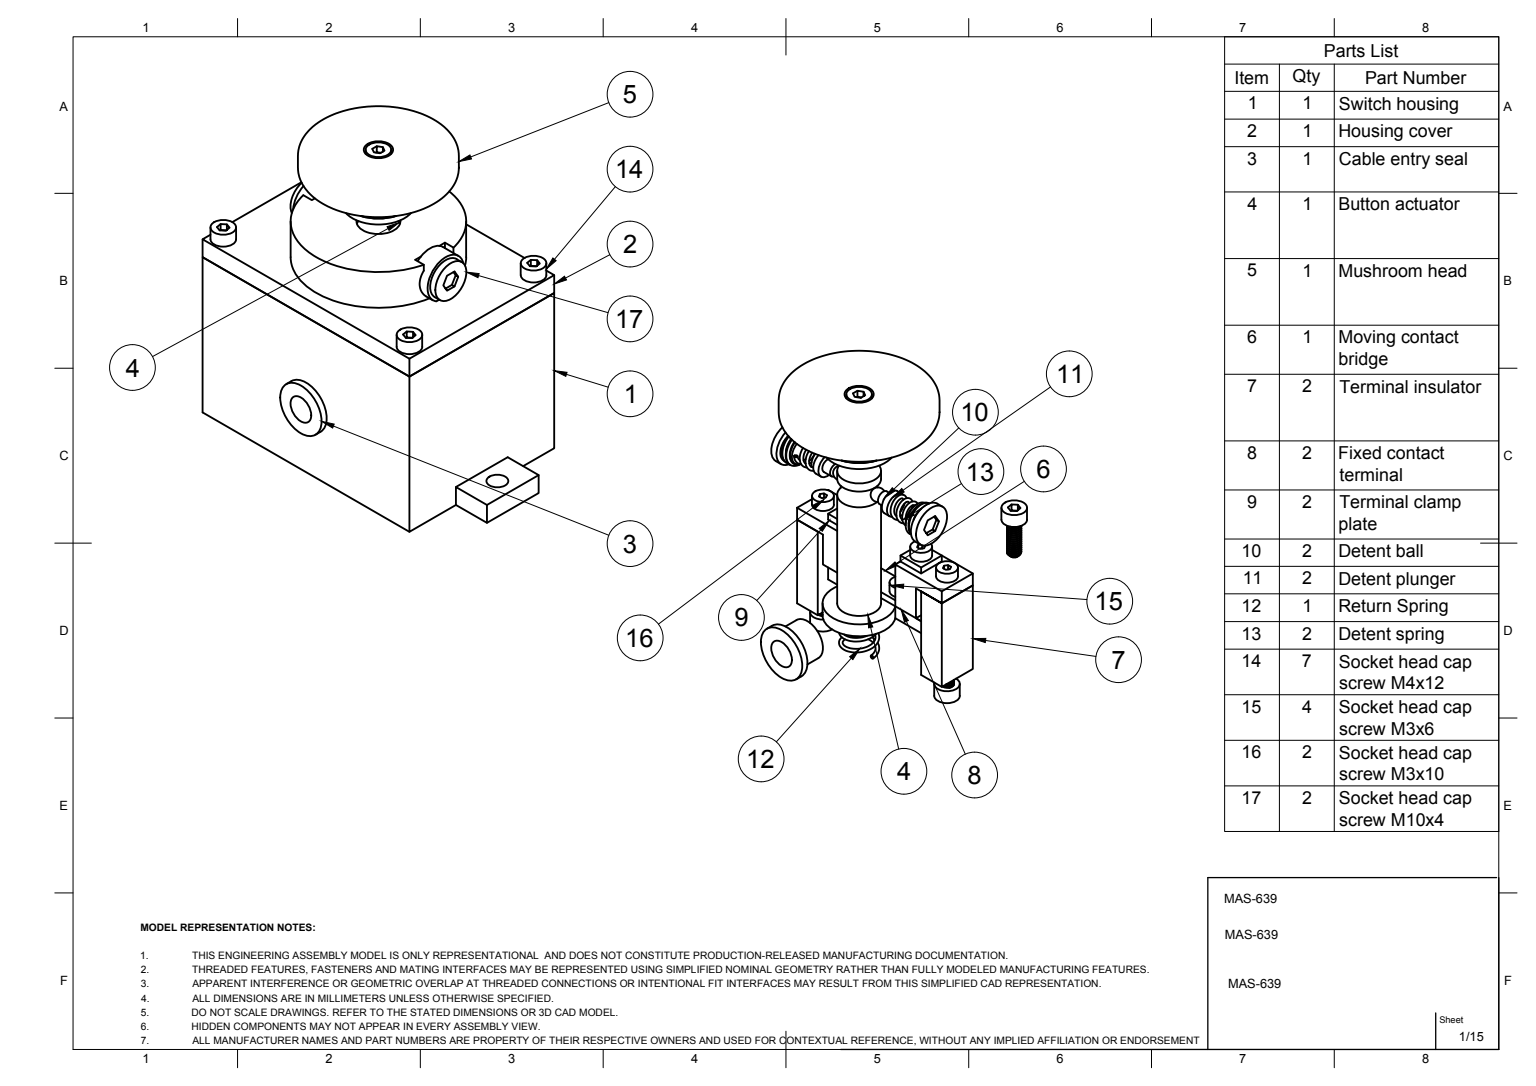
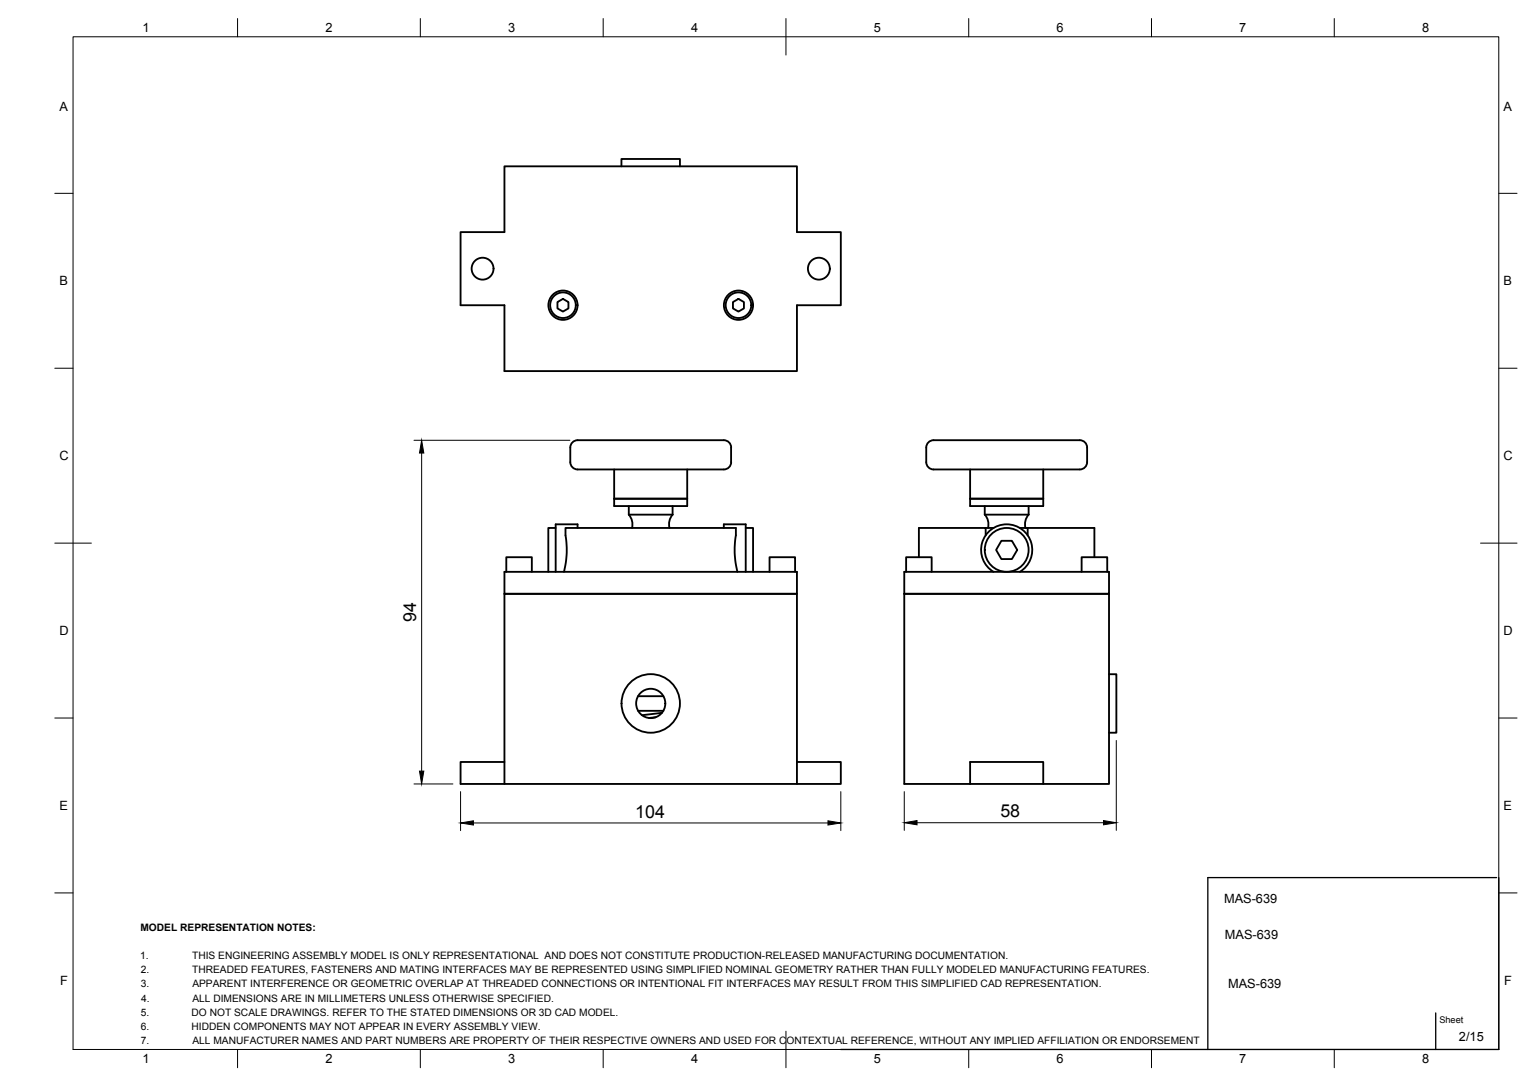
ISO-10303-21;
HEADER;
/* Generated by software containing ST-Developer
 * from STEP Tools, Inc. (www.steptools.com) 
 */

FILE_DESCRIPTION(
/* description */ ('Independent maintained push-to-latch/pull-to-reset mushroom-operator 
CAD. Two opposed spring-loaded ball detents in turned circular seats b
ias both travel stops; direct normally-closed bridge opens6mm when pre
ssed. Rounded palm/pull rim, captured head screw, removable detent clo
sures, native Coil spring families, insulated shared terminals and ord
inary machining features. Manual geometric states and ideal same-mater
ial spring-energy direction only; no electrical/safety certification, 
force/contact dynamics, wear, load or life rating. Requested blue/gray
 visual palette, not safety identification. External wiring/anchors an
d application engineering omitted.'),
/* implementation_level */ '2;1');

FILE_NAME(
/* name */ 'MAS-639.step',
/* time_stamp */ '2026-11-08T17:54:26-08:00',
/* author */ (''),
/* organization */ (''),
/* preprocessor_version */ 'ST-DEVELOPER v20.2',
/* originating_system */ 'Autodesk Translation Framework v15.17.0.0',
/* authorisation */ '');

FILE_SCHEMA (('AUTOMOTIVE_DESIGN { 1 0 10303 214 3 1 1 }'));
ENDSEC;

DATA;
#10=MECHANICAL_DESIGN_GEOMETRIC_PRESENTATION_REPRESENTATION('',(#190,#191,
#192,#193,#194,#195,#196,#197,#198,#199,#200,#201,#202,#203,#204,#205,#206),
#43980);
#11=ITEM_DEFINED_TRANSFORMATION($,$,#11437,#12233);
#12=ITEM_DEFINED_TRANSFORMATION($,$,#11636,#12234);
#13=ITEM_DEFINED_TRANSFORMATION($,$,#11727,#12235);
#14=ITEM_DEFINED_TRANSFORMATION($,$,#11740,#12236);
#15=ITEM_DEFINED_TRANSFORMATION($,$,#11851,#12237);
#16=ITEM_DEFINED_TRANSFORMATION($,$,#11878,#12238);
#17=ITEM_DEFINED_TRANSFORMATION($,$,#11896,#12239);
#18=ITEM_DEFINED_TRANSFORMATION($,$,#11983,#12240);
#19=ITEM_DEFINED_TRANSFORMATION($,$,#12025,#12241);
#20=ITEM_DEFINED_TRANSFORMATION($,$,#12035,#12242);
#21=ITEM_DEFINED_TRANSFORMATION($,$,#12038,#12243);
#22=ITEM_DEFINED_TRANSFORMATION($,$,#11891,#12244);
#23=ITEM_DEFINED_TRANSFORMATION($,$,#11896,#12245);
#24=ITEM_DEFINED_TRANSFORMATION($,$,#11983,#12246);
#25=ITEM_DEFINED_TRANSFORMATION($,$,#12025,#12247);
#26=ITEM_DEFINED_TRANSFORMATION($,$,#12035,#12248);
#27=ITEM_DEFINED_TRANSFORMATION($,$,#12038,#12249);
#28=ITEM_DEFINED_TRANSFORMATION($,$,#12048,#12250);
#29=ITEM_DEFINED_TRANSFORMATION($,$,#12053,#12251);
#30=ITEM_DEFINED_TRANSFORMATION($,$,#12107,#12252);
#31=ITEM_DEFINED_TRANSFORMATION($,$,#12149,#12253);
#32=ITEM_DEFINED_TRANSFORMATION($,$,#12207,#12254);
#33=ITEM_DEFINED_TRANSFORMATION($,$,#12048,#12255);
#34=ITEM_DEFINED_TRANSFORMATION($,$,#12053,#12256);
#35=ITEM_DEFINED_TRANSFORMATION($,$,#12053,#12257);
#36=ITEM_DEFINED_TRANSFORMATION($,$,#12053,#12258);
#37=ITEM_DEFINED_TRANSFORMATION($,$,#12053,#12259);
#38=ITEM_DEFINED_TRANSFORMATION($,$,#12053,#12260);
#39=ITEM_DEFINED_TRANSFORMATION($,$,#12053,#12261);
#40=ITEM_DEFINED_TRANSFORMATION($,$,#12107,#12262);
#41=ITEM_DEFINED_TRANSFORMATION($,$,#12107,#12263);
#42=ITEM_DEFINED_TRANSFORMATION($,$,#12107,#12264);
#43=ITEM_DEFINED_TRANSFORMATION($,$,#12149,#12265);
#44=ITEM_DEFINED_TRANSFORMATION($,$,#12207,#12266);
#45=(
REPRESENTATION_RELATIONSHIP($,$,#44056,#44055)
REPRESENTATION_RELATIONSHIP_WITH_TRANSFORMATION(#11)
SHAPE_REPRESENTATION_RELATIONSHIP()
);
#46=(
REPRESENTATION_RELATIONSHIP($,$,#44057,#44055)
REPRESENTATION_RELATIONSHIP_WITH_TRANSFORMATION(#12)
SHAPE_REPRESENTATION_RELATIONSHIP()
);
#47=(
REPRESENTATION_RELATIONSHIP($,$,#44058,#44055)
REPRESENTATION_RELATIONSHIP_WITH_TRANSFORMATION(#13)
SHAPE_REPRESENTATION_RELATIONSHIP()
);
#48=(
REPRESENTATION_RELATIONSHIP($,$,#44059,#44055)
REPRESENTATION_RELATIONSHIP_WITH_TRANSFORMATION(#14)
SHAPE_REPRESENTATION_RELATIONSHIP()
);
#49=(
REPRESENTATION_RELATIONSHIP($,$,#44060,#44055)
REPRESENTATION_RELATIONSHIP_WITH_TRANSFORMATION(#15)
SHAPE_REPRESENTATION_RELATIONSHIP()
);
#50=(
REPRESENTATION_RELATIONSHIP($,$,#44061,#44055)
REPRESENTATION_RELATIONSHIP_WITH_TRANSFORMATION(#16)
SHAPE_REPRESENTATION_RELATIONSHIP()
);
#51=(
REPRESENTATION_RELATIONSHIP($,$,#44063,#44055)
REPRESENTATION_RELATIONSHIP_WITH_TRANSFORMATION(#17)
SHAPE_REPRESENTATION_RELATIONSHIP()
);
#52=(
REPRESENTATION_RELATIONSHIP($,$,#44064,#44055)
REPRESENTATION_RELATIONSHIP_WITH_TRANSFORMATION(#18)
SHAPE_REPRESENTATION_RELATIONSHIP()
);
#53=(
REPRESENTATION_RELATIONSHIP($,$,#44065,#44055)
REPRESENTATION_RELATIONSHIP_WITH_TRANSFORMATION(#19)
SHAPE_REPRESENTATION_RELATIONSHIP()
);
#54=(
REPRESENTATION_RELATIONSHIP($,$,#44066,#44055)
REPRESENTATION_RELATIONSHIP_WITH_TRANSFORMATION(#20)
SHAPE_REPRESENTATION_RELATIONSHIP()
);
#55=(
REPRESENTATION_RELATIONSHIP($,$,#44067,#44055)
REPRESENTATION_RELATIONSHIP_WITH_TRANSFORMATION(#21)
SHAPE_REPRESENTATION_RELATIONSHIP()
);
#56=(
REPRESENTATION_RELATIONSHIP($,$,#44062,#44055)
REPRESENTATION_RELATIONSHIP_WITH_TRANSFORMATION(#22)
SHAPE_REPRESENTATION_RELATIONSHIP()
);
#57=(
REPRESENTATION_RELATIONSHIP($,$,#44063,#44055)
REPRESENTATION_RELATIONSHIP_WITH_TRANSFORMATION(#23)
SHAPE_REPRESENTATION_RELATIONSHIP()
);
#58=(
REPRESENTATION_RELATIONSHIP($,$,#44064,#44055)
REPRESENTATION_RELATIONSHIP_WITH_TRANSFORMATION(#24)
SHAPE_REPRESENTATION_RELATIONSHIP()
);
#59=(
REPRESENTATION_RELATIONSHIP($,$,#44065,#44055)
REPRESENTATION_RELATIONSHIP_WITH_TRANSFORMATION(#25)
SHAPE_REPRESENTATION_RELATIONSHIP()
);
#60=(
REPRESENTATION_RELATIONSHIP($,$,#44066,#44055)
REPRESENTATION_RELATIONSHIP_WITH_TRANSFORMATION(#26)
SHAPE_REPRESENTATION_RELATIONSHIP()
);
#61=(
REPRESENTATION_RELATIONSHIP($,$,#44067,#44055)
REPRESENTATION_RELATIONSHIP_WITH_TRANSFORMATION(#27)
SHAPE_REPRESENTATION_RELATIONSHIP()
);
#62=(
REPRESENTATION_RELATIONSHIP($,$,#44068,#44055)
REPRESENTATION_RELATIONSHIP_WITH_TRANSFORMATION(#28)
SHAPE_REPRESENTATION_RELATIONSHIP()
);
#63=(
REPRESENTATION_RELATIONSHIP($,$,#44069,#44055)
REPRESENTATION_RELATIONSHIP_WITH_TRANSFORMATION(#29)
SHAPE_REPRESENTATION_RELATIONSHIP()
);
#64=(
REPRESENTATION_RELATIONSHIP($,$,#44070,#44055)
REPRESENTATION_RELATIONSHIP_WITH_TRANSFORMATION(#30)
SHAPE_REPRESENTATION_RELATIONSHIP()
);
#65=(
REPRESENTATION_RELATIONSHIP($,$,#44071,#44055)
REPRESENTATION_RELATIONSHIP_WITH_TRANSFORMATION(#31)
SHAPE_REPRESENTATION_RELATIONSHIP()
);
#66=(
REPRESENTATION_RELATIONSHIP($,$,#44072,#44055)
REPRESENTATION_RELATIONSHIP_WITH_TRANSFORMATION(#32)
SHAPE_REPRESENTATION_RELATIONSHIP()
);
#67=(
REPRESENTATION_RELATIONSHIP($,$,#44068,#44055)
REPRESENTATION_RELATIONSHIP_WITH_TRANSFORMATION(#33)
SHAPE_REPRESENTATION_RELATIONSHIP()
);
#68=(
REPRESENTATION_RELATIONSHIP($,$,#44069,#44055)
REPRESENTATION_RELATIONSHIP_WITH_TRANSFORMATION(#34)
SHAPE_REPRESENTATION_RELATIONSHIP()
);
#69=(
REPRESENTATION_RELATIONSHIP($,$,#44069,#44055)
REPRESENTATION_RELATIONSHIP_WITH_TRANSFORMATION(#35)
SHAPE_REPRESENTATION_RELATIONSHIP()
);
#70=(
REPRESENTATION_RELATIONSHIP($,$,#44069,#44055)
REPRESENTATION_RELATIONSHIP_WITH_TRANSFORMATION(#36)
SHAPE_REPRESENTATION_RELATIONSHIP()
);
#71=(
REPRESENTATION_RELATIONSHIP($,$,#44069,#44055)
REPRESENTATION_RELATIONSHIP_WITH_TRANSFORMATION(#37)
SHAPE_REPRESENTATION_RELATIONSHIP()
);
#72=(
REPRESENTATION_RELATIONSHIP($,$,#44069,#44055)
REPRESENTATION_RELATIONSHIP_WITH_TRANSFORMATION(#38)
SHAPE_REPRESENTATION_RELATIONSHIP()
);
#73=(
REPRESENTATION_RELATIONSHIP($,$,#44069,#44055)
REPRESENTATION_RELATIONSHIP_WITH_TRANSFORMATION(#39)
SHAPE_REPRESENTATION_RELATIONSHIP()
);
#74=(
REPRESENTATION_RELATIONSHIP($,$,#44070,#44055)
REPRESENTATION_RELATIONSHIP_WITH_TRANSFORMATION(#40)
SHAPE_REPRESENTATION_RELATIONSHIP()
);
#75=(
REPRESENTATION_RELATIONSHIP($,$,#44070,#44055)
REPRESENTATION_RELATIONSHIP_WITH_TRANSFORMATION(#41)
SHAPE_REPRESENTATION_RELATIONSHIP()
);
#76=(
REPRESENTATION_RELATIONSHIP($,$,#44070,#44055)
REPRESENTATION_RELATIONSHIP_WITH_TRANSFORMATION(#42)
SHAPE_REPRESENTATION_RELATIONSHIP()
);
#77=(
REPRESENTATION_RELATIONSHIP($,$,#44071,#44055)
REPRESENTATION_RELATIONSHIP_WITH_TRANSFORMATION(#43)
SHAPE_REPRESENTATION_RELATIONSHIP()
);
#78=(
REPRESENTATION_RELATIONSHIP($,$,#44072,#44055)
REPRESENTATION_RELATIONSHIP_WITH_TRANSFORMATION(#44)
SHAPE_REPRESENTATION_RELATIONSHIP()
);
#79=CONTEXT_DEPENDENT_SHAPE_REPRESENTATION(#45,#44021);
#80=CONTEXT_DEPENDENT_SHAPE_REPRESENTATION(#46,#44022);
#81=CONTEXT_DEPENDENT_SHAPE_REPRESENTATION(#47,#44023);
#82=CONTEXT_DEPENDENT_SHAPE_REPRESENTATION(#48,#44024);
#83=CONTEXT_DEPENDENT_SHAPE_REPRESENTATION(#49,#44025);
#84=CONTEXT_DEPENDENT_SHAPE_REPRESENTATION(#50,#44026);
#85=CONTEXT_DEPENDENT_SHAPE_REPRESENTATION(#51,#44027);
#86=CONTEXT_DEPENDENT_SHAPE_REPRESENTATION(#52,#44028);
#87=CONTEXT_DEPENDENT_SHAPE_REPRESENTATION(#53,#44029);
#88=CONTEXT_DEPENDENT_SHAPE_REPRESENTATION(#54,#44030);
#89=CONTEXT_DEPENDENT_SHAPE_REPRESENTATION(#55,#44031);
#90=CONTEXT_DEPENDENT_SHAPE_REPRESENTATION(#56,#44032);
#91=CONTEXT_DEPENDENT_SHAPE_REPRESENTATION(#57,#44033);
#92=CONTEXT_DEPENDENT_SHAPE_REPRESENTATION(#58,#44034);
#93=CONTEXT_DEPENDENT_SHAPE_REPRESENTATION(#59,#44035);
#94=CONTEXT_DEPENDENT_SHAPE_REPRESENTATION(#60,#44036);
#95=CONTEXT_DEPENDENT_SHAPE_REPRESENTATION(#61,#44037);
#96=CONTEXT_DEPENDENT_SHAPE_REPRESENTATION(#62,#44038);
#97=CONTEXT_DEPENDENT_SHAPE_REPRESENTATION(#63,#44039);
#98=CONTEXT_DEPENDENT_SHAPE_REPRESENTATION(#64,#44040);
#99=CONTEXT_DEPENDENT_SHAPE_REPRESENTATION(#65,#44041);
#100=CONTEXT_DEPENDENT_SHAPE_REPRESENTATION(#66,#44042);
#101=CONTEXT_DEPENDENT_SHAPE_REPRESENTATION(#67,#44043);
#102=CONTEXT_DEPENDENT_SHAPE_REPRESENTATION(#68,#44044);
#103=CONTEXT_DEPENDENT_SHAPE_REPRESENTATION(#69,#44045);
#104=CONTEXT_DEPENDENT_SHAPE_REPRESENTATION(#70,#44046);
#105=CONTEXT_DEPENDENT_SHAPE_REPRESENTATION(#71,#44047);
#106=CONTEXT_DEPENDENT_SHAPE_REPRESENTATION(#72,#44048);
#107=CONTEXT_DEPENDENT_SHAPE_REPRESENTATION(#73,#44049);
#108=CONTEXT_DEPENDENT_SHAPE_REPRESENTATION(#74,#44050);
#109=CONTEXT_DEPENDENT_SHAPE_REPRESENTATION(#75,#44051);
#110=CONTEXT_DEPENDENT_SHAPE_REPRESENTATION(#76,#44052);
#111=CONTEXT_DEPENDENT_SHAPE_REPRESENTATION(#77,#44053);
#112=CONTEXT_DEPENDENT_SHAPE_REPRESENTATION(#78,#44054);
#113=NEXT_ASSEMBLY_USAGE_OCCURRENCE('Switch housing:1',
'Switch housing:1','Switch housing:1',#44074,#44075,'Switch housing:1');
#114=NEXT_ASSEMBLY_USAGE_OCCURRENCE('Housing cover:1','Housing cover:1',
'Housing cover:1',#44074,#44076,'Housing cover:1');
#115=NEXT_ASSEMBLY_USAGE_OCCURRENCE('Cable entry seal:1',
'Cable entry seal:1','Cable entry seal:1',#44074,#44077,
'Cable entry seal:1');
#116=NEXT_ASSEMBLY_USAGE_OCCURRENCE('Button actuator:1',
'Button actuator:1','Button actuator:1',#44074,#44078,
'Button actuator:1');
#117=NEXT_ASSEMBLY_USAGE_OCCURRENCE('Mushroom head:1','Mushroom head:1',
'Mushroom head:1',#44074,#44079,'Mushroom head:1');
#118=NEXT_ASSEMBLY_USAGE_OCCURRENCE('Moving contact bridge:1',
'Moving contact bridge:1','Moving contact bridge:1',#44074,#44080,
'Moving contact bridge:1');
#119=NEXT_ASSEMBLY_USAGE_OCCURRENCE('Terminal insulator:1',
'Terminal insulator:1','Terminal insulator:1',#44074,#44082,
'Terminal insulator:1');
#120=NEXT_ASSEMBLY_USAGE_OCCURRENCE('Fixed contact terminal:1',
'Fixed contact terminal:1','Fixed contact terminal:1',#44074,#44083,
'Fixed contact terminal:1');
#121=NEXT_ASSEMBLY_USAGE_OCCURRENCE('Terminal clamp plate:1',
'Terminal clamp plate:1','Terminal clamp plate:1',#44074,#44084,
'Terminal clamp plate:1');
#122=NEXT_ASSEMBLY_USAGE_OCCURRENCE('Detent ball:1','Detent ball:1',
'Detent ball:1',#44074,#44085,'Detent ball:1');
#123=NEXT_ASSEMBLY_USAGE_OCCURRENCE('Detent plunger:1',
'Detent plunger:1','Detent plunger:1',#44074,#44086,'Detent plunger:1');
#124=NEXT_ASSEMBLY_USAGE_OCCURRENCE('Return spring:1','Return spring:1',
'Return spring:1',#44074,#44081,'Return spring:1');
#125=NEXT_ASSEMBLY_USAGE_OCCURRENCE('Terminal insulator:2',
'Terminal insulator:2','Terminal insulator:2',#44074,#44082,
'Terminal insulator:2');
#126=NEXT_ASSEMBLY_USAGE_OCCURRENCE('Fixed contact terminal:2',
'Fixed contact terminal:2','Fixed contact terminal:2',#44074,#44083,
'Fixed contact terminal:2');
#127=NEXT_ASSEMBLY_USAGE_OCCURRENCE('Terminal clamp plate:2',
'Terminal clamp plate:2','Terminal clamp plate:2',#44074,#44084,
'Terminal clamp plate:2');
#128=NEXT_ASSEMBLY_USAGE_OCCURRENCE('Detent ball:2','Detent ball:2',
'Detent ball:2',#44074,#44085,'Detent ball:2');
#129=NEXT_ASSEMBLY_USAGE_OCCURRENCE('Detent plunger:2',
'Detent plunger:2','Detent plunger:2',#44074,#44086,'Detent plunger:2');
#130=NEXT_ASSEMBLY_USAGE_OCCURRENCE('Detent spring:1','Detent spring:1',
'Detent spring:1',#44074,#44087,'Detent spring:1');
#131=NEXT_ASSEMBLY_USAGE_OCCURRENCE('Socket head cap screw M4x12:1',
'Socket head cap screw M4x12:1','Socket head cap screw M4x12:1',#44074,
#44088,'Socket head cap screw M4x12:1');
#132=NEXT_ASSEMBLY_USAGE_OCCURRENCE('Socket head cap screw M3x6:1',
'Socket head cap screw M3x6:1','Socket head cap screw M3x6:1',#44074,#44089,
'Socket head cap screw M3x6:1');
#133=NEXT_ASSEMBLY_USAGE_OCCURRENCE('Socket head cap screw M3x10:1',
'Socket head cap screw M3x10:1','Socket head cap screw M3x10:1',#44074,
#44090,'Socket head cap screw M3x10:1');
#134=NEXT_ASSEMBLY_USAGE_OCCURRENCE('Socket head cap screw M10x4:1',
'Socket head cap screw M10x4:1','Socket head cap screw M10x4:1',#44074,
#44091,'Socket head cap screw M10x4:1');
#135=NEXT_ASSEMBLY_USAGE_OCCURRENCE('Detent spring:2','Detent spring:2',
'Detent spring:2',#44074,#44087,'Detent spring:2');
#136=NEXT_ASSEMBLY_USAGE_OCCURRENCE('Socket head cap screw M4x12:2',
'Socket head cap screw M4x12:2','Socket head cap screw M4x12:2',#44074,
#44088,'Socket head cap screw M4x12:2');
#137=NEXT_ASSEMBLY_USAGE_OCCURRENCE('Socket head cap screw M4x12:3',
'Socket head cap screw M4x12:3','Socket head cap screw M4x12:3',#44074,
#44088,'Socket head cap screw M4x12:3');
#138=NEXT_ASSEMBLY_USAGE_OCCURRENCE('Socket head cap screw M4x12:4',
'Socket head cap screw M4x12:4','Socket head cap screw M4x12:4',#44074,
#44088,'Socket head cap screw M4x12:4');
#139=NEXT_ASSEMBLY_USAGE_OCCURRENCE('Socket head cap screw M4x12:5',
'Socket head cap screw M4x12:5','Socket head cap screw M4x12:5',#44074,
#44088,'Socket head cap screw M4x12:5');
#140=NEXT_ASSEMBLY_USAGE_OCCURRENCE('Socket head cap screw M4x12:6',
'Socket head cap screw M4x12:6','Socket head cap screw M4x12:6',#44074,
#44088,'Socket head cap screw M4x12:6');
#141=NEXT_ASSEMBLY_USAGE_OCCURRENCE('Socket head cap screw M4x12:7',
'Socket head cap screw M4x12:7','Socket head cap screw M4x12:7',#44074,
#44088,'Socket head cap screw M4x12:7');
#142=NEXT_ASSEMBLY_USAGE_OCCURRENCE('Socket head cap screw M3x6:2',
'Socket head cap screw M3x6:2','Socket head cap screw M3x6:2',#44074,#44089,
'Socket head cap screw M3x6:2');
#143=NEXT_ASSEMBLY_USAGE_OCCURRENCE('Socket head cap screw M3x6:3',
'Socket head cap screw M3x6:3','Socket head cap screw M3x6:3',#44074,#44089,
'Socket head cap screw M3x6:3');
#144=NEXT_ASSEMBLY_USAGE_OCCURRENCE('Socket head cap screw M3x6:4',
'Socket head cap screw M3x6:4','Socket head cap screw M3x6:4',#44074,#44089,
'Socket head cap screw M3x6:4');
#145=NEXT_ASSEMBLY_USAGE_OCCURRENCE('Socket head cap screw M3x10:2',
'Socket head cap screw M3x10:2','Socket head cap screw M3x10:2',#44074,
#44090,'Socket head cap screw M3x10:2');
#146=NEXT_ASSEMBLY_USAGE_OCCURRENCE('Socket head cap screw M10x4:2',
'Socket head cap screw M10x4:2','Socket head cap screw M10x4:2',#44074,
#44091,'Socket head cap screw M10x4:2');
#147=CONICAL_SURFACE('',#12088,0.15,0.785398163397449);
#148=CONICAL_SURFACE('',#12130,0.1,0.785398163397448);
#149=CONICAL_SURFACE('',#12188,0.1,0.785398163397448);
#150=CONICAL_SURFACE('',#12214,0.45,0.785398163397448);
#151=SPHERICAL_SURFACE('',#12036,0.2);
#152=TOROIDAL_SURFACE('',#11821,0.899999999999998,0.399999999999998);
#153=TOROIDAL_SURFACE('',#11827,0.900000000000001,0.4);
#154=TOROIDAL_SURFACE('',#11852,2.,0.2);
#155=TOROIDAL_SURFACE('',#11860,2.,0.2);
#156=SHAPE_REPRESENTATION_RELATIONSHIP('SRR','None',#44056,#173);
#157=SHAPE_REPRESENTATION_RELATIONSHIP('SRR','None',#44057,#174);
#158=SHAPE_REPRESENTATION_RELATIONSHIP('SRR','None',#44058,#175);
#159=SHAPE_REPRESENTATION_RELATIONSHIP('SRR','None',#44059,#176);
#160=SHAPE_REPRESENTATION_RELATIONSHIP('SRR','None',#44060,#177);
#161=SHAPE_REPRESENTATION_RELATIONSHIP('SRR','None',#44061,#178);
#162=SHAPE_REPRESENTATION_RELATIONSHIP('SRR','None',#44062,#179);
#163=SHAPE_REPRESENTATION_RELATIONSHIP('SRR','None',#44063,#180);
#164=SHAPE_REPRESENTATION_RELATIONSHIP('SRR','None',#44064,#181);
#165=SHAPE_REPRESENTATION_RELATIONSHIP('SRR','None',#44065,#182);
#166=SHAPE_REPRESENTATION_RELATIONSHIP('SRR','None',#44066,#183);
#167=SHAPE_REPRESENTATION_RELATIONSHIP('SRR','None',#44067,#184);
#168=SHAPE_REPRESENTATION_RELATIONSHIP('SRR','None',#44068,#185);
#169=SHAPE_REPRESENTATION_RELATIONSHIP('SRR','None',#44069,#186);
#170=SHAPE_REPRESENTATION_RELATIONSHIP('SRR','None',#44070,#187);
#171=SHAPE_REPRESENTATION_RELATIONSHIP('SRR','None',#44071,#188);
#172=SHAPE_REPRESENTATION_RELATIONSHIP('SRR','None',#44072,#189);
#173=ADVANCED_BREP_SHAPE_REPRESENTATION('',(#207),#43963);
#174=ADVANCED_BREP_SHAPE_REPRESENTATION('',(#208),#43964);
#175=ADVANCED_BREP_SHAPE_REPRESENTATION('',(#209),#43965);
#176=ADVANCED_BREP_SHAPE_REPRESENTATION('',(#210),#43966);
#177=ADVANCED_BREP_SHAPE_REPRESENTATION('',(#211),#43967);
#178=ADVANCED_BREP_SHAPE_REPRESENTATION('',(#212),#43968);
#179=ADVANCED_BREP_SHAPE_REPRESENTATION('',(#213),#43969);
#180=ADVANCED_BREP_SHAPE_REPRESENTATION('',(#214),#43970);
#181=ADVANCED_BREP_SHAPE_REPRESENTATION('',(#215),#43971);
#182=ADVANCED_BREP_SHAPE_REPRESENTATION('',(#216),#43972);
#183=ADVANCED_BREP_SHAPE_REPRESENTATION('',(#217),#43973);
#184=ADVANCED_BREP_SHAPE_REPRESENTATION('',(#218),#43974);
#185=ADVANCED_BREP_SHAPE_REPRESENTATION('',(#219),#43975);
#186=ADVANCED_BREP_SHAPE_REPRESENTATION('',(#220),#43976);
#187=ADVANCED_BREP_SHAPE_REPRESENTATION('',(#221),#43977);
#188=ADVANCED_BREP_SHAPE_REPRESENTATION('',(#222),#43978);
#189=ADVANCED_BREP_SHAPE_REPRESENTATION('',(#223),#43979);
#190=STYLED_ITEM('',(#44150),#207);
#191=STYLED_ITEM('',(#44151),#208);
#192=STYLED_ITEM('',(#44152),#209);
#193=STYLED_ITEM('',(#44153),#210);
#194=STYLED_ITEM('',(#44150),#211);
#195=STYLED_ITEM('',(#44154),#212);
#196=STYLED_ITEM('',(#44155),#213);
#197=STYLED_ITEM('',(#44156),#214);
#198=STYLED_ITEM('',(#44154),#215);
#199=STYLED_ITEM('',(#44157),#216);
#200=STYLED_ITEM('',(#44158),#217);
#201=STYLED_ITEM('',(#44159),#218);
#202=STYLED_ITEM('',(#44155),#219);
#203=STYLED_ITEM('',(#44160),#220);
#204=STYLED_ITEM('',(#44160),#221);
#205=STYLED_ITEM('',(#44160),#222);
#206=STYLED_ITEM('',(#44160),#223);
#207=MANIFOLD_SOLID_BREP('Body1',#11231);
#208=MANIFOLD_SOLID_BREP('Body1',#11232);
#209=MANIFOLD_SOLID_BREP('Body1',#11233);
#210=MANIFOLD_SOLID_BREP('Body1',#11234);
#211=MANIFOLD_SOLID_BREP('Body1',#11235);
#212=MANIFOLD_SOLID_BREP('Body1',#11236);
#213=MANIFOLD_SOLID_BREP('Body1',#11237);
#214=MANIFOLD_SOLID_BREP('Body1',#11238);
#215=MANIFOLD_SOLID_BREP('Body1',#11239);
#216=MANIFOLD_SOLID_BREP('Body1',#11240);
#217=MANIFOLD_SOLID_BREP('Body1',#11241);
#218=MANIFOLD_SOLID_BREP('Body1',#11242);
#219=MANIFOLD_SOLID_BREP('Body1',#11243);
#220=MANIFOLD_SOLID_BREP('Body1',#11244);
#221=MANIFOLD_SOLID_BREP('Body1',#11245);
#222=MANIFOLD_SOLID_BREP('Body1',#11246);
#223=MANIFOLD_SOLID_BREP('Body1',#11247);
#224=B_SPLINE_SURFACE_WITH_KNOTS('',3,3,((#18348,#18349,#18350,#18351,#18352,
#18353,#18354,#18355,#18356,#18357,#18358,#18359,#18360,#18361,#18362,#18363,
#18364,#18365,#18366,#18367,#18368,#18369,#18370,#18371,#18372,#18373,#18374,
#18375,#18376,#18377,#18378,#18379,#18380,#18381,#18382,#18383,#18384,#18385,
#18386,#18387,#18388,#18389,#18390,#18391,#18392,#18393,#18394,#18395,#18396,
#18397,#18398,#18399,#18400,#18401,#18402,#18403,#18404,#18405,#18406,#18407,
#18408,#18409,#18410,#18411,#18412,#18413,#18414,#18415,#18416,#18417,#18418,
#18419,#18420,#18421,#18422,#18423,#18424,#18425,#18426,#18427,#18428,#18429,
#18430,#18431,#18432,#18433),(#18434,#18435,#18436,#18437,#18438,#18439,
#18440,#18441,#18442,#18443,#18444,#18445,#18446,#18447,#18448,#18449,#18450,
#18451,#18452,#18453,#18454,#18455,#18456,#18457,#18458,#18459,#18460,#18461,
#18462,#18463,#18464,#18465,#18466,#18467,#18468,#18469,#18470,#18471,#18472,
#18473,#18474,#18475,#18476,#18477,#18478,#18479,#18480,#18481,#18482,#18483,
#18484,#18485,#18486,#18487,#18488,#18489,#18490,#18491,#18492,#18493,#18494,
#18495,#18496,#18497,#18498,#18499,#18500,#18501,#18502,#18503,#18504,#18505,
#18506,#18507,#18508,#18509,#18510,#18511,#18512,#18513,#18514,#18515,#18516,
#18517,#18518,#18519),(#18520,#18521,#18522,#18523,#18524,#18525,#18526,
#18527,#18528,#18529,#18530,#18531,#18532,#18533,#18534,#18535,#18536,#18537,
#18538,#18539,#18540,#18541,#18542,#18543,#18544,#18545,#18546,#18547,#18548,
#18549,#18550,#18551,#18552,#18553,#18554,#18555,#18556,#18557,#18558,#18559,
#18560,#18561,#18562,#18563,#18564,#18565,#18566,#18567,#18568,#18569,#18570,
#18571,#18572,#18573,#18574,#18575,#18576,#18577,#18578,#18579,#18580,#18581,
#18582,#18583,#18584,#18585,#18586,#18587,#18588,#18589,#18590,#18591,#18592,
#18593,#18594,#18595,#18596,#18597,#18598,#18599,#18600,#18601,#18602,#18603,
#18604,#18605),(#18606,#18607,#18608,#18609,#18610,#18611,#18612,#18613,
#18614,#18615,#18616,#18617,#18618,#18619,#18620,#18621,#18622,#18623,#18624,
#18625,#18626,#18627,#18628,#18629,#18630,#18631,#18632,#18633,#18634,#18635,
#18636,#18637,#18638,#18639,#18640,#18641,#18642,#18643,#18644,#18645,#18646,
#18647,#18648,#18649,#18650,#18651,#18652,#18653,#18654,#18655,#18656,#18657,
#18658,#18659,#18660,#18661,#18662,#18663,#18664,#18665,#18666,#18667,#18668,
#18669,#18670,#18671,#18672,#18673,#18674,#18675,#18676,#18677,#18678,#18679,
#18680,#18681,#18682,#18683,#18684,#18685,#18686,#18687,#18688,#18689,#18690,
#18691)),.UNSPECIFIED.,.F.,.F.,.F.,(4,4),(4,1,1,1,1,1,1,1,1,1,1,1,1,1,1,
1,1,1,1,1,1,1,1,1,1,1,1,1,1,1,1,1,1,1,1,1,1,1,1,1,1,1,1,1,1,1,1,1,1,1,1,
1,1,1,1,1,1,1,1,1,1,1,1,1,1,1,1,1,1,1,1,1,1,1,1,1,1,1,1,1,1,1,1,4),(0.,
0.0448889834294937),(11.8615800042567,12.8591513772396,13.8567227502226,
14.8542941232055,15.8518654961884,16.8494368691714,17.8470082421543,18.8445796151372,
19.8421509881202,20.8397223611031,21.837293734086,22.834865107069,23.8324364800519,
24.8300078530348,25.8275792260178,26.8251505990007,27.8227219719836,28.8202933449666,
29.8178647179495,30.8154360909324,31.8130074639154,32.8105788368983,33.8081502098812,
34.8057215828642,35.8032929558471,36.80086432883,37.798435701813,38.7960070747959,
39.7935784477789,40.7911498207618,41.7887211937447,42.7862925667277,43.7838639397106,
44.7814353126935,45.7790066856765,46.7765780586594,47.7741494316423,48.7717208046253,
49.7692921776082,50.7668635505911,51.7644349235741,52.762006296557,53.7595776695399,
54.7571490425229,55.7547204155058,56.7522917884887,57.7498631614717,58.7474345344546,
59.7450059074375,60.7425772804205,61.7401486534034,62.7377200263864,63.7352913993693,
64.7328627723522,65.7304341453352,66.7280055183181,67.725576891301,68.723148264284,
69.7207196372669,70.7182910102498,71.7158623832328,72.7134337562157,73.7110051291986,
74.7085765021816,75.7061478751645,76.7037192481474,77.7012906211304,78.6988619941133,
79.6964333670962,80.6940047400792,81.6915761130621,82.689147486045,83.686718859028,
84.6842902320109,85.6818616049939,86.6794329779768,87.6770043509597,88.6745757239427,
89.6721470969256,90.6697184699085,91.6672898428915,92.6648612158744,93.6624325888573,
94.6600039618403),.UNSPECIFIED.);
#225=B_SPLINE_SURFACE_WITH_KNOTS('',3,3,((#18769,#18770,#18771,#18772,#18773,
#18774,#18775,#18776,#18777,#18778,#18779,#18780,#18781,#18782,#18783,#18784,
#18785,#18786,#18787,#18788,#18789,#18790,#18791,#18792,#18793,#18794,#18795,
#18796,#18797,#18798,#18799,#18800,#18801,#18802,#18803,#18804,#18805,#18806,
#18807,#18808,#18809,#18810,#18811,#18812,#18813,#18814,#18815,#18816,#18817,
#18818,#18819,#18820,#18821,#18822,#18823,#18824,#18825,#18826,#18827,#18828,
#18829,#18830,#18831,#18832,#18833,#18834,#18835,#18836,#18837,#18838,#18839,
#18840,#18841,#18842,#18843,#18844,#18845,#18846,#18847,#18848,#18849,#18850,
#18851,#18852,#18853,#18854),(#18855,#18856,#18857,#18858,#18859,#18860,
#18861,#18862,#18863,#18864,#18865,#18866,#18867,#18868,#18869,#18870,#18871,
#18872,#18873,#18874,#18875,#18876,#18877,#18878,#18879,#18880,#18881,#18882,
#18883,#18884,#18885,#18886,#18887,#18888,#18889,#18890,#18891,#18892,#18893,
#18894,#18895,#18896,#18897,#18898,#18899,#18900,#18901,#18902,#18903,#18904,
#18905,#18906,#18907,#18908,#18909,#18910,#18911,#18912,#18913,#18914,#18915,
#18916,#18917,#18918,#18919,#18920,#18921,#18922,#18923,#18924,#18925,#18926,
#18927,#18928,#18929,#18930,#18931,#18932,#18933,#18934,#18935,#18936,#18937,
#18938,#18939,#18940),(#18941,#18942,#18943,#18944,#18945,#18946,#18947,
#18948,#18949,#18950,#18951,#18952,#18953,#18954,#18955,#18956,#18957,#18958,
#18959,#18960,#18961,#18962,#18963,#18964,#18965,#18966,#18967,#18968,#18969,
#18970,#18971,#18972,#18973,#18974,#18975,#18976,#18977,#18978,#18979,#18980,
#18981,#18982,#18983,#18984,#18985,#18986,#18987,#18988,#18989,#18990,#18991,
#18992,#18993,#18994,#18995,#18996,#18997,#18998,#18999,#19000,#19001,#19002,
#19003,#19004,#19005,#19006,#19007,#19008,#19009,#19010,#19011,#19012,#19013,
#19014,#19015,#19016,#19017,#19018,#19019,#19020,#19021,#19022,#19023,#19024,
#19025,#19026),(#19027,#19028,#19029,#19030,#19031,#19032,#19033,#19034,
#19035,#19036,#19037,#19038,#19039,#19040,#19041,#19042,#19043,#19044,#19045,
#19046,#19047,#19048,#19049,#19050,#19051,#19052,#19053,#19054,#19055,#19056,
#19057,#19058,#19059,#19060,#19061,#19062,#19063,#19064,#19065,#19066,#19067,
#19068,#19069,#19070,#19071,#19072,#19073,#19074,#19075,#19076,#19077,#19078,
#19079,#19080,#19081,#19082,#19083,#19084,#19085,#19086,#19087,#19088,#19089,
#19090,#19091,#19092,#19093,#19094,#19095,#19096,#19097,#19098,#19099,#19100,
#19101,#19102,#19103,#19104,#19105,#19106,#19107,#19108,#19109,#19110,#19111,
#19112)),.UNSPECIFIED.,.F.,.F.,.F.,(4,4),(4,1,1,1,1,1,1,1,1,1,1,1,1,1,1,
1,1,1,1,1,1,1,1,1,1,1,1,1,1,1,1,1,1,1,1,1,1,1,1,1,1,1,1,1,1,1,1,1,1,1,1,
1,1,1,1,1,1,1,1,1,1,1,1,1,1,1,1,1,1,1,1,1,1,1,1,1,1,1,1,1,1,1,1,4),(0.,
0.0448889834294937),(14.3981410127769,15.3957123857599,16.3932837587428,
17.3908551317257,18.3884265047087,19.3859978776916,20.3835692506745,21.3811406236575,
22.3787119966404,23.3762833696233,24.3738547426063,25.3714261155892,26.3689974885721,
27.3665688615551,28.364140234538,29.3617116075209,30.3592829805039,31.3568543534868,
32.3544257264697,33.3519970994527,34.3495684724356,35.3471398454185,36.3447112184015,
37.3422825913844,38.3398539643674,39.3374253373503,40.3349967103332,41.3325680833162,
42.3301394562991,43.327710829282,44.325282202265,45.3228535752479,46.3204249482308,
47.3179963212138,48.3155676941967,49.3131390671796,50.3107104401626,51.3082818131455,
52.3058531861284,53.3034245591114,54.3009959320943,55.2985673050772,56.2961386780602,
57.2937100510431,58.291281424026,59.288852797009,60.2864241699919,61.2839955429748,
62.2815669159578,63.2791382889407,64.2767096619236,65.2742810349066,66.2718524078895,
67.2694237808725,68.2669951538554,69.2645665268383,70.2621378998213,71.2597092728042,
72.2572806457871,73.2548520187701,74.252423391753,75.2499947647359,76.2475661377189,
77.2451375107018,78.2427088836847,79.2402802566677,80.2378516296506,81.2354230026336,
82.2329943756165,83.2305657485994,84.2281371215823,85.2257084945653,86.2232798675482,
87.2208512405312,88.2184226135141,89.215993986497,90.21356535948,91.2111367324629,
92.2087081054458,93.2062794784288,94.2038508514117,95.2014222243946,96.1989935973776,
97.1965649703605),.UNSPECIFIED.);
#226=B_SPLINE_SURFACE_WITH_KNOTS('',3,3,((#19321,#19322,#19323,#19324,#19325,
#19326,#19327,#19328,#19329,#19330,#19331,#19332,#19333,#19334,#19335,#19336,
#19337,#19338,#19339,#19340,#19341,#19342,#19343,#19344,#19345,#19346,#19347,
#19348,#19349,#19350,#19351,#19352,#19353,#19354,#19355,#19356,#19357,#19358,
#19359,#19360,#19361,#19362,#19363,#19364,#19365,#19366,#19367,#19368,#19369,
#19370,#19371,#19372,#19373,#19374,#19375,#19376,#19377,#19378,#19379,#19380,
#19381,#19382,#19383,#19384,#19385,#19386,#19387,#19388,#19389,#19390,#19391,
#19392,#19393,#19394,#19395,#19396,#19397,#19398,#19399,#19400,#19401,#19402,
#19403,#19404,#19405,#19406),(#19407,#19408,#19409,#19410,#19411,#19412,
#19413,#19414,#19415,#19416,#19417,#19418,#19419,#19420,#19421,#19422,#19423,
#19424,#19425,#19426,#19427,#19428,#19429,#19430,#19431,#19432,#19433,#19434,
#19435,#19436,#19437,#19438,#19439,#19440,#19441,#19442,#19443,#19444,#19445,
#19446,#19447,#19448,#19449,#19450,#19451,#19452,#19453,#19454,#19455,#19456,
#19457,#19458,#19459,#19460,#19461,#19462,#19463,#19464,#19465,#19466,#19467,
#19468,#19469,#19470,#19471,#19472,#19473,#19474,#19475,#19476,#19477,#19478,
#19479,#19480,#19481,#19482,#19483,#19484,#19485,#19486,#19487,#19488,#19489,
#19490,#19491,#19492),(#19493,#19494,#19495,#19496,#19497,#19498,#19499,
#19500,#19501,#19502,#19503,#19504,#19505,#19506,#19507,#19508,#19509,#19510,
#19511,#19512,#19513,#19514,#19515,#19516,#19517,#19518,#19519,#19520,#19521,
#19522,#19523,#19524,#19525,#19526,#19527,#19528,#19529,#19530,#19531,#19532,
#19533,#19534,#19535,#19536,#19537,#19538,#19539,#19540,#19541,#19542,#19543,
#19544,#19545,#19546,#19547,#19548,#19549,#19550,#19551,#19552,#19553,#19554,
#19555,#19556,#19557,#19558,#19559,#19560,#19561,#19562,#19563,#19564,#19565,
#19566,#19567,#19568,#19569,#19570,#19571,#19572,#19573,#19574,#19575,#19576,
#19577,#19578),(#19579,#19580,#19581,#19582,#19583,#19584,#19585,#19586,
#19587,#19588,#19589,#19590,#19591,#19592,#19593,#19594,#19595,#19596,#19597,
#19598,#19599,#19600,#19601,#19602,#19603,#19604,#19605,#19606,#19607,#19608,
#19609,#19610,#19611,#19612,#19613,#19614,#19615,#19616,#19617,#19618,#19619,
#19620,#19621,#19622,#19623,#19624,#19625,#19626,#19627,#19628,#19629,#19630,
#19631,#19632,#19633,#19634,#19635,#19636,#19637,#19638,#19639,#19640,#19641,
#19642,#19643,#19644,#19645,#19646,#19647,#19648,#19649,#19650,#19651,#19652,
#19653,#19654,#19655,#19656,#19657,#19658,#19659,#19660,#19661,#19662,#19663,
#19664)),.UNSPECIFIED.,.F.,.F.,.F.,(4,4),(4,1,1,1,1,1,1,1,1,1,1,1,1,1,1,
1,1,1,1,1,1,1,1,1,1,1,1,1,1,1,1,1,1,1,1,1,1,1,1,1,1,1,1,1,1,1,1,1,1,1,1,
1,1,1,1,1,1,1,1,1,1,1,1,1,1,1,1,1,1,1,1,1,1,1,1,1,1,1,1,1,1,1,1,4),(0.,
0.0448889834294937),(11.8615800042567,12.8591513772396,13.8567227502225,
14.8542941232055,15.8518654961884,16.8494368691713,17.8470082421543,18.8445796151372,
19.8421509881202,20.8397223611031,21.837293734086,22.834865107069,23.8324364800519,
24.8300078530348,25.8275792260178,26.8251505990007,27.8227219719836,28.8202933449666,
29.8178647179495,30.8154360909324,31.8130074639154,32.8105788368983,33.8081502098812,
34.8057215828642,35.8032929558471,36.80086432883,37.798435701813,38.7960070747959,
39.7935784477788,40.7911498207618,41.7887211937447,42.7862925667276,43.7838639397106,
44.7814353126935,45.7790066856764,46.7765780586594,47.7741494316423,48.7717208046252,
49.7692921776082,50.7668635505911,51.764434923574,52.762006296557,53.7595776695399,
54.7571490425228,55.7547204155058,56.7522917884887,57.7498631614716,58.7474345344546,
59.7450059074375,60.7425772804204,61.7401486534034,62.7377200263863,63.7352913993692,
64.7328627723522,65.7304341453351,66.728005518318,67.725576891301,68.7231482642839,
69.7207196372669,70.7182910102498,71.7158623832327,72.7134337562156,73.7110051291986,
74.7085765021815,75.7061478751644,76.7037192481474,77.7012906211303,78.6988619941132,
79.6964333670962,80.6940047400791,81.6915761130621,82.689147486045,83.6867188590279,
84.6842902320109,85.6818616049938,86.6794329779767,87.6770043509596,88.6745757239426,
89.6721470969255,90.6697184699085,91.6672898428914,92.6648612158743,93.6624325888573,
94.6600039618402),.UNSPECIFIED.);
#227=B_SPLINE_SURFACE_WITH_KNOTS('',3,3,((#19742,#19743,#19744,#19745,#19746,
#19747,#19748,#19749,#19750,#19751,#19752,#19753,#19754,#19755,#19756,#19757,
#19758,#19759,#19760,#19761,#19762,#19763,#19764,#19765,#19766,#19767,#19768,
#19769,#19770,#19771,#19772,#19773,#19774,#19775,#19776,#19777,#19778,#19779,
#19780,#19781,#19782,#19783,#19784,#19785,#19786,#19787,#19788,#19789,#19790,
#19791,#19792,#19793,#19794,#19795,#19796,#19797,#19798,#19799,#19800,#19801,
#19802,#19803,#19804,#19805,#19806,#19807,#19808,#19809,#19810,#19811,#19812,
#19813,#19814,#19815,#19816,#19817,#19818,#19819,#19820,#19821,#19822,#19823,
#19824,#19825,#19826,#19827),(#19828,#19829,#19830,#19831,#19832,#19833,
#19834,#19835,#19836,#19837,#19838,#19839,#19840,#19841,#19842,#19843,#19844,
#19845,#19846,#19847,#19848,#19849,#19850,#19851,#19852,#19853,#19854,#19855,
#19856,#19857,#19858,#19859,#19860,#19861,#19862,#19863,#19864,#19865,#19866,
#19867,#19868,#19869,#19870,#19871,#19872,#19873,#19874,#19875,#19876,#19877,
#19878,#19879,#19880,#19881,#19882,#19883,#19884,#19885,#19886,#19887,#19888,
#19889,#19890,#19891,#19892,#19893,#19894,#19895,#19896,#19897,#19898,#19899,
#19900,#19901,#19902,#19903,#19904,#19905,#19906,#19907,#19908,#19909,#19910,
#19911,#19912,#19913),(#19914,#19915,#19916,#19917,#19918,#19919,#19920,
#19921,#19922,#19923,#19924,#19925,#19926,#19927,#19928,#19929,#19930,#19931,
#19932,#19933,#19934,#19935,#19936,#19937,#19938,#19939,#19940,#19941,#19942,
#19943,#19944,#19945,#19946,#19947,#19948,#19949,#19950,#19951,#19952,#19953,
#19954,#19955,#19956,#19957,#19958,#19959,#19960,#19961,#19962,#19963,#19964,
#19965,#19966,#19967,#19968,#19969,#19970,#19971,#19972,#19973,#19974,#19975,
#19976,#19977,#19978,#19979,#19980,#19981,#19982,#19983,#19984,#19985,#19986,
#19987,#19988,#19989,#19990,#19991,#19992,#19993,#19994,#19995,#19996,#19997,
#19998,#19999),(#20000,#20001,#20002,#20003,#20004,#20005,#20006,#20007,
#20008,#20009,#20010,#20011,#20012,#20013,#20014,#20015,#20016,#20017,#20018,
#20019,#20020,#20021,#20022,#20023,#20024,#20025,#20026,#20027,#20028,#20029,
#20030,#20031,#20032,#20033,#20034,#20035,#20036,#20037,#20038,#20039,#20040,
#20041,#20042,#20043,#20044,#20045,#20046,#20047,#20048,#20049,#20050,#20051,
#20052,#20053,#20054,#20055,#20056,#20057,#20058,#20059,#20060,#20061,#20062,
#20063,#20064,#20065,#20066,#20067,#20068,#20069,#20070,#20071,#20072,#20073,
#20074,#20075,#20076,#20077,#20078,#20079,#20080,#20081,#20082,#20083,#20084,
#20085)),.UNSPECIFIED.,.F.,.F.,.F.,(4,4),(4,1,1,1,1,1,1,1,1,1,1,1,1,1,1,
1,1,1,1,1,1,1,1,1,1,1,1,1,1,1,1,1,1,1,1,1,1,1,1,1,1,1,1,1,1,1,1,1,1,1,1,
1,1,1,1,1,1,1,1,1,1,1,1,1,1,1,1,1,1,1,1,1,1,1,1,1,1,1,1,1,1,1,1,4),(0.,
0.0448889834294937),(14.3981410127769,15.3957123857599,16.3932837587428,
17.3908551317257,18.3884265047087,19.3859978776916,20.3835692506745,21.3811406236575,
22.3787119966404,23.3762833696233,24.3738547426063,25.3714261155892,26.3689974885721,
27.3665688615551,28.364140234538,29.3617116075209,30.3592829805039,31.3568543534868,
32.3544257264697,33.3519970994527,34.3495684724356,35.3471398454185,36.3447112184015,
37.3422825913844,38.3398539643673,39.3374253373503,40.3349967103332,41.3325680833161,
42.3301394562991,43.327710829282,44.3252822022649,45.3228535752479,46.3204249482308,
47.3179963212137,48.3155676941967,49.3131390671796,50.3107104401625,51.3082818131455,
52.3058531861284,53.3034245591113,54.3009959320943,55.2985673050772,56.2961386780601,
57.2937100510431,58.291281424026,59.2888527970089,60.2864241699919,61.2839955429748,
62.2815669159577,63.2791382889407,64.2767096619236,65.2742810349065,66.2718524078895,
67.2694237808724,68.2669951538553,69.2645665268383,70.2621378998212,71.2597092728041,
72.2572806457871,73.25485201877,74.2524233917529,75.2499947647359,76.2475661377188,
77.2451375107017,78.2427088836847,79.2402802566676,80.2378516296505,81.2354230026335,
82.2329943756164,83.2305657485993,84.2281371215823,85.2257084945652,86.2232798675481,
87.2208512405311,88.218422613514,89.2159939864969,90.2135653594799,91.2111367324628,
92.2087081054457,93.2062794784287,94.2038508514116,95.2014222243945,96.1989935973775,
97.1965649703604),.UNSPECIFIED.);
#228=B_SPLINE_SURFACE_WITH_KNOTS('',3,3,((#20294,#20295,#20296,#20297,#20298,
#20299,#20300,#20301,#20302,#20303,#20304,#20305,#20306,#20307,#20308,#20309,
#20310,#20311,#20312,#20313,#20314,#20315,#20316,#20317,#20318,#20319,#20320,
#20321,#20322,#20323,#20324,#20325,#20326,#20327,#20328,#20329,#20330,#20331,
#20332,#20333,#20334,#20335,#20336,#20337,#20338,#20339,#20340,#20341,#20342,
#20343,#20344,#20345,#20346,#20347,#20348,#20349,#20350,#20351,#20352,#20353,
#20354,#20355,#20356,#20357,#20358,#20359,#20360,#20361,#20362,#20363,#20364,
#20365,#20366,#20367,#20368,#20369,#20370,#20371,#20372,#20373,#20374,#20375,
#20376,#20377,#20378,#20379),(#20380,#20381,#20382,#20383,#20384,#20385,
#20386,#20387,#20388,#20389,#20390,#20391,#20392,#20393,#20394,#20395,#20396,
#20397,#20398,#20399,#20400,#20401,#20402,#20403,#20404,#20405,#20406,#20407,
#20408,#20409,#20410,#20411,#20412,#20413,#20414,#20415,#20416,#20417,#20418,
#20419,#20420,#20421,#20422,#20423,#20424,#20425,#20426,#20427,#20428,#20429,
#20430,#20431,#20432,#20433,#20434,#20435,#20436,#20437,#20438,#20439,#20440,
#20441,#20442,#20443,#20444,#20445,#20446,#20447,#20448,#20449,#20450,#20451,
#20452,#20453,#20454,#20455,#20456,#20457,#20458,#20459,#20460,#20461,#20462,
#20463,#20464,#20465),(#20466,#20467,#20468,#20469,#20470,#20471,#20472,
#20473,#20474,#20475,#20476,#20477,#20478,#20479,#20480,#20481,#20482,#20483,
#20484,#20485,#20486,#20487,#20488,#20489,#20490,#20491,#20492,#20493,#20494,
#20495,#20496,#20497,#20498,#20499,#20500,#20501,#20502,#20503,#20504,#20505,
#20506,#20507,#20508,#20509,#20510,#20511,#20512,#20513,#20514,#20515,#20516,
#20517,#20518,#20519,#20520,#20521,#20522,#20523,#20524,#20525,#20526,#20527,
#20528,#20529,#20530,#20531,#20532,#20533,#20534,#20535,#20536,#20537,#20538,
#20539,#20540,#20541,#20542,#20543,#20544,#20545,#20546,#20547,#20548,#20549,
#20550,#20551),(#20552,#20553,#20554,#20555,#20556,#20557,#20558,#20559,
#20560,#20561,#20562,#20563,#20564,#20565,#20566,#20567,#20568,#20569,#20570,
#20571,#20572,#20573,#20574,#20575,#20576,#20577,#20578,#20579,#20580,#20581,
#20582,#20583,#20584,#20585,#20586,#20587,#20588,#20589,#20590,#20591,#20592,
#20593,#20594,#20595,#20596,#20597,#20598,#20599,#20600,#20601,#20602,#20603,
#20604,#20605,#20606,#20607,#20608,#20609,#20610,#20611,#20612,#20613,#20614,
#20615,#20616,#20617,#20618,#20619,#20620,#20621,#20622,#20623,#20624,#20625,
#20626,#20627,#20628,#20629,#20630,#20631,#20632,#20633,#20634,#20635,#20636,
#20637)),.UNSPECIFIED.,.F.,.F.,.F.,(4,4),(4,1,1,1,1,1,1,1,1,1,1,1,1,1,1,
1,1,1,1,1,1,1,1,1,1,1,1,1,1,1,1,1,1,1,1,1,1,1,1,1,1,1,1,1,1,1,1,1,1,1,1,
1,1,1,1,1,1,1,1,1,1,1,1,1,1,1,1,1,1,1,1,1,1,1,1,1,1,1,1,1,1,1,1,4),(0.,
0.0448889834294937),(11.8615800042567,12.8591513772396,13.8567227502225,
14.8542941232055,15.8518654961884,16.8494368691713,17.8470082421543,18.8445796151372,
19.8421509881201,20.8397223611031,21.837293734086,22.8348651070689,23.8324364800519,
24.8300078530348,25.8275792260178,26.8251505990007,27.8227219719836,28.8202933449666,
29.8178647179495,30.8154360909324,31.8130074639154,32.8105788368983,33.8081502098812,
34.8057215828642,35.8032929558471,36.80086432883,37.798435701813,38.7960070747959,
39.7935784477788,40.7911498207618,41.7887211937447,42.7862925667276,43.7838639397106,
44.7814353126935,45.7790066856764,46.7765780586594,47.7741494316423,48.7717208046252,
49.7692921776082,50.7668635505911,51.764434923574,52.762006296557,53.7595776695399,
54.7571490425228,55.7547204155058,56.7522917884887,57.7498631614716,58.7474345344546,
59.7450059074375,60.7425772804204,61.7401486534034,62.7377200263863,63.7352913993692,
64.7328627723522,65.7304341453351,66.728005518318,67.725576891301,68.7231482642839,
69.7207196372668,70.7182910102498,71.7158623832327,72.7134337562156,73.7110051291986,
74.7085765021815,75.7061478751644,76.7037192481474,77.7012906211303,78.6988619941132,
79.6964333670962,80.6940047400791,81.6915761130621,82.689147486045,83.6867188590279,
84.6842902320109,85.6818616049938,86.6794329779767,87.6770043509596,88.6745757239426,
89.6721470969255,90.6697184699085,91.6672898428914,92.6648612158743,93.6624325888573,
94.6600039618402),.UNSPECIFIED.);
#229=B_SPLINE_SURFACE_WITH_KNOTS('',3,3,((#20715,#20716,#20717,#20718,#20719,
#20720,#20721,#20722,#20723,#20724,#20725,#20726,#20727,#20728,#20729,#20730,
#20731,#20732,#20733,#20734,#20735,#20736,#20737,#20738,#20739,#20740,#20741,
#20742,#20743,#20744,#20745,#20746,#20747,#20748,#20749,#20750,#20751,#20752,
#20753,#20754,#20755,#20756,#20757,#20758,#20759,#20760,#20761,#20762,#20763,
#20764,#20765,#20766,#20767,#20768,#20769,#20770,#20771,#20772,#20773,#20774,
#20775,#20776,#20777,#20778,#20779,#20780,#20781,#20782,#20783,#20784,#20785,
#20786,#20787,#20788,#20789,#20790,#20791,#20792,#20793,#20794,#20795,#20796,
#20797,#20798,#20799,#20800),(#20801,#20802,#20803,#20804,#20805,#20806,
#20807,#20808,#20809,#20810,#20811,#20812,#20813,#20814,#20815,#20816,#20817,
#20818,#20819,#20820,#20821,#20822,#20823,#20824,#20825,#20826,#20827,#20828,
#20829,#20830,#20831,#20832,#20833,#20834,#20835,#20836,#20837,#20838,#20839,
#20840,#20841,#20842,#20843,#20844,#20845,#20846,#20847,#20848,#20849,#20850,
#20851,#20852,#20853,#20854,#20855,#20856,#20857,#20858,#20859,#20860,#20861,
#20862,#20863,#20864,#20865,#20866,#20867,#20868,#20869,#20870,#20871,#20872,
#20873,#20874,#20875,#20876,#20877,#20878,#20879,#20880,#20881,#20882,#20883,
#20884,#20885,#20886),(#20887,#20888,#20889,#20890,#20891,#20892,#20893,
#20894,#20895,#20896,#20897,#20898,#20899,#20900,#20901,#20902,#20903,#20904,
#20905,#20906,#20907,#20908,#20909,#20910,#20911,#20912,#20913,#20914,#20915,
#20916,#20917,#20918,#20919,#20920,#20921,#20922,#20923,#20924,#20925,#20926,
#20927,#20928,#20929,#20930,#20931,#20932,#20933,#20934,#20935,#20936,#20937,
#20938,#20939,#20940,#20941,#20942,#20943,#20944,#20945,#20946,#20947,#20948,
#20949,#20950,#20951,#20952,#20953,#20954,#20955,#20956,#20957,#20958,#20959,
#20960,#20961,#20962,#20963,#20964,#20965,#20966,#20967,#20968,#20969,#20970,
#20971,#20972),(#20973,#20974,#20975,#20976,#20977,#20978,#20979,#20980,
#20981,#20982,#20983,#20984,#20985,#20986,#20987,#20988,#20989,#20990,#20991,
#20992,#20993,#20994,#20995,#20996,#20997,#20998,#20999,#21000,#21001,#21002,
#21003,#21004,#21005,#21006,#21007,#21008,#21009,#21010,#21011,#21012,#21013,
#21014,#21015,#21016,#21017,#21018,#21019,#21020,#21021,#21022,#21023,#21024,
#21025,#21026,#21027,#21028,#21029,#21030,#21031,#21032,#21033,#21034,#21035,
#21036,#21037,#21038,#21039,#21040,#21041,#21042,#21043,#21044,#21045,#21046,
#21047,#21048,#21049,#21050,#21051,#21052,#21053,#21054,#21055,#21056,#21057,
#21058)),.UNSPECIFIED.,.F.,.F.,.F.,(4,4),(4,1,1,1,1,1,1,1,1,1,1,1,1,1,1,
1,1,1,1,1,1,1,1,1,1,1,1,1,1,1,1,1,1,1,1,1,1,1,1,1,1,1,1,1,1,1,1,1,1,1,1,
1,1,1,1,1,1,1,1,1,1,1,1,1,1,1,1,1,1,1,1,1,1,1,1,1,1,1,1,1,1,1,1,4),(0.,
0.0448889834294937),(14.3981410127769,15.3957123857599,16.3932837587428,
17.3908551317257,18.3884265047087,19.3859978776916,20.3835692506745,21.3811406236575,
22.3787119966404,23.3762833696233,24.3738547426063,25.3714261155892,26.3689974885721,
27.3665688615551,28.364140234538,29.3617116075209,30.3592829805039,31.3568543534868,
32.3544257264697,33.3519970994527,34.3495684724356,35.3471398454185,36.3447112184015,
37.3422825913844,38.3398539643673,39.3374253373503,40.3349967103332,41.3325680833161,
42.3301394562991,43.327710829282,44.3252822022649,45.3228535752479,46.3204249482308,
47.3179963212137,48.3155676941967,49.3131390671796,50.3107104401625,51.3082818131455,
52.3058531861284,53.3034245591113,54.3009959320943,55.2985673050772,56.2961386780601,
57.2937100510431,58.291281424026,59.2888527970089,60.2864241699919,61.2839955429748,
62.2815669159577,63.2791382889407,64.2767096619236,65.2742810349065,66.2718524078895,
67.2694237808724,68.2669951538553,69.2645665268383,70.2621378998212,71.2597092728041,
72.2572806457871,73.25485201877,74.2524233917529,75.2499947647359,76.2475661377188,
77.2451375107017,78.2427088836847,79.2402802566676,80.2378516296505,81.2354230026335,
82.2329943756164,83.2305657485993,84.2281371215823,85.2257084945652,86.2232798675481,
87.2208512405311,88.218422613514,89.2159939864969,90.2135653594799,91.2111367324628,
92.2087081054457,93.2062794784287,94.2038508514116,95.2014222243945,96.1989935973775,
97.1965649703604),.UNSPECIFIED.);
#230=B_SPLINE_SURFACE_WITH_KNOTS('',3,3,((#21267,#21268,#21269,#21270,#21271,
#21272,#21273,#21274,#21275,#21276,#21277,#21278,#21279,#21280,#21281,#21282,
#21283,#21284,#21285,#21286,#21287,#21288,#21289,#21290,#21291,#21292,#21293,
#21294,#21295,#21296,#21297,#21298,#21299,#21300,#21301,#21302,#21303,#21304,
#21305,#21306,#21307,#21308,#21309,#21310,#21311,#21312,#21313,#21314,#21315,
#21316,#21317,#21318,#21319,#21320,#21321,#21322,#21323,#21324,#21325,#21326,
#21327,#21328,#21329,#21330,#21331,#21332,#21333,#21334,#21335,#21336,#21337,
#21338,#21339,#21340,#21341,#21342,#21343,#21344,#21345,#21346,#21347,#21348,
#21349,#21350,#21351,#21352),(#21353,#21354,#21355,#21356,#21357,#21358,
#21359,#21360,#21361,#21362,#21363,#21364,#21365,#21366,#21367,#21368,#21369,
#21370,#21371,#21372,#21373,#21374,#21375,#21376,#21377,#21378,#21379,#21380,
#21381,#21382,#21383,#21384,#21385,#21386,#21387,#21388,#21389,#21390,#21391,
#21392,#21393,#21394,#21395,#21396,#21397,#21398,#21399,#21400,#21401,#21402,
#21403,#21404,#21405,#21406,#21407,#21408,#21409,#21410,#21411,#21412,#21413,
#21414,#21415,#21416,#21417,#21418,#21419,#21420,#21421,#21422,#21423,#21424,
#21425,#21426,#21427,#21428,#21429,#21430,#21431,#21432,#21433,#21434,#21435,
#21436,#21437,#21438),(#21439,#21440,#21441,#21442,#21443,#21444,#21445,
#21446,#21447,#21448,#21449,#21450,#21451,#21452,#21453,#21454,#21455,#21456,
#21457,#21458,#21459,#21460,#21461,#21462,#21463,#21464,#21465,#21466,#21467,
#21468,#21469,#21470,#21471,#21472,#21473,#21474,#21475,#21476,#21477,#21478,
#21479,#21480,#21481,#21482,#21483,#21484,#21485,#21486,#21487,#21488,#21489,
#21490,#21491,#21492,#21493,#21494,#21495,#21496,#21497,#21498,#21499,#21500,
#21501,#21502,#21503,#21504,#21505,#21506,#21507,#21508,#21509,#21510,#21511,
#21512,#21513,#21514,#21515,#21516,#21517,#21518,#21519,#21520,#21521,#21522,
#21523,#21524),(#21525,#21526,#21527,#21528,#21529,#21530,#21531,#21532,
#21533,#21534,#21535,#21536,#21537,#21538,#21539,#21540,#21541,#21542,#21543,
#21544,#21545,#21546,#21547,#21548,#21549,#21550,#21551,#21552,#21553,#21554,
#21555,#21556,#21557,#21558,#21559,#21560,#21561,#21562,#21563,#21564,#21565,
#21566,#21567,#21568,#21569,#21570,#21571,#21572,#21573,#21574,#21575,#21576,
#21577,#21578,#21579,#21580,#21581,#21582,#21583,#21584,#21585,#21586,#21587,
#21588,#21589,#21590,#21591,#21592,#21593,#21594,#21595,#21596,#21597,#21598,
#21599,#21600,#21601,#21602,#21603,#21604,#21605,#21606,#21607,#21608,#21609,
#21610)),.UNSPECIFIED.,.F.,.F.,.F.,(4,4),(4,1,1,1,1,1,1,1,1,1,1,1,1,1,1,
1,1,1,1,1,1,1,1,1,1,1,1,1,1,1,1,1,1,1,1,1,1,1,1,1,1,1,1,1,1,1,1,1,1,1,1,
1,1,1,1,1,1,1,1,1,1,1,1,1,1,1,1,1,1,1,1,1,1,1,1,1,1,1,1,1,1,1,1,4),(0.,
0.0448889834294937),(11.8615800042567,12.8591513772396,13.8567227502226,
14.8542941232055,15.8518654961884,16.8494368691714,17.8470082421543,18.8445796151372,
19.8421509881202,20.8397223611031,21.837293734086,22.834865107069,23.8324364800519,
24.8300078530348,25.8275792260178,26.8251505990007,27.8227219719836,28.8202933449666,
29.8178647179495,30.8154360909324,31.8130074639154,32.8105788368983,33.8081502098812,
34.8057215828642,35.8032929558471,36.80086432883,37.798435701813,38.7960070747959,
39.7935784477789,40.7911498207618,41.7887211937447,42.7862925667277,43.7838639397106,
44.7814353126935,45.7790066856765,46.7765780586594,47.7741494316423,48.7717208046253,
49.7692921776082,50.7668635505911,51.7644349235741,52.762006296557,53.7595776695399,
54.7571490425229,55.7547204155058,56.7522917884887,57.7498631614717,58.7474345344546,
59.7450059074375,60.7425772804205,61.7401486534034,62.7377200263864,63.7352913993693,
64.7328627723522,65.7304341453352,66.7280055183181,67.725576891301,68.723148264284,
69.7207196372669,70.7182910102498,71.7158623832328,72.7134337562157,73.7110051291986,
74.7085765021816,75.7061478751645,76.7037192481474,77.7012906211304,78.6988619941133,
79.6964333670962,80.6940047400792,81.6915761130621,82.689147486045,83.686718859028,
84.6842902320109,85.6818616049939,86.6794329779768,87.6770043509597,88.6745757239427,
89.6721470969256,90.6697184699085,91.6672898428915,92.6648612158744,93.6624325888573,
94.6600039618403),.UNSPECIFIED.);
#231=B_SPLINE_SURFACE_WITH_KNOTS('',3,3,((#21688,#21689,#21690,#21691,#21692,
#21693,#21694,#21695,#21696,#21697,#21698,#21699,#21700,#21701,#21702,#21703,
#21704,#21705,#21706,#21707,#21708,#21709,#21710,#21711,#21712,#21713,#21714,
#21715,#21716,#21717,#21718,#21719,#21720,#21721,#21722,#21723,#21724,#21725,
#21726,#21727,#21728,#21729,#21730,#21731,#21732,#21733,#21734,#21735,#21736,
#21737,#21738,#21739,#21740,#21741,#21742,#21743,#21744,#21745,#21746,#21747,
#21748,#21749,#21750,#21751,#21752,#21753,#21754,#21755,#21756,#21757,#21758,
#21759,#21760,#21761,#21762,#21763,#21764,#21765,#21766,#21767,#21768,#21769,
#21770,#21771,#21772,#21773),(#21774,#21775,#21776,#21777,#21778,#21779,
#21780,#21781,#21782,#21783,#21784,#21785,#21786,#21787,#21788,#21789,#21790,
#21791,#21792,#21793,#21794,#21795,#21796,#21797,#21798,#21799,#21800,#21801,
#21802,#21803,#21804,#21805,#21806,#21807,#21808,#21809,#21810,#21811,#21812,
#21813,#21814,#21815,#21816,#21817,#21818,#21819,#21820,#21821,#21822,#21823,
#21824,#21825,#21826,#21827,#21828,#21829,#21830,#21831,#21832,#21833,#21834,
#21835,#21836,#21837,#21838,#21839,#21840,#21841,#21842,#21843,#21844,#21845,
#21846,#21847,#21848,#21849,#21850,#21851,#21852,#21853,#21854,#21855,#21856,
#21857,#21858,#21859),(#21860,#21861,#21862,#21863,#21864,#21865,#21866,
#21867,#21868,#21869,#21870,#21871,#21872,#21873,#21874,#21875,#21876,#21877,
#21878,#21879,#21880,#21881,#21882,#21883,#21884,#21885,#21886,#21887,#21888,
#21889,#21890,#21891,#21892,#21893,#21894,#21895,#21896,#21897,#21898,#21899,
#21900,#21901,#21902,#21903,#21904,#21905,#21906,#21907,#21908,#21909,#21910,
#21911,#21912,#21913,#21914,#21915,#21916,#21917,#21918,#21919,#21920,#21921,
#21922,#21923,#21924,#21925,#21926,#21927,#21928,#21929,#21930,#21931,#21932,
#21933,#21934,#21935,#21936,#21937,#21938,#21939,#21940,#21941,#21942,#21943,
#21944,#21945),(#21946,#21947,#21948,#21949,#21950,#21951,#21952,#21953,
#21954,#21955,#21956,#21957,#21958,#21959,#21960,#21961,#21962,#21963,#21964,
#21965,#21966,#21967,#21968,#21969,#21970,#21971,#21972,#21973,#21974,#21975,
#21976,#21977,#21978,#21979,#21980,#21981,#21982,#21983,#21984,#21985,#21986,
#21987,#21988,#21989,#21990,#21991,#21992,#21993,#21994,#21995,#21996,#21997,
#21998,#21999,#22000,#22001,#22002,#22003,#22004,#22005,#22006,#22007,#22008,
#22009,#22010,#22011,#22012,#22013,#22014,#22015,#22016,#22017,#22018,#22019,
#22020,#22021,#22022,#22023,#22024,#22025,#22026,#22027,#22028,#22029,#22030,
#22031)),.UNSPECIFIED.,.F.,.F.,.F.,(4,4),(4,1,1,1,1,1,1,1,1,1,1,1,1,1,1,
1,1,1,1,1,1,1,1,1,1,1,1,1,1,1,1,1,1,1,1,1,1,1,1,1,1,1,1,1,1,1,1,1,1,1,1,
1,1,1,1,1,1,1,1,1,1,1,1,1,1,1,1,1,1,1,1,1,1,1,1,1,1,1,1,1,1,1,1,4),(0.,
0.0448889834294937),(14.3981410127769,15.3957123857599,16.3932837587428,
17.3908551317257,18.3884265047087,19.3859978776916,20.3835692506745,21.3811406236575,
22.3787119966404,23.3762833696233,24.3738547426063,25.3714261155892,26.3689974885721,
27.3665688615551,28.364140234538,29.3617116075209,30.3592829805039,31.3568543534868,
32.3544257264697,33.3519970994527,34.3495684724356,35.3471398454185,36.3447112184015,
37.3422825913844,38.3398539643674,39.3374253373503,40.3349967103332,41.3325680833162,
42.3301394562991,43.327710829282,44.325282202265,45.3228535752479,46.3204249482308,
47.3179963212138,48.3155676941967,49.3131390671796,50.3107104401626,51.3082818131455,
52.3058531861284,53.3034245591114,54.3009959320943,55.2985673050772,56.2961386780602,
57.2937100510431,58.291281424026,59.288852797009,60.2864241699919,61.2839955429748,
62.2815669159578,63.2791382889407,64.2767096619237,65.2742810349066,66.2718524078895,
67.2694237808725,68.2669951538554,69.2645665268383,70.2621378998213,71.2597092728042,
72.2572806457871,73.2548520187701,74.252423391753,75.2499947647359,76.2475661377189,
77.2451375107018,78.2427088836847,79.2402802566677,80.2378516296506,81.2354230026336,
82.2329943756165,83.2305657485994,84.2281371215823,85.2257084945653,86.2232798675482,
87.2208512405312,88.2184226135141,89.215993986497,90.21356535948,91.2111367324629,
92.2087081054458,93.2062794784288,94.2038508514117,95.2014222243946,96.1989935973776,
97.1965649703605),.UNSPECIFIED.);
#232=B_SPLINE_SURFACE_WITH_KNOTS('',3,3,((#23003,#23004,#23005,#23006,#23007,
#23008,#23009,#23010,#23011,#23012,#23013,#23014,#23015,#23016,#23017,#23018,
#23019,#23020,#23021,#23022,#23023,#23024,#23025,#23026,#23027,#23028,#23029,
#23030,#23031,#23032,#23033,#23034,#23035,#23036,#23037,#23038,#23039,#23040,
#23041,#23042,#23043,#23044,#23045,#23046,#23047,#23048,#23049,#23050,#23051),
(#23052,#23053,#23054,#23055,#23056,#23057,#23058,#23059,#23060,#23061,
#23062,#23063,#23064,#23065,#23066,#23067,#23068,#23069,#23070,#23071,#23072,
#23073,#23074,#23075,#23076,#23077,#23078,#23079,#23080,#23081,#23082,#23083,
#23084,#23085,#23086,#23087,#23088,#23089,#23090,#23091,#23092,#23093,#23094,
#23095,#23096,#23097,#23098,#23099,#23100),(#23101,#23102,#23103,#23104,
#23105,#23106,#23107,#23108,#23109,#23110,#23111,#23112,#23113,#23114,#23115,
#23116,#23117,#23118,#23119,#23120,#23121,#23122,#23123,#23124,#23125,#23126,
#23127,#23128,#23129,#23130,#23131,#23132,#23133,#23134,#23135,#23136,#23137,
#23138,#23139,#23140,#23141,#23142,#23143,#23144,#23145,#23146,#23147,#23148,
#23149),(#23150,#23151,#23152,#23153,#23154,#23155,#23156,#23157,#23158,
#23159,#23160,#23161,#23162,#23163,#23164,#23165,#23166,#23167,#23168,#23169,
#23170,#23171,#23172,#23173,#23174,#23175,#23176,#23177,#23178,#23179,#23180,
#23181,#23182,#23183,#23184,#23185,#23186,#23187,#23188,#23189,#23190,#23191,
#23192,#23193,#23194,#23195,#23196,#23197,#23198)),.UNSPECIFIED.,.F.,.F.,
 .F.,(4,4),(4,1,1,1,1,1,1,1,1,1,1,1,1,1,1,1,1,1,1,1,1,1,1,1,1,1,1,1,1,1,
1,1,1,1,1,1,1,1,1,1,1,1,1,1,1,1,4),(0.,0.0965329650085055),(11.852942864427,
12.3521979234545,12.851452982482,13.3507080415095,13.849963100537,14.3492181595645,
14.848473218592,15.3477282776195,15.846983336647,16.3462383956745,16.845493454702,
17.3447485137295,17.844003572757,18.3432586317845,18.842513690812,19.3417687498395,
19.841023808867,20.3402788678945,20.839533926922,21.3387889859495,21.838044044977,
22.3372991040045,22.836554163032,23.3358092220595,23.835064281087,24.3343193401145,
24.833574399142,25.3328294581695,25.832084517197,26.3313395762245,26.830594635252,
27.3298496942795,27.829104753307,28.3283598123345,28.827614871362,29.3268699303895,
29.826124989417,30.3253800484445,30.824635107472,31.3238901664995,31.823145225527,
32.3224002845545,32.821655343582,33.3209104026095,33.820165461637,34.3194205206645,
34.818675579692),.UNSPECIFIED.);
#233=B_SPLINE_SURFACE_WITH_KNOTS('',3,3,((#23385,#23386,#23387,#23388,#23389,
#23390,#23391,#23392,#23393,#23394,#23395,#23396,#23397,#23398,#23399,#23400,
#23401,#23402,#23403,#23404,#23405,#23406,#23407,#23408,#23409,#23410,#23411,
#23412,#23413,#23414,#23415,#23416,#23417,#23418,#23419,#23420,#23421,#23422,
#23423,#23424,#23425,#23426,#23427,#23428,#23429,#23430,#23431,#23432,#23433),
(#23434,#23435,#23436,#23437,#23438,#23439,#23440,#23441,#23442,#23443,
#23444,#23445,#23446,#23447,#23448,#23449,#23450,#23451,#23452,#23453,#23454,
#23455,#23456,#23457,#23458,#23459,#23460,#23461,#23462,#23463,#23464,#23465,
#23466,#23467,#23468,#23469,#23470,#23471,#23472,#23473,#23474,#23475,#23476,
#23477,#23478,#23479,#23480,#23481,#23482),(#23483,#23484,#23485,#23486,
#23487,#23488,#23489,#23490,#23491,#23492,#23493,#23494,#23495,#23496,#23497,
#23498,#23499,#23500,#23501,#23502,#23503,#23504,#23505,#23506,#23507,#23508,
#23509,#23510,#23511,#23512,#23513,#23514,#23515,#23516,#23517,#23518,#23519,
#23520,#23521,#23522,#23523,#23524,#23525,#23526,#23527,#23528,#23529,#23530,
#23531),(#23532,#23533,#23534,#23535,#23536,#23537,#23538,#23539,#23540,
#23541,#23542,#23543,#23544,#23545,#23546,#23547,#23548,#23549,#23550,#23551,
#23552,#23553,#23554,#23555,#23556,#23557,#23558,#23559,#23560,#23561,#23562,
#23563,#23564,#23565,#23566,#23567,#23568,#23569,#23570,#23571,#23572,#23573,
#23574,#23575,#23576,#23577,#23578,#23579,#23580)),.UNSPECIFIED.,.F.,.F.,
 .F.,(4,4),(4,1,1,1,1,1,1,1,1,1,1,1,1,1,1,1,1,1,1,1,1,1,1,1,1,1,1,1,1,1,
1,1,1,1,1,1,1,1,1,1,1,1,1,1,1,1,4),(0.,0.0965329650085055),(14.399609326548,
14.8988643855755,15.398119444603,15.8973745036305,16.396629562658,16.8958846216855,
17.395139680713,17.8943947397405,18.393649798768,18.8929048577955,19.392159916823,
19.8914149758505,20.390670034878,20.8899250939055,21.389180152933,21.8884352119605,
22.387690270988,22.8869453300155,23.386200389043,23.8854554480705,24.384710507098,
24.8839655661255,25.383220625153,25.8824756841805,26.381730743208,26.8809858022355,
27.380240861263,27.8794959202905,28.378750979318,28.8780060383455,29.377261097373,
29.8765161564005,30.375771215428,30.8750262744555,31.374281333483,31.8735363925105,
32.372791451538,32.8720465105655,33.371301569593,33.8705566286205,34.369811687648,
34.8690667466755,35.368321805703,35.8675768647305,36.366831923758,36.8660869827855,
37.365342041813),.UNSPECIFIED.);
#234=B_SPLINE_SURFACE_WITH_KNOTS('',3,3,((#23796,#23797,#23798,#23799,#23800,
#23801,#23802,#23803,#23804,#23805,#23806,#23807,#23808,#23809,#23810,#23811,
#23812,#23813,#23814,#23815,#23816,#23817,#23818,#23819,#23820,#23821,#23822,
#23823,#23824,#23825,#23826,#23827,#23828,#23829,#23830,#23831,#23832,#23833,
#23834,#23835,#23836,#23837,#23838,#23839,#23840,#23841,#23842,#23843,#23844),
(#23845,#23846,#23847,#23848,#23849,#23850,#23851,#23852,#23853,#23854,
#23855,#23856,#23857,#23858,#23859,#23860,#23861,#23862,#23863,#23864,#23865,
#23866,#23867,#23868,#23869,#23870,#23871,#23872,#23873,#23874,#23875,#23876,
#23877,#23878,#23879,#23880,#23881,#23882,#23883,#23884,#23885,#23886,#23887,
#23888,#23889,#23890,#23891,#23892,#23893),(#23894,#23895,#23896,#23897,
#23898,#23899,#23900,#23901,#23902,#23903,#23904,#23905,#23906,#23907,#23908,
#23909,#23910,#23911,#23912,#23913,#23914,#23915,#23916,#23917,#23918,#23919,
#23920,#23921,#23922,#23923,#23924,#23925,#23926,#23927,#23928,#23929,#23930,
#23931,#23932,#23933,#23934,#23935,#23936,#23937,#23938,#23939,#23940,#23941,
#23942),(#23943,#23944,#23945,#23946,#23947,#23948,#23949,#23950,#23951,
#23952,#23953,#23954,#23955,#23956,#23957,#23958,#23959,#23960,#23961,#23962,
#23963,#23964,#23965,#23966,#23967,#23968,#23969,#23970,#23971,#23972,#23973,
#23974,#23975,#23976,#23977,#23978,#23979,#23980,#23981,#23982,#23983,#23984,
#23985,#23986,#23987,#23988,#23989,#23990,#23991)),.UNSPECIFIED.,.F.,.F.,
 .F.,(4,4),(4,1,1,1,1,1,1,1,1,1,1,1,1,1,1,1,1,1,1,1,1,1,1,1,1,1,1,1,1,1,
1,1,1,1,1,1,1,1,1,1,1,1,1,1,1,1,4),(0.,0.0965329650085055),(11.852942864427,
12.3521979234545,12.851452982482,13.3507080415095,13.849963100537,14.3492181595645,
14.848473218592,15.3477282776195,15.846983336647,16.3462383956745,16.845493454702,
17.3447485137295,17.844003572757,18.3432586317845,18.842513690812,19.3417687498395,
19.841023808867,20.3402788678945,20.839533926922,21.3387889859495,21.838044044977,
22.3372991040045,22.836554163032,23.3358092220595,23.835064281087,24.3343193401145,
24.833574399142,25.3328294581695,25.832084517197,26.3313395762245,26.830594635252,
27.3298496942795,27.829104753307,28.3283598123345,28.827614871362,29.3268699303895,
29.826124989417,30.3253800484445,30.824635107472,31.3238901664995,31.823145225527,
32.3224002845545,32.821655343582,33.3209104026095,33.820165461637,34.3194205206645,
34.818675579692),.UNSPECIFIED.);
#235=B_SPLINE_SURFACE_WITH_KNOTS('',3,3,((#24178,#24179,#24180,#24181,#24182,
#24183,#24184,#24185,#24186,#24187,#24188,#24189,#24190,#24191,#24192,#24193,
#24194,#24195,#24196,#24197,#24198,#24199,#24200,#24201,#24202,#24203,#24204,
#24205,#24206,#24207,#24208,#24209,#24210,#24211,#24212,#24213,#24214,#24215,
#24216,#24217,#24218,#24219,#24220,#24221,#24222,#24223,#24224,#24225,#24226),
(#24227,#24228,#24229,#24230,#24231,#24232,#24233,#24234,#24235,#24236,
#24237,#24238,#24239,#24240,#24241,#24242,#24243,#24244,#24245,#24246,#24247,
#24248,#24249,#24250,#24251,#24252,#24253,#24254,#24255,#24256,#24257,#24258,
#24259,#24260,#24261,#24262,#24263,#24264,#24265,#24266,#24267,#24268,#24269,
#24270,#24271,#24272,#24273,#24274,#24275),(#24276,#24277,#24278,#24279,
#24280,#24281,#24282,#24283,#24284,#24285,#24286,#24287,#24288,#24289,#24290,
#24291,#24292,#24293,#24294,#24295,#24296,#24297,#24298,#24299,#24300,#24301,
#24302,#24303,#24304,#24305,#24306,#24307,#24308,#24309,#24310,#24311,#24312,
#24313,#24314,#24315,#24316,#24317,#24318,#24319,#24320,#24321,#24322,#24323,
#24324),(#24325,#24326,#24327,#24328,#24329,#24330,#24331,#24332,#24333,
#24334,#24335,#24336,#24337,#24338,#24339,#24340,#24341,#24342,#24343,#24344,
#24345,#24346,#24347,#24348,#24349,#24350,#24351,#24352,#24353,#24354,#24355,
#24356,#24357,#24358,#24359,#24360,#24361,#24362,#24363,#24364,#24365,#24366,
#24367,#24368,#24369,#24370,#24371,#24372,#24373)),.UNSPECIFIED.,.F.,.F.,
 .F.,(4,4),(4,1,1,1,1,1,1,1,1,1,1,1,1,1,1,1,1,1,1,1,1,1,1,1,1,1,1,1,1,1,
1,1,1,1,1,1,1,1,1,1,1,1,1,1,1,1,4),(0.,0.0965329650085055),(14.399609326548,
14.8988643855755,15.398119444603,15.8973745036305,16.396629562658,16.8958846216855,
17.395139680713,17.8943947397405,18.393649798768,18.8929048577955,19.392159916823,
19.8914149758505,20.390670034878,20.8899250939055,21.389180152933,21.8884352119605,
22.387690270988,22.8869453300155,23.386200389043,23.8854554480705,24.384710507098,
24.8839655661255,25.383220625153,25.8824756841805,26.381730743208,26.8809858022355,
27.380240861263,27.8794959202905,28.378750979318,28.8780060383455,29.377261097373,
29.8765161564005,30.375771215428,30.8750262744555,31.374281333483,31.8735363925105,
32.372791451538,32.8720465105655,33.371301569593,33.8705566286205,34.369811687648,
34.8690667466755,35.368321805703,35.8675768647305,36.366831923758,36.8660869827855,
37.365342041813),.UNSPECIFIED.);
#236=B_SPLINE_SURFACE_WITH_KNOTS('',3,3,((#26841,#26842,#26843,#26844,#26845,
#26846,#26847,#26848,#26849,#26850,#26851,#26852,#26853,#26854,#26855,#26856,
#26857,#26858,#26859,#26860,#26861,#26862,#26863,#26864,#26865,#26866,#26867,
#26868,#26869,#26870,#26871,#26872,#26873,#26874,#26875,#26876,#26877,#26878,
#26879,#26880,#26881,#26882,#26883,#26884,#26885,#26886,#26887,#26888,#26889,
#26890,#26891,#26892,#26893,#26894,#26895,#26896),(#26897,#26898,#26899,
#26900,#26901,#26902,#26903,#26904,#26905,#26906,#26907,#26908,#26909,#26910,
#26911,#26912,#26913,#26914,#26915,#26916,#26917,#26918,#26919,#26920,#26921,
#26922,#26923,#26924,#26925,#26926,#26927,#26928,#26929,#26930,#26931,#26932,
#26933,#26934,#26935,#26936,#26937,#26938,#26939,#26940,#26941,#26942,#26943,
#26944,#26945,#26946,#26947,#26948,#26949,#26950,#26951,#26952),(#26953,
#26954,#26955,#26956,#26957,#26958,#26959,#26960,#26961,#26962,#26963,#26964,
#26965,#26966,#26967,#26968,#26969,#26970,#26971,#26972,#26973,#26974,#26975,
#26976,#26977,#26978,#26979,#26980,#26981,#26982,#26983,#26984,#26985,#26986,
#26987,#26988,#26989,#26990,#26991,#26992,#26993,#26994,#26995,#26996,#26997,
#26998,#26999,#27000,#27001,#27002,#27003,#27004,#27005,#27006,#27007,#27008),
(#27009,#27010,#27011,#27012,#27013,#27014,#27015,#27016,#27017,#27018,
#27019,#27020,#27021,#27022,#27023,#27024,#27025,#27026,#27027,#27028,#27029,
#27030,#27031,#27032,#27033,#27034,#27035,#27036,#27037,#27038,#27039,#27040,
#27041,#27042,#27043,#27044,#27045,#27046,#27047,#27048,#27049,#27050,#27051,
#27052,#27053,#27054,#27055,#27056,#27057,#27058,#27059,#27060,#27061,#27062,
#27063,#27064)),.UNSPECIFIED.,.F.,.F.,.F.,(4,4),(4,1,1,1,1,1,1,1,1,1,1,
1,1,1,1,1,1,1,1,1,1,1,1,1,1,1,1,1,1,1,1,1,1,1,1,1,1,1,1,1,1,1,1,1,1,1,1,
1,1,1,1,1,1,4),(0.,0.0321584099938621),(11.8553612635793,12.8418906022433,
13.8284199409074,14.8149492795714,15.8014786182354,16.7880079568995,17.7745372955635,
18.7610666342275,19.7475959728915,20.7341253115556,21.7206546502196,22.7071839888836,
23.6937133275477,24.6802426662117,25.6667720048757,26.6533013435398,27.6398306822038,
28.6263600208678,29.6128893595319,30.5994186981959,31.5859480368599,32.5724773755239,
33.559006714188,34.545536052852,35.532065391516,36.5185947301801,37.5051240688441,
38.4916534075081,39.4781827461722,40.4647120848362,41.4512414235002,42.4377707621643,
43.4243001008283,44.4108294394923,45.3973587781563,46.3838881168204,47.3704174554844,
48.3569467941484,49.3434761328125,50.3300054714765,51.3165348101405,52.3030641488046,
53.2895934874686,54.2761228261326,55.2626521647967,56.2491815034607,57.2357108421247,
58.2222401807888,59.2087695194528,60.1952988581168,61.1818281967808,62.1683575354449,
63.1548868741089,64.1414162127729),.UNSPECIFIED.);
#237=B_SPLINE_SURFACE_WITH_KNOTS('',3,3,((#27191,#27192,#27193,#27194,#27195,
#27196,#27197,#27198,#27199,#27200,#27201,#27202,#27203,#27204,#27205,#27206,
#27207,#27208,#27209,#27210,#27211,#27212,#27213,#27214,#27215,#27216,#27217,
#27218,#27219,#27220,#27221,#27222,#27223,#27224,#27225,#27226,#27227,#27228,
#27229,#27230,#27231,#27232,#27233,#27234,#27235,#27236,#27237,#27238,#27239,
#27240,#27241,#27242,#27243,#27244,#27245,#27246),(#27247,#27248,#27249,
#27250,#27251,#27252,#27253,#27254,#27255,#27256,#27257,#27258,#27259,#27260,
#27261,#27262,#27263,#27264,#27265,#27266,#27267,#27268,#27269,#27270,#27271,
#27272,#27273,#27274,#27275,#27276,#27277,#27278,#27279,#27280,#27281,#27282,
#27283,#27284,#27285,#27286,#27287,#27288,#27289,#27290,#27291,#27292,#27293,
#27294,#27295,#27296,#27297,#27298,#27299,#27300,#27301,#27302),(#27303,
#27304,#27305,#27306,#27307,#27308,#27309,#27310,#27311,#27312,#27313,#27314,
#27315,#27316,#27317,#27318,#27319,#27320,#27321,#27322,#27323,#27324,#27325,
#27326,#27327,#27328,#27329,#27330,#27331,#27332,#27333,#27334,#27335,#27336,
#27337,#27338,#27339,#27340,#27341,#27342,#27343,#27344,#27345,#27346,#27347,
#27348,#27349,#27350,#27351,#27352,#27353,#27354,#27355,#27356,#27357,#27358),
(#27359,#27360,#27361,#27362,#27363,#27364,#27365,#27366,#27367,#27368,
#27369,#27370,#27371,#27372,#27373,#27374,#27375,#27376,#27377,#27378,#27379,
#27380,#27381,#27382,#27383,#27384,#27385,#27386,#27387,#27388,#27389,#27390,
#27391,#27392,#27393,#27394,#27395,#27396,#27397,#27398,#27399,#27400,#27401,
#27402,#27403,#27404,#27405,#27406,#27407,#27408,#27409,#27410,#27411,#27412,
#27413,#27414)),.UNSPECIFIED.,.F.,.F.,.F.,(4,4),(4,1,1,1,1,1,1,1,1,1,1,
1,1,1,1,1,1,1,1,1,1,1,1,1,1,1,1,1,1,1,1,1,1,1,1,1,1,1,1,1,1,1,1,1,1,1,1,
1,1,1,1,1,1,4),(0.,0.0321584099938621),(14.3984001269718,15.3849294656359,
16.3714588042999,17.3579881429639,18.344517481628,19.331046820292,20.317576158956,
21.30410549762,22.2906348362841,23.2771641749481,24.2636935136121,25.2502228522762,
26.2367521909402,27.2232815296042,28.2098108682683,29.1963402069323,30.1828695455963,
31.1693988842604,32.1559282229244,33.1424575615884,34.1289869002524,35.1155162389165,
36.1020455775805,37.0885749162445,38.0751042549086,39.0616335935726,40.0481629322366,
41.0346922709007,42.0212216095647,43.0077509482287,43.9942802868928,44.9808096255568,
45.9673389642208,46.9538683028848,47.9403976415489,48.9269269802129,49.9134563188769,
50.899985657541,51.886514996205,52.873044334869,53.8595736735331,54.8461030121971,
55.8326323508611,56.8191616895251,57.8056910281892,58.7922203668532,59.7787497055172,
60.7652790441813,61.7518083828453,62.7383377215093,63.7248670601734,64.7113963988374,
65.6979257375014,66.6844550761655),.UNSPECIFIED.);
#238=B_SPLINE_SURFACE_WITH_KNOTS('',3,3,((#27677,#27678,#27679,#27680,#27681,
#27682,#27683,#27684,#27685,#27686,#27687,#27688,#27689,#27690,#27691,#27692,
#27693,#27694,#27695,#27696,#27697,#27698,#27699,#27700,#27701,#27702,#27703,
#27704,#27705,#27706,#27707,#27708,#27709,#27710,#27711,#27712,#27713,#27714,
#27715,#27716,#27717,#27718,#27719,#27720,#27721,#27722,#27723,#27724,#27725,
#27726,#27727,#27728,#27729,#27730,#27731,#27732),(#27733,#27734,#27735,
#27736,#27737,#27738,#27739,#27740,#27741,#27742,#27743,#27744,#27745,#27746,
#27747,#27748,#27749,#27750,#27751,#27752,#27753,#27754,#27755,#27756,#27757,
#27758,#27759,#27760,#27761,#27762,#27763,#27764,#27765,#27766,#27767,#27768,
#27769,#27770,#27771,#27772,#27773,#27774,#27775,#27776,#27777,#27778,#27779,
#27780,#27781,#27782,#27783,#27784,#27785,#27786,#27787,#27788),(#27789,
#27790,#27791,#27792,#27793,#27794,#27795,#27796,#27797,#27798,#27799,#27800,
#27801,#27802,#27803,#27804,#27805,#27806,#27807,#27808,#27809,#27810,#27811,
#27812,#27813,#27814,#27815,#27816,#27817,#27818,#27819,#27820,#27821,#27822,
#27823,#27824,#27825,#27826,#27827,#27828,#27829,#27830,#27831,#27832,#27833,
#27834,#27835,#27836,#27837,#27838,#27839,#27840,#27841,#27842,#27843,#27844),
(#27845,#27846,#27847,#27848,#27849,#27850,#27851,#27852,#27853,#27854,
#27855,#27856,#27857,#27858,#27859,#27860,#27861,#27862,#27863,#27864,#27865,
#27866,#27867,#27868,#27869,#27870,#27871,#27872,#27873,#27874,#27875,#27876,
#27877,#27878,#27879,#27880,#27881,#27882,#27883,#27884,#27885,#27886,#27887,
#27888,#27889,#27890,#27891,#27892,#27893,#27894,#27895,#27896,#27897,#27898,
#27899,#27900)),.UNSPECIFIED.,.F.,.F.,.F.,(4,4),(4,1,1,1,1,1,1,1,1,1,1,
1,1,1,1,1,1,1,1,1,1,1,1,1,1,1,1,1,1,1,1,1,1,1,1,1,1,1,1,1,1,1,1,1,1,1,1,
1,1,1,1,1,1,4),(0.,0.0321584099938621),(11.8553612635793,12.8418906022433,
13.8284199409074,14.8149492795714,15.8014786182354,16.7880079568995,17.7745372955635,
18.7610666342275,19.7475959728915,20.7341253115556,21.7206546502196,22.7071839888836,
23.6937133275477,24.6802426662117,25.6667720048757,26.6533013435398,27.6398306822038,
28.6263600208678,29.6128893595319,30.5994186981959,31.5859480368599,32.5724773755239,
33.559006714188,34.545536052852,35.532065391516,36.5185947301801,37.5051240688441,
38.4916534075081,39.4781827461722,40.4647120848362,41.4512414235002,42.4377707621643,
43.4243001008283,44.4108294394923,45.3973587781563,46.3838881168204,47.3704174554844,
48.3569467941484,49.3434761328125,50.3300054714765,51.3165348101405,52.3030641488046,
53.2895934874686,54.2761228261326,55.2626521647967,56.2491815034607,57.2357108421247,
58.2222401807888,59.2087695194528,60.1952988581168,61.1818281967808,62.1683575354449,
63.1548868741089,64.1414162127729),.UNSPECIFIED.);
#239=B_SPLINE_SURFACE_WITH_KNOTS('',3,3,((#27975,#27976,#27977,#27978,#27979,
#27980,#27981,#27982,#27983,#27984,#27985,#27986,#27987,#27988,#27989,#27990,
#27991,#27992,#27993,#27994,#27995,#27996,#27997,#27998,#27999,#28000,#28001,
#28002,#28003,#28004,#28005,#28006,#28007,#28008,#28009,#28010,#28011,#28012,
#28013,#28014,#28015,#28016,#28017,#28018,#28019,#28020,#28021,#28022,#28023,
#28024,#28025,#28026,#28027,#28028,#28029,#28030),(#28031,#28032,#28033,
#28034,#28035,#28036,#28037,#28038,#28039,#28040,#28041,#28042,#28043,#28044,
#28045,#28046,#28047,#28048,#28049,#28050,#28051,#28052,#28053,#28054,#28055,
#28056,#28057,#28058,#28059,#28060,#28061,#28062,#28063,#28064,#28065,#28066,
#28067,#28068,#28069,#28070,#28071,#28072,#28073,#28074,#28075,#28076,#28077,
#28078,#28079,#28080,#28081,#28082,#28083,#28084,#28085,#28086),(#28087,
#28088,#28089,#28090,#28091,#28092,#28093,#28094,#28095,#28096,#28097,#28098,
#28099,#28100,#28101,#28102,#28103,#28104,#28105,#28106,#28107,#28108,#28109,
#28110,#28111,#28112,#28113,#28114,#28115,#28116,#28117,#28118,#28119,#28120,
#28121,#28122,#28123,#28124,#28125,#28126,#28127,#28128,#28129,#28130,#28131,
#28132,#28133,#28134,#28135,#28136,#28137,#28138,#28139,#28140,#28141,#28142),
(#28143,#28144,#28145,#28146,#28147,#28148,#28149,#28150,#28151,#28152,
#28153,#28154,#28155,#28156,#28157,#28158,#28159,#28160,#28161,#28162,#28163,
#28164,#28165,#28166,#28167,#28168,#28169,#28170,#28171,#28172,#28173,#28174,
#28175,#28176,#28177,#28178,#28179,#28180,#28181,#28182,#28183,#28184,#28185,
#28186,#28187,#28188,#28189,#28190,#28191,#28192,#28193,#28194,#28195,#28196,
#28197,#28198)),.UNSPECIFIED.,.F.,.F.,.F.,(4,4),(4,1,1,1,1,1,1,1,1,1,1,
1,1,1,1,1,1,1,1,1,1,1,1,1,1,1,1,1,1,1,1,1,1,1,1,1,1,1,1,1,1,1,1,1,1,1,1,
1,1,1,1,1,1,4),(0.,0.0321584099938621),(14.3984001269718,15.3849294656359,
16.3714588042999,17.3579881429639,18.344517481628,19.331046820292,20.317576158956,
21.30410549762,22.2906348362841,23.2771641749481,24.2636935136121,25.2502228522762,
26.2367521909402,27.2232815296042,28.2098108682683,29.1963402069323,30.1828695455963,
31.1693988842604,32.1559282229244,33.1424575615884,34.1289869002524,35.1155162389165,
36.1020455775805,37.0885749162445,38.0751042549086,39.0616335935726,40.0481629322366,
41.0346922709007,42.0212216095647,43.0077509482287,43.9942802868928,44.9808096255568,
45.9673389642208,46.9538683028848,47.9403976415489,48.9269269802129,49.9134563188769,
50.899985657541,51.886514996205,52.873044334869,53.8595736735331,54.8461030121971,
55.8326323508611,56.8191616895251,57.8056910281892,58.7922203668532,59.7787497055172,
60.7652790441813,61.7518083828453,62.7383377215093,63.7248670601734,64.7113963988374,
65.6979257375014,66.6844550761655),.UNSPECIFIED.);
#240=B_SPLINE_SURFACE_WITH_KNOTS('',3,3,((#28411,#28412,#28413,#28414,#28415,
#28416,#28417,#28418,#28419,#28420,#28421,#28422,#28423,#28424,#28425,#28426,
#28427,#28428,#28429,#28430,#28431,#28432,#28433,#28434,#28435,#28436,#28437,
#28438,#28439,#28440,#28441,#28442,#28443,#28444,#28445,#28446,#28447,#28448,
#28449,#28450,#28451,#28452,#28453,#28454,#28455,#28456,#28457,#28458,#28459,
#28460,#28461,#28462,#28463,#28464,#28465,#28466,#28467,#28468,#28469,#28470,
#28471,#28472,#28473,#28474,#28475,#28476,#28477,#28478,#28479,#28480,#28481,
#28482,#28483,#28484,#28485,#28486,#28487,#28488,#28489,#28490,#28491,#28492,
#28493,#28494,#28495,#28496),(#28497,#28498,#28499,#28500,#28501,#28502,
#28503,#28504,#28505,#28506,#28507,#28508,#28509,#28510,#28511,#28512,#28513,
#28514,#28515,#28516,#28517,#28518,#28519,#28520,#28521,#28522,#28523,#28524,
#28525,#28526,#28527,#28528,#28529,#28530,#28531,#28532,#28533,#28534,#28535,
#28536,#28537,#28538,#28539,#28540,#28541,#28542,#28543,#28544,#28545,#28546,
#28547,#28548,#28549,#28550,#28551,#28552,#28553,#28554,#28555,#28556,#28557,
#28558,#28559,#28560,#28561,#28562,#28563,#28564,#28565,#28566,#28567,#28568,
#28569,#28570,#28571,#28572,#28573,#28574,#28575,#28576,#28577,#28578,#28579,
#28580,#28581,#28582),(#28583,#28584,#28585,#28586,#28587,#28588,#28589,
#28590,#28591,#28592,#28593,#28594,#28595,#28596,#28597,#28598,#28599,#28600,
#28601,#28602,#28603,#28604,#28605,#28606,#28607,#28608,#28609,#28610,#28611,
#28612,#28613,#28614,#28615,#28616,#28617,#28618,#28619,#28620,#28621,#28622,
#28623,#28624,#28625,#28626,#28627,#28628,#28629,#28630,#28631,#28632,#28633,
#28634,#28635,#28636,#28637,#28638,#28639,#28640,#28641,#28642,#28643,#28644,
#28645,#28646,#28647,#28648,#28649,#28650,#28651,#28652,#28653,#28654,#28655,
#28656,#28657,#28658,#28659,#28660,#28661,#28662,#28663,#28664,#28665,#28666,
#28667,#28668),(#28669,#28670,#28671,#28672,#28673,#28674,#28675,#28676,
#28677,#28678,#28679,#28680,#28681,#28682,#28683,#28684,#28685,#28686,#28687,
#28688,#28689,#28690,#28691,#28692,#28693,#28694,#28695,#28696,#28697,#28698,
#28699,#28700,#28701,#28702,#28703,#28704,#28705,#28706,#28707,#28708,#28709,
#28710,#28711,#28712,#28713,#28714,#28715,#28716,#28717,#28718,#28719,#28720,
#28721,#28722,#28723,#28724,#28725,#28726,#28727,#28728,#28729,#28730,#28731,
#28732,#28733,#28734,#28735,#28736,#28737,#28738,#28739,#28740,#28741,#28742,
#28743,#28744,#28745,#28746,#28747,#28748,#28749,#28750,#28751,#28752,#28753,
#28754)),.UNSPECIFIED.,.F.,.F.,.F.,(4,4),(4,1,1,1,1,1,1,1,1,1,1,1,1,1,1,
1,1,1,1,1,1,1,1,1,1,1,1,1,1,1,1,1,1,1,1,1,1,1,1,1,1,1,1,1,1,1,1,1,1,1,1,
1,1,1,1,1,1,1,1,1,1,1,1,1,1,1,1,1,1,1,1,1,1,1,1,1,1,1,1,1,1,1,1,4),(0.,
0.0448889834294937),(11.8615800042566,12.8591513772395,13.8567227502225,
14.8542941232054,15.8518654961883,16.8494368691713,17.8470082421542,18.8445796151371,
19.8421509881201,20.839722361103,21.837293734086,22.8348651070689,23.8324364800518,
24.8300078530348,25.8275792260177,26.8251505990006,27.8227219719836,28.8202933449665,
29.8178647179494,30.8154360909324,31.8130074639153,32.8105788368982,33.8081502098812,
34.8057215828641,35.803292955847,36.80086432883,37.7984357018129,38.7960070747958,
39.7935784477788,40.7911498207617,41.7887211937446,42.7862925667276,43.7838639397105,
44.7814353126934,45.7790066856764,46.7765780586593,47.7741494316422,48.7717208046252,
49.7692921776081,50.766863550591,51.764434923574,52.7620062965569,53.7595776695398,
54.7571490425228,55.7547204155057,56.7522917884886,57.7498631614716,58.7474345344545,
59.7450059074374,60.7425772804204,61.7401486534033,62.7377200263862,63.7352913993692,
64.7328627723521,65.730434145335,66.728005518318,67.7255768913009,68.7231482642838,
69.7207196372668,70.7182910102497,71.7158623832326,72.7134337562156,73.7110051291985,
74.7085765021814,75.7061478751644,76.7037192481473,77.7012906211302,78.6988619941132,
79.6964333670961,80.6940047400791,81.691576113062,82.6891474860449,83.6867188590278,
84.6842902320108,85.6818616049937,86.6794329779766,87.6770043509596,88.6745757239425,
89.6721470969255,90.6697184699084,91.6672898428913,92.6648612158743,93.6624325888572,
94.6600039618401),.UNSPECIFIED.);
#241=B_SPLINE_SURFACE_WITH_KNOTS('',3,3,((#28832,#28833,#28834,#28835,#28836,
#28837,#28838,#28839,#28840,#28841,#28842,#28843,#28844,#28845,#28846,#28847,
#28848,#28849,#28850,#28851,#28852,#28853,#28854,#28855,#28856,#28857,#28858,
#28859,#28860,#28861,#28862,#28863,#28864,#28865,#28866,#28867,#28868,#28869,
#28870,#28871,#28872,#28873,#28874,#28875,#28876,#28877,#28878,#28879,#28880,
#28881,#28882,#28883,#28884,#28885,#28886,#28887,#28888,#28889,#28890,#28891,
#28892,#28893,#28894,#28895,#28896,#28897,#28898,#28899,#28900,#28901,#28902,
#28903,#28904,#28905,#28906,#28907,#28908,#28909,#28910,#28911,#28912,#28913,
#28914,#28915,#28916,#28917),(#28918,#28919,#28920,#28921,#28922,#28923,
#28924,#28925,#28926,#28927,#28928,#28929,#28930,#28931,#28932,#28933,#28934,
#28935,#28936,#28937,#28938,#28939,#28940,#28941,#28942,#28943,#28944,#28945,
#28946,#28947,#28948,#28949,#28950,#28951,#28952,#28953,#28954,#28955,#28956,
#28957,#28958,#28959,#28960,#28961,#28962,#28963,#28964,#28965,#28966,#28967,
#28968,#28969,#28970,#28971,#28972,#28973,#28974,#28975,#28976,#28977,#28978,
#28979,#28980,#28981,#28982,#28983,#28984,#28985,#28986,#28987,#28988,#28989,
#28990,#28991,#28992,#28993,#28994,#28995,#28996,#28997,#28998,#28999,#29000,
#29001,#29002,#29003),(#29004,#29005,#29006,#29007,#29008,#29009,#29010,
#29011,#29012,#29013,#29014,#29015,#29016,#29017,#29018,#29019,#29020,#29021,
#29022,#29023,#29024,#29025,#29026,#29027,#29028,#29029,#29030,#29031,#29032,
#29033,#29034,#29035,#29036,#29037,#29038,#29039,#29040,#29041,#29042,#29043,
#29044,#29045,#29046,#29047,#29048,#29049,#29050,#29051,#29052,#29053,#29054,
#29055,#29056,#29057,#29058,#29059,#29060,#29061,#29062,#29063,#29064,#29065,
#29066,#29067,#29068,#29069,#29070,#29071,#29072,#29073,#29074,#29075,#29076,
#29077,#29078,#29079,#29080,#29081,#29082,#29083,#29084,#29085,#29086,#29087,
#29088,#29089),(#29090,#29091,#29092,#29093,#29094,#29095,#29096,#29097,
#29098,#29099,#29100,#29101,#29102,#29103,#29104,#29105,#29106,#29107,#29108,
#29109,#29110,#29111,#29112,#29113,#29114,#29115,#29116,#29117,#29118,#29119,
#29120,#29121,#29122,#29123,#29124,#29125,#29126,#29127,#29128,#29129,#29130,
#29131,#29132,#29133,#29134,#29135,#29136,#29137,#29138,#29139,#29140,#29141,
#29142,#29143,#29144,#29145,#29146,#29147,#29148,#29149,#29150,#29151,#29152,
#29153,#29154,#29155,#29156,#29157,#29158,#29159,#29160,#29161,#29162,#29163,
#29164,#29165,#29166,#29167,#29168,#29169,#29170,#29171,#29172,#29173,#29174,
#29175)),.UNSPECIFIED.,.F.,.F.,.F.,(4,4),(4,1,1,1,1,1,1,1,1,1,1,1,1,1,1,
1,1,1,1,1,1,1,1,1,1,1,1,1,1,1,1,1,1,1,1,1,1,1,1,1,1,1,1,1,1,1,1,1,1,1,1,
1,1,1,1,1,1,1,1,1,1,1,1,1,1,1,1,1,1,1,1,1,1,1,1,1,1,1,1,1,1,1,1,4),(0.,
0.0448889834294937),(14.3981410127768,15.3957123857598,16.3932837587427,
17.3908551317256,18.3884265047086,19.3859978776915,20.3835692506744,21.3811406236574,
22.3787119966403,23.3762833696232,24.3738547426062,25.3714261155891,26.368997488572,
27.366568861555,28.3641402345379,29.3617116075208,30.3592829805038,31.3568543534867,
32.3544257264696,33.3519970994526,34.3495684724355,35.3471398454184,36.3447112184014,
37.3422825913843,38.3398539643672,39.3374253373502,40.3349967103331,41.332568083316,
42.330139456299,43.3277108292819,44.3252822022648,45.3228535752478,46.3204249482307,
47.3179963212136,48.3155676941966,49.3131390671795,50.3107104401624,51.3082818131454,
52.3058531861283,53.3034245591112,54.3009959320942,55.2985673050771,56.29613867806,
57.293710051043,58.2912814240259,59.2888527970089,60.2864241699918,61.2839955429747,
62.2815669159576,63.2791382889406,64.2767096619235,65.2742810349065,66.2718524078894,
67.2694237808723,68.2669951538552,69.2645665268382,70.2621378998211,71.2597092728041,
72.257280645787,73.2548520187699,74.2524233917528,75.2499947647358,76.2475661377187,
77.2451375107017,78.2427088836846,79.2402802566675,80.2378516296505,81.2354230026334,
82.2329943756163,83.2305657485992,84.2281371215822,85.2257084945651,86.2232798675481,
87.220851240531,88.2184226135139,89.2159939864968,90.2135653594798,91.2111367324627,
92.2087081054457,93.2062794784286,94.2038508514115,95.2014222243945,96.1989935973774,
97.1965649703603),.UNSPECIFIED.);
#242=B_SPLINE_SURFACE_WITH_KNOTS('',3,3,((#29398,#29399,#29400,#29401,#29402,
#29403,#29404,#29405,#29406,#29407,#29408,#29409,#29410,#29411,#29412,#29413,
#29414,#29415,#29416,#29417,#29418,#29419,#29420,#29421,#29422,#29423,#29424,
#29425,#29426,#29427,#29428,#29429,#29430,#29431,#29432,#29433,#29434,#29435,
#29436,#29437,#29438),(#29439,#29440,#29441,#29442,#29443,#29444,#29445,
#29446,#29447,#29448,#29449,#29450,#29451,#29452,#29453,#29454,#29455,#29456,
#29457,#29458,#29459,#29460,#29461,#29462,#29463,#29464,#29465,#29466,#29467,
#29468,#29469,#29470,#29471,#29472,#29473,#29474,#29475,#29476,#29477,#29478,
#29479),(#29480,#29481,#29482,#29483,#29484,#29485,#29486,#29487,#29488,
#29489,#29490,#29491,#29492,#29493,#29494,#29495,#29496,#29497,#29498,#29499,
#29500,#29501,#29502,#29503,#29504,#29505,#29506,#29507,#29508,#29509,#29510,
#29511,#29512,#29513,#29514,#29515,#29516,#29517,#29518,#29519,#29520),
(#29521,#29522,#29523,#29524,#29525,#29526,#29527,#29528,#29529,#29530,
#29531,#29532,#29533,#29534,#29535,#29536,#29537,#29538,#29539,#29540,#29541,
#29542,#29543,#29544,#29545,#29546,#29547,#29548,#29549,#29550,#29551,#29552,
#29553,#29554,#29555,#29556,#29557,#29558,#29559,#29560,#29561),(#29562,
#29563,#29564,#29565,#29566,#29567,#29568,#29569,#29570,#29571,#29572,#29573,
#29574,#29575,#29576,#29577,#29578,#29579,#29580,#29581,#29582,#29583,#29584,
#29585,#29586,#29587,#29588,#29589,#29590,#29591,#29592,#29593,#29594,#29595,
#29596,#29597,#29598,#29599,#29600,#29601,#29602),(#29603,#29604,#29605,
#29606,#29607,#29608,#29609,#29610,#29611,#29612,#29613,#29614,#29615,#29616,
#29617,#29618,#29619,#29620,#29621,#29622,#29623,#29624,#29625,#29626,#29627,
#29628,#29629,#29630,#29631,#29632,#29633,#29634,#29635,#29636,#29637,#29638,
#29639,#29640,#29641,#29642,#29643),(#29644,#29645,#29646,#29647,#29648,
#29649,#29650,#29651,#29652,#29653,#29654,#29655,#29656,#29657,#29658,#29659,
#29660,#29661,#29662,#29663,#29664,#29665,#29666,#29667,#29668,#29669,#29670,
#29671,#29672,#29673,#29674,#29675,#29676,#29677,#29678,#29679,#29680,#29681,
#29682,#29683,#29684),(#29685,#29686,#29687,#29688,#29689,#29690,#29691,
#29692,#29693,#29694,#29695,#29696,#29697,#29698,#29699,#29700,#29701,#29702,
#29703,#29704,#29705,#29706,#29707,#29708,#29709,#29710,#29711,#29712,#29713,
#29714,#29715,#29716,#29717,#29718,#29719,#29720,#29721,#29722,#29723,#29724,
#29725),(#29726,#29727,#29728,#29729,#29730,#29731,#29732,#29733,#29734,
#29735,#29736,#29737,#29738,#29739,#29740,#29741,#29742,#29743,#29744,#29745,
#29746,#29747,#29748,#29749,#29750,#29751,#29752,#29753,#29754,#29755,#29756,
#29757,#29758,#29759,#29760,#29761,#29762,#29763,#29764,#29765,#29766),
(#29767,#29768,#29769,#29770,#29771,#29772,#29773,#29774,#29775,#29776,
#29777,#29778,#29779,#29780,#29781,#29782,#29783,#29784,#29785,#29786,#29787,
#29788,#29789,#29790,#29791,#29792,#29793,#29794,#29795,#29796,#29797,#29798,
#29799,#29800,#29801,#29802,#29803,#29804,#29805,#29806,#29807)),
 .UNSPECIFIED.,.T.,.F.,.F.,(4,1,1,1,1,1,1,4),(4,1,1,1,1,1,1,1,1,1,1,1,1,
1,1,1,1,1,1,1,1,1,1,1,1,1,1,1,1,1,1,1,1,1,1,1,1,1,4),(-3.14159265358979,
-2.24399475256414,-1.34639685153848,-0.448798950512828,0.448798950512828,
1.34639685153848,2.24399475256414,3.14159265358979),(0.,0.496040945303652,
0.992081890607303,1.48812283591095,1.98416378121461,2.48020472651826,2.97624567182191,
3.47228661712556,3.96832756242921,4.46436850773286,4.96040945303652,5.45645039834017,
5.95249134364382,6.44853228894747,6.94457323425112,7.44061417955477,7.93665512485842,
8.43269607016208,8.92873701546573,9.42477796076938,9.92081890607303,10.4168598513767,
10.9129007966803,11.408941741984,11.9049826872876,12.4010236325913,12.8970645778949,
13.3931055231986,13.8891464685022,14.3851874138059,14.8812283591095,15.3772693044132,
15.8733102497168,16.3693511950205,16.8653921403242,17.3614330856278,17.8574740309315,
18.3535149762351,18.8495559215388),.UNSPECIFIED.);
#243=B_SPLINE_SURFACE_WITH_KNOTS('',3,3,((#32192,#32193,#32194,#32195,#32196,
#32197,#32198,#32199,#32200,#32201,#32202,#32203,#32204,#32205,#32206,#32207,
#32208,#32209,#32210,#32211,#32212,#32213,#32214,#32215,#32216,#32217,#32218,
#32219,#32220,#32221,#32222,#32223,#32224,#32225,#32226,#32227,#32228,#32229,
#32230,#32231,#32232,#32233,#32234,#32235,#32236,#32237,#32238,#32239,#32240,
#32241,#32242,#32243,#32244,#32245,#32246,#32247,#32248,#32249,#32250,#32251,
#32252,#32253,#32254,#32255,#32256,#32257,#32258,#32259,#32260,#32261,#32262,
#32263,#32264,#32265,#32266,#32267,#32268,#32269,#32270,#32271,#32272,#32273,
#32274,#32275,#32276,#32277,#32278,#32279,#32280,#32281,#32282,#32283,#32284,
#32285,#32286,#32287,#32288,#32289,#32290,#32291,#32292,#32293,#32294,#32295,
#32296,#32297,#32298,#32299,#32300,#32301,#32302,#32303,#32304,#32305,#32306,
#32307,#32308,#32309,#32310),(#32311,#32312,#32313,#32314,#32315,#32316,
#32317,#32318,#32319,#32320,#32321,#32322,#32323,#32324,#32325,#32326,#32327,
#32328,#32329,#32330,#32331,#32332,#32333,#32334,#32335,#32336,#32337,#32338,
#32339,#32340,#32341,#32342,#32343,#32344,#32345,#32346,#32347,#32348,#32349,
#32350,#32351,#32352,#32353,#32354,#32355,#32356,#32357,#32358,#32359,#32360,
#32361,#32362,#32363,#32364,#32365,#32366,#32367,#32368,#32369,#32370,#32371,
#32372,#32373,#32374,#32375,#32376,#32377,#32378,#32379,#32380,#32381,#32382,
#32383,#32384,#32385,#32386,#32387,#32388,#32389,#32390,#32391,#32392,#32393,
#32394,#32395,#32396,#32397,#32398,#32399,#32400,#32401,#32402,#32403,#32404,
#32405,#32406,#32407,#32408,#32409,#32410,#32411,#32412,#32413,#32414,#32415,
#32416,#32417,#32418,#32419,#32420,#32421,#32422,#32423,#32424,#32425,#32426,
#32427,#32428,#32429),(#32430,#32431,#32432,#32433,#32434,#32435,#32436,
#32437,#32438,#32439,#32440,#32441,#32442,#32443,#32444,#32445,#32446,#32447,
#32448,#32449,#32450,#32451,#32452,#32453,#32454,#32455,#32456,#32457,#32458,
#32459,#32460,#32461,#32462,#32463,#32464,#32465,#32466,#32467,#32468,#32469,
#32470,#32471,#32472,#32473,#32474,#32475,#32476,#32477,#32478,#32479,#32480,
#32481,#32482,#32483,#32484,#32485,#32486,#32487,#32488,#32489,#32490,#32491,
#32492,#32493,#32494,#32495,#32496,#32497,#32498,#32499,#32500,#32501,#32502,
#32503,#32504,#32505,#32506,#32507,#32508,#32509,#32510,#32511,#32512,#32513,
#32514,#32515,#32516,#32517,#32518,#32519,#32520,#32521,#32522,#32523,#32524,
#32525,#32526,#32527,#32528,#32529,#32530,#32531,#32532,#32533,#32534,#32535,
#32536,#32537,#32538,#32539,#32540,#32541,#32542,#32543,#32544,#32545,#32546,
#32547,#32548),(#32549,#32550,#32551,#32552,#32553,#32554,#32555,#32556,
#32557,#32558,#32559,#32560,#32561,#32562,#32563,#32564,#32565,#32566,#32567,
#32568,#32569,#32570,#32571,#32572,#32573,#32574,#32575,#32576,#32577,#32578,
#32579,#32580,#32581,#32582,#32583,#32584,#32585,#32586,#32587,#32588,#32589,
#32590,#32591,#32592,#32593,#32594,#32595,#32596,#32597,#32598,#32599,#32600,
#32601,#32602,#32603,#32604,#32605,#32606,#32607,#32608,#32609,#32610,#32611,
#32612,#32613,#32614,#32615,#32616,#32617,#32618,#32619,#32620,#32621,#32622,
#32623,#32624,#32625,#32626,#32627,#32628,#32629,#32630,#32631,#32632,#32633,
#32634,#32635,#32636,#32637,#32638,#32639,#32640,#32641,#32642,#32643,#32644,
#32645,#32646,#32647,#32648,#32649,#32650,#32651,#32652,#32653,#32654,#32655,
#32656,#32657,#32658,#32659,#32660,#32661,#32662,#32663,#32664,#32665,#32666,
#32667)),.UNSPECIFIED.,.F.,.F.,.F.,(4,4),(4,1,1,1,1,1,1,1,1,1,1,1,1,1,1,
1,1,1,1,1,1,1,1,1,1,1,1,1,1,1,1,1,1,1,1,1,1,1,1,1,1,1,1,1,1,1,1,1,1,1,1,
1,1,1,1,1,1,1,1,1,1,1,1,1,1,1,1,1,1,1,1,1,1,1,1,1,1,1,1,1,1,1,1,1,1,1,1,
1,1,1,1,1,1,1,1,1,1,1,1,1,1,1,1,1,1,1,1,1,1,1,1,1,1,1,1,1,4),(0.,0.0321584099938621),
(11.8553612635792,12.8477570223809,13.8401527811825,14.8325485399841,15.8249442987858,
16.8173400575874,17.809735816389,18.8021315751907,19.7945273339923,20.7869230927939,
21.7793188515956,22.7717146103972,23.7641103691988,24.7565061280005,25.7489018868021,
26.7412976456037,27.7336934044054,28.726089163207,29.7184849220086,30.7108806808103,
31.7032764396119,32.6956721984135,33.6880679572152,34.6804637160168,35.6728594748184,
36.6652552336201,37.6576509924217,38.6500467512233,39.642442510025,40.6348382688266,
41.6272340276282,42.6196297864299,43.6120255452315,44.6044213040331,45.5968170628348,
46.5892128216364,47.581608580438,48.5740043392397,49.5664000980413,50.5587958568429,
51.5511916156446,52.5435873744462,53.5359831332478,54.5283788920495,55.5207746508511,
56.5131704096527,57.5055661684544,58.497961927256,59.4903576860576,60.4827534448593,
61.4751492036609,62.4675449624625,63.4599407212642,64.4523364800658,65.4447322388674,
66.4371279976691,67.4295237564707,68.4219195152723,69.4143152740739,70.4067110328756,
71.3991067916772,72.3915025504788,73.3838983092805,74.3762940680821,75.3686898268838,
76.3610855856854,77.353481344487,78.3458771032886,79.3382728620903,80.3306686208919,
81.3230643796935,82.3154601384952,83.3078558972968,84.3002516560985,85.2926474149001,
86.2850431737017,87.2774389325033,88.269834691305,89.2622304501066,90.2546262089082,
91.2470219677099,92.2394177265115,93.2318134853131,94.2242092441148,95.2166050029164,
96.209000761718,97.2013965205197,98.1937922793213,99.1861880381229,100.178583796925,
101.170979555726,102.163375314528,103.155771073329,104.148166832131,105.140562590933,
106.132958349734,107.125354108536,108.117749867338,109.110145626139,110.102541384941,
111.094937143743,112.087332902544,113.079728661346,114.072124420147,115.064520178949,
116.056915937751,117.049311696552,118.041707455354,119.034103214156,120.026498972957,
121.018894731759,122.01129049056,123.003686249362,123.996082008164,124.988477766965,
125.980873525767,126.973269284569),.UNSPECIFIED.);
#244=B_SPLINE_SURFACE_WITH_KNOTS('',3,3,((#32742,#32743,#32744,#32745,#32746,
#32747,#32748,#32749,#32750,#32751,#32752,#32753,#32754,#32755,#32756,#32757,
#32758,#32759,#32760,#32761,#32762,#32763,#32764,#32765,#32766,#32767,#32768,
#32769,#32770,#32771,#32772,#32773,#32774,#32775,#32776,#32777,#32778,#32779,
#32780,#32781,#32782,#32783,#32784,#32785,#32786,#32787,#32788,#32789,#32790,
#32791,#32792,#32793,#32794,#32795,#32796,#32797,#32798,#32799,#32800,#32801,
#32802,#32803,#32804,#32805,#32806,#32807,#32808,#32809,#32810,#32811,#32812,
#32813,#32814,#32815,#32816,#32817,#32818,#32819,#32820,#32821,#32822,#32823,
#32824,#32825,#32826,#32827,#32828,#32829,#32830,#32831,#32832,#32833,#32834,
#32835,#32836,#32837,#32838,#32839,#32840,#32841,#32842,#32843,#32844,#32845,
#32846,#32847,#32848,#32849,#32850,#32851,#32852,#32853,#32854,#32855,#32856,
#32857,#32858,#32859,#32860),(#32861,#32862,#32863,#32864,#32865,#32866,
#32867,#32868,#32869,#32870,#32871,#32872,#32873,#32874,#32875,#32876,#32877,
#32878,#32879,#32880,#32881,#32882,#32883,#32884,#32885,#32886,#32887,#32888,
#32889,#32890,#32891,#32892,#32893,#32894,#32895,#32896,#32897,#32898,#32899,
#32900,#32901,#32902,#32903,#32904,#32905,#32906,#32907,#32908,#32909,#32910,
#32911,#32912,#32913,#32914,#32915,#32916,#32917,#32918,#32919,#32920,#32921,
#32922,#32923,#32924,#32925,#32926,#32927,#32928,#32929,#32930,#32931,#32932,
#32933,#32934,#32935,#32936,#32937,#32938,#32939,#32940,#32941,#32942,#32943,
#32944,#32945,#32946,#32947,#32948,#32949,#32950,#32951,#32952,#32953,#32954,
#32955,#32956,#32957,#32958,#32959,#32960,#32961,#32962,#32963,#32964,#32965,
#32966,#32967,#32968,#32969,#32970,#32971,#32972,#32973,#32974,#32975,#32976,
#32977,#32978,#32979),(#32980,#32981,#32982,#32983,#32984,#32985,#32986,
#32987,#32988,#32989,#32990,#32991,#32992,#32993,#32994,#32995,#32996,#32997,
#32998,#32999,#33000,#33001,#33002,#33003,#33004,#33005,#33006,#33007,#33008,
#33009,#33010,#33011,#33012,#33013,#33014,#33015,#33016,#33017,#33018,#33019,
#33020,#33021,#33022,#33023,#33024,#33025,#33026,#33027,#33028,#33029,#33030,
#33031,#33032,#33033,#33034,#33035,#33036,#33037,#33038,#33039,#33040,#33041,
#33042,#33043,#33044,#33045,#33046,#33047,#33048,#33049,#33050,#33051,#33052,
#33053,#33054,#33055,#33056,#33057,#33058,#33059,#33060,#33061,#33062,#33063,
#33064,#33065,#33066,#33067,#33068,#33069,#33070,#33071,#33072,#33073,#33074,
#33075,#33076,#33077,#33078,#33079,#33080,#33081,#33082,#33083,#33084,#33085,
#33086,#33087,#33088,#33089,#33090,#33091,#33092,#33093,#33094,#33095,#33096,
#33097,#33098),(#33099,#33100,#33101,#33102,#33103,#33104,#33105,#33106,
#33107,#33108,#33109,#33110,#33111,#33112,#33113,#33114,#33115,#33116,#33117,
#33118,#33119,#33120,#33121,#33122,#33123,#33124,#33125,#33126,#33127,#33128,
#33129,#33130,#33131,#33132,#33133,#33134,#33135,#33136,#33137,#33138,#33139,
#33140,#33141,#33142,#33143,#33144,#33145,#33146,#33147,#33148,#33149,#33150,
#33151,#33152,#33153,#33154,#33155,#33156,#33157,#33158,#33159,#33160,#33161,
#33162,#33163,#33164,#33165,#33166,#33167,#33168,#33169,#33170,#33171,#33172,
#33173,#33174,#33175,#33176,#33177,#33178,#33179,#33180,#33181,#33182,#33183,
#33184,#33185,#33186,#33187,#33188,#33189,#33190,#33191,#33192,#33193,#33194,
#33195,#33196,#33197,#33198,#33199,#33200,#33201,#33202,#33203,#33204,#33205,
#33206,#33207,#33208,#33209,#33210,#33211,#33212,#33213,#33214,#33215,#33216,
#33217)),.UNSPECIFIED.,.F.,.F.,.F.,(4,4),(4,1,1,1,1,1,1,1,1,1,1,1,1,1,1,
1,1,1,1,1,1,1,1,1,1,1,1,1,1,1,1,1,1,1,1,1,1,1,1,1,1,1,1,1,1,1,1,1,1,1,1,
1,1,1,1,1,1,1,1,1,1,1,1,1,1,1,1,1,1,1,1,1,1,1,1,1,1,1,1,1,1,1,1,1,1,1,1,
1,1,1,1,1,1,1,1,1,1,1,1,1,1,1,1,1,1,1,1,1,1,1,1,1,1,1,1,1,4),(0.,0.0321584099938621),
(14.3984001269718,15.3907958857734,16.383191644575,17.3755874033767,18.3679831621783,
19.3603789209799,20.3527746797816,21.3451704385832,22.3375661973848,23.3299619561865,
24.3223577149881,25.3147534737897,26.3071492325914,27.299544991393,28.2919407501946,
29.2843365089963,30.2767322677979,31.2691280265995,32.2615237854012,33.2539195442028,
34.2463153030044,35.2387110618061,36.2311068206077,37.2235025794093,38.215898338211,
39.2082940970126,40.2006898558142,41.1930856146159,42.1854813734175,43.1778771322191,
44.1702728910208,45.1626686498224,46.155064408624,47.1474601674257,48.1398559262273,
49.1322516850289,50.1246474438306,51.1170432026322,52.1094389614338,53.1018347202355,
54.0942304790371,55.0866262378387,56.0790219966403,57.071417755442,58.0638135142436,
59.0562092730452,60.0486050318469,61.0410007906485,62.0333965494501,63.0257923082518,
64.0181880670534,65.010583825855,66.0029795846567,66.9953753434583,67.9877711022599,
68.9801668610616,69.9725626198632,70.9649583786648,71.9573541374665,72.9497498962681,
73.9421456550697,74.9345414138714,75.926937172673,76.9193329314746,77.9117286902763,
78.9041244490779,79.8965202078795,80.8889159666812,81.8813117254828,82.8737074842844,
83.8661032430861,84.8584990018877,85.8508947606893,86.8432905194909,87.8356862782926,
88.8280820370942,89.8204777958959,90.8128735546975,91.8052693134991,92.7976650723007,
93.7900608311024,94.782456589904,95.7748523487057,96.7672481075073,97.7596438663089,
98.7520396251105,99.7444353839122,100.736831142714,101.729226901515,102.721622660317,
103.714018419119,104.70641417792,105.698809936722,106.691205695524,107.683601454325,
108.675997213127,109.668392971929,110.66078873073,111.653184489532,112.645580248333,
113.637976007135,114.630371765937,115.622767524738,116.61516328354,117.607559042342,
118.599954801143,119.592350559945,120.584746318746,121.577142077548,122.56953783635,
123.561933595151,124.554329353953,125.546725112755,126.539120871556,127.531516630358,
128.52391238916,129.516308147961),.UNSPECIFIED.);
#245=B_SPLINE_SURFACE_WITH_KNOTS('',3,3,((#33424,#33425,#33426,#33427,#33428,
#33429,#33430,#33431,#33432,#33433,#33434,#33435,#33436,#33437,#33438,#33439,
#33440,#33441,#33442,#33443,#33444,#33445,#33446,#33447,#33448,#33449,#33450,
#33451,#33452,#33453,#33454,#33455,#33456,#33457,#33458,#33459,#33460,#33461,
#33462,#33463,#33464,#33465,#33466,#33467,#33468,#33469,#33470,#33471,#33472,
#33473,#33474,#33475,#33476,#33477,#33478,#33479,#33480,#33481,#33482,#33483,
#33484,#33485,#33486,#33487,#33488,#33489,#33490,#33491,#33492,#33493,#33494,
#33495,#33496,#33497,#33498,#33499,#33500,#33501,#33502,#33503,#33504,#33505,
#33506,#33507,#33508,#33509),(#33510,#33511,#33512,#33513,#33514,#33515,
#33516,#33517,#33518,#33519,#33520,#33521,#33522,#33523,#33524,#33525,#33526,
#33527,#33528,#33529,#33530,#33531,#33532,#33533,#33534,#33535,#33536,#33537,
#33538,#33539,#33540,#33541,#33542,#33543,#33544,#33545,#33546,#33547,#33548,
#33549,#33550,#33551,#33552,#33553,#33554,#33555,#33556,#33557,#33558,#33559,
#33560,#33561,#33562,#33563,#33564,#33565,#33566,#33567,#33568,#33569,#33570,
#33571,#33572,#33573,#33574,#33575,#33576,#33577,#33578,#33579,#33580,#33581,
#33582,#33583,#33584,#33585,#33586,#33587,#33588,#33589,#33590,#33591,#33592,
#33593,#33594,#33595),(#33596,#33597,#33598,#33599,#33600,#33601,#33602,
#33603,#33604,#33605,#33606,#33607,#33608,#33609,#33610,#33611,#33612,#33613,
#33614,#33615,#33616,#33617,#33618,#33619,#33620,#33621,#33622,#33623,#33624,
#33625,#33626,#33627,#33628,#33629,#33630,#33631,#33632,#33633,#33634,#33635,
#33636,#33637,#33638,#33639,#33640,#33641,#33642,#33643,#33644,#33645,#33646,
#33647,#33648,#33649,#33650,#33651,#33652,#33653,#33654,#33655,#33656,#33657,
#33658,#33659,#33660,#33661,#33662,#33663,#33664,#33665,#33666,#33667,#33668,
#33669,#33670,#33671,#33672,#33673,#33674,#33675,#33676,#33677,#33678,#33679,
#33680,#33681),(#33682,#33683,#33684,#33685,#33686,#33687,#33688,#33689,
#33690,#33691,#33692,#33693,#33694,#33695,#33696,#33697,#33698,#33699,#33700,
#33701,#33702,#33703,#33704,#33705,#33706,#33707,#33708,#33709,#33710,#33711,
#33712,#33713,#33714,#33715,#33716,#33717,#33718,#33719,#33720,#33721,#33722,
#33723,#33724,#33725,#33726,#33727,#33728,#33729,#33730,#33731,#33732,#33733,
#33734,#33735,#33736,#33737,#33738,#33739,#33740,#33741,#33742,#33743,#33744,
#33745,#33746,#33747,#33748,#33749,#33750,#33751,#33752,#33753,#33754,#33755,
#33756,#33757,#33758,#33759,#33760,#33761,#33762,#33763,#33764,#33765,#33766,
#33767)),.UNSPECIFIED.,.F.,.F.,.F.,(4,4),(4,1,1,1,1,1,1,1,1,1,1,1,1,1,1,
1,1,1,1,1,1,1,1,1,1,1,1,1,1,1,1,1,1,1,1,1,1,1,1,1,1,1,1,1,1,1,1,1,1,1,1,
1,1,1,1,1,1,1,1,1,1,1,1,1,1,1,1,1,1,1,1,1,1,1,1,1,1,1,1,1,1,1,1,4),(0.,
0.0448889834294934),(11.8615800042567,12.8591513772396,13.8567227502225,
14.8542941232054,15.8518654961884,16.8494368691713,17.8470082421542,18.8445796151372,
19.8421509881201,20.839722361103,21.837293734086,22.8348651070689,23.8324364800518,
24.8300078530348,25.8275792260177,26.8251505990006,27.8227219719836,28.8202933449665,
29.8178647179494,30.8154360909324,31.8130074639153,32.8105788368982,33.8081502098812,
34.8057215828641,35.803292955847,36.80086432883,37.7984357018129,38.7960070747958,
39.7935784477788,40.7911498207617,41.7887211937446,42.7862925667276,43.7838639397105,
44.7814353126934,45.7790066856764,46.7765780586593,47.7741494316422,48.7717208046252,
49.7692921776081,50.766863550591,51.764434923574,52.7620062965569,53.7595776695398,
54.7571490425228,55.7547204155057,56.7522917884886,57.7498631614716,58.7474345344545,
59.7450059074374,60.7425772804204,61.7401486534033,62.7377200263862,63.7352913993692,
64.7328627723521,65.730434145335,66.728005518318,67.7255768913009,68.7231482642838,
69.7207196372668,70.7182910102497,71.7158623832326,72.7134337562156,73.7110051291985,
74.7085765021814,75.7061478751643,76.7037192481473,77.7012906211302,78.6988619941132,
79.6964333670961,80.694004740079,81.691576113062,82.6891474860449,83.6867188590278,
84.6842902320108,85.6818616049937,86.6794329779766,87.6770043509595,88.6745757239425,
89.6721470969254,90.6697184699083,91.6672898428913,92.6648612158742,93.6624325888571,
94.6600039618401),.UNSPECIFIED.);
#246=B_SPLINE_SURFACE_WITH_KNOTS('',3,3,((#33845,#33846,#33847,#33848,#33849,
#33850,#33851,#33852,#33853,#33854,#33855,#33856,#33857,#33858,#33859,#33860,
#33861,#33862,#33863,#33864,#33865,#33866,#33867,#33868,#33869,#33870,#33871,
#33872,#33873,#33874,#33875,#33876,#33877,#33878,#33879,#33880,#33881,#33882,
#33883,#33884,#33885,#33886,#33887,#33888,#33889,#33890,#33891,#33892,#33893,
#33894,#33895,#33896,#33897,#33898,#33899,#33900,#33901,#33902,#33903,#33904,
#33905,#33906,#33907,#33908,#33909,#33910,#33911,#33912,#33913,#33914,#33915,
#33916,#33917,#33918,#33919,#33920,#33921,#33922,#33923,#33924,#33925,#33926,
#33927,#33928,#33929,#33930),(#33931,#33932,#33933,#33934,#33935,#33936,
#33937,#33938,#33939,#33940,#33941,#33942,#33943,#33944,#33945,#33946,#33947,
#33948,#33949,#33950,#33951,#33952,#33953,#33954,#33955,#33956,#33957,#33958,
#33959,#33960,#33961,#33962,#33963,#33964,#33965,#33966,#33967,#33968,#33969,
#33970,#33971,#33972,#33973,#33974,#33975,#33976,#33977,#33978,#33979,#33980,
#33981,#33982,#33983,#33984,#33985,#33986,#33987,#33988,#33989,#33990,#33991,
#33992,#33993,#33994,#33995,#33996,#33997,#33998,#33999,#34000,#34001,#34002,
#34003,#34004,#34005,#34006,#34007,#34008,#34009,#34010,#34011,#34012,#34013,
#34014,#34015,#34016),(#34017,#34018,#34019,#34020,#34021,#34022,#34023,
#34024,#34025,#34026,#34027,#34028,#34029,#34030,#34031,#34032,#34033,#34034,
#34035,#34036,#34037,#34038,#34039,#34040,#34041,#34042,#34043,#34044,#34045,
#34046,#34047,#34048,#34049,#34050,#34051,#34052,#34053,#34054,#34055,#34056,
#34057,#34058,#34059,#34060,#34061,#34062,#34063,#34064,#34065,#34066,#34067,
#34068,#34069,#34070,#34071,#34072,#34073,#34074,#34075,#34076,#34077,#34078,
#34079,#34080,#34081,#34082,#34083,#34084,#34085,#34086,#34087,#34088,#34089,
#34090,#34091,#34092,#34093,#34094,#34095,#34096,#34097,#34098,#34099,#34100,
#34101,#34102),(#34103,#34104,#34105,#34106,#34107,#34108,#34109,#34110,
#34111,#34112,#34113,#34114,#34115,#34116,#34117,#34118,#34119,#34120,#34121,
#34122,#34123,#34124,#34125,#34126,#34127,#34128,#34129,#34130,#34131,#34132,
#34133,#34134,#34135,#34136,#34137,#34138,#34139,#34140,#34141,#34142,#34143,
#34144,#34145,#34146,#34147,#34148,#34149,#34150,#34151,#34152,#34153,#34154,
#34155,#34156,#34157,#34158,#34159,#34160,#34161,#34162,#34163,#34164,#34165,
#34166,#34167,#34168,#34169,#34170,#34171,#34172,#34173,#34174,#34175,#34176,
#34177,#34178,#34179,#34180,#34181,#34182,#34183,#34184,#34185,#34186,#34187,
#34188)),.UNSPECIFIED.,.F.,.F.,.F.,(4,4),(4,1,1,1,1,1,1,1,1,1,1,1,1,1,1,
1,1,1,1,1,1,1,1,1,1,1,1,1,1,1,1,1,1,1,1,1,1,1,1,1,1,1,1,1,1,1,1,1,1,1,1,
1,1,1,1,1,1,1,1,1,1,1,1,1,1,1,1,1,1,1,1,1,1,1,1,1,1,1,1,1,1,1,1,4),(0.,
0.0448889834294934),(14.3981410127769,15.3957123857598,16.3932837587428,
17.3908551317257,18.3884265047086,19.3859978776916,20.3835692506745,21.3811406236574,
22.3787119966404,23.3762833696233,24.3738547426062,25.3714261155892,26.3689974885721,
27.366568861555,28.364140234538,29.3617116075209,30.3592829805038,31.3568543534868,
32.3544257264697,33.3519970994526,34.3495684724355,35.3471398454185,36.3447112184014,
37.3422825913843,38.3398539643673,39.3374253373502,40.3349967103331,41.3325680833161,
42.330139456299,43.3277108292819,44.3252822022649,45.3228535752478,46.3204249482307,
47.3179963212137,48.3155676941966,49.3131390671795,50.3107104401625,51.3082818131454,
52.3058531861283,53.3034245591113,54.3009959320942,55.2985673050771,56.2961386780601,
57.293710051043,58.2912814240259,59.2888527970089,60.2864241699918,61.2839955429747,
62.2815669159577,63.2791382889406,64.2767096619235,65.2742810349065,66.2718524078894,
67.2694237808723,68.2669951538553,69.2645665268382,70.2621378998211,71.2597092728041,
72.257280645787,73.2548520187699,74.2524233917529,75.2499947647358,76.2475661377187,
77.2451375107017,78.2427088836846,79.2402802566675,80.2378516296505,81.2354230026334,
82.2329943756163,83.2305657485993,84.2281371215822,85.2257084945651,86.2232798675481,
87.220851240531,88.2184226135139,89.2159939864969,90.2135653594798,91.2111367324627,
92.2087081054457,93.2062794784286,94.2038508514115,95.2014222243944,96.1989935973774,
97.1965649703603),.UNSPECIFIED.);
#247=B_SPLINE_SURFACE_WITH_KNOTS('',3,3,((#35123,#35124,#35125,#35126,#35127,
#35128,#35129,#35130,#35131,#35132,#35133,#35134,#35135,#35136,#35137,#35138,
#35139,#35140,#35141,#35142,#35143,#35144,#35145,#35146,#35147,#35148,#35149,
#35150,#35151,#35152,#35153,#35154,#35155,#35156,#35157,#35158,#35159,#35160,
#35161,#35162,#35163,#35164,#35165,#35166,#35167,#35168,#35169,#35170,#35171,
#35172,#35173,#35174,#35175,#35176,#35177,#35178,#35179,#35180,#35181,#35182,
#35183,#35184,#35185,#35186,#35187,#35188,#35189,#35190),(#35191,#35192,
#35193,#35194,#35195,#35196,#35197,#35198,#35199,#35200,#35201,#35202,#35203,
#35204,#35205,#35206,#35207,#35208,#35209,#35210,#35211,#35212,#35213,#35214,
#35215,#35216,#35217,#35218,#35219,#35220,#35221,#35222,#35223,#35224,#35225,
#35226,#35227,#35228,#35229,#35230,#35231,#35232,#35233,#35234,#35235,#35236,
#35237,#35238,#35239,#35240,#35241,#35242,#35243,#35244,#35245,#35246,#35247,
#35248,#35249,#35250,#35251,#35252,#35253,#35254,#35255,#35256,#35257,#35258),
(#35259,#35260,#35261,#35262,#35263,#35264,#35265,#35266,#35267,#35268,
#35269,#35270,#35271,#35272,#35273,#35274,#35275,#35276,#35277,#35278,#35279,
#35280,#35281,#35282,#35283,#35284,#35285,#35286,#35287,#35288,#35289,#35290,
#35291,#35292,#35293,#35294,#35295,#35296,#35297,#35298,#35299,#35300,#35301,
#35302,#35303,#35304,#35305,#35306,#35307,#35308,#35309,#35310,#35311,#35312,
#35313,#35314,#35315,#35316,#35317,#35318,#35319,#35320,#35321,#35322,#35323,
#35324,#35325,#35326),(#35327,#35328,#35329,#35330,#35331,#35332,#35333,
#35334,#35335,#35336,#35337,#35338,#35339,#35340,#35341,#35342,#35343,#35344,
#35345,#35346,#35347,#35348,#35349,#35350,#35351,#35352,#35353,#35354,#35355,
#35356,#35357,#35358,#35359,#35360,#35361,#35362,#35363,#35364,#35365,#35366,
#35367,#35368,#35369,#35370,#35371,#35372,#35373,#35374,#35375,#35376,#35377,
#35378,#35379,#35380,#35381,#35382,#35383,#35384,#35385,#35386,#35387,#35388,
#35389,#35390,#35391,#35392,#35393,#35394)),.UNSPECIFIED.,.F.,.F.,.F.,(4,
4),(4,1,1,1,1,1,1,1,1,1,1,1,1,1,1,1,1,1,1,1,1,1,1,1,1,1,1,1,1,1,1,1,1,1,
1,1,1,1,1,1,1,1,1,1,1,1,1,1,1,1,1,1,1,1,1,1,1,1,1,1,1,1,1,1,1,4),(0.,0.0321584099938621),
(11.8553612635792,12.8530908876339,13.8508205116886,14.8485501357432,15.8462797597979,
16.8440093838525,17.8417390079072,18.8394686319618,19.8371982560165,20.8349278800712,
21.8326575041258,22.8303871281805,23.8281167522351,24.8258463762898,25.8235760003445,
26.8213056243991,27.8190352484538,28.8167648725084,29.8144944965631,30.8122241206177,
31.8099537446724,32.8076833687271,33.8054129927817,34.8031426168364,35.800872240891,
36.7986018649457,37.7963314890004,38.794061113055,39.7917907371097,40.7895203611643,
41.787249985219,42.7849796092736,43.7827092333283,44.780438857383,45.7781684814376,
46.7758981054923,47.7736277295469,48.7713573536016,49.7690869776563,50.7668166017109,
51.7645462257656,52.7622758498202,53.7600054738749,54.7577350979295,55.7554647219842,
56.7531943460389,57.7509239700935,58.7486535941482,59.7463832182028,60.7441128422575,
61.7418424663121,62.7395720903668,63.7373017144215,64.7350313384761,65.7327609625308,
66.7304905865854,67.7282202106401,68.7259498346948,69.7236794587494,70.7214090828041,
71.7191387068587,72.7168683309134,73.7145979549681,74.7123275790227,75.7100572030774,
76.707786827132),.UNSPECIFIED.);
#248=B_SPLINE_SURFACE_WITH_KNOTS('',3,3,((#35469,#35470,#35471,#35472,#35473,
#35474,#35475,#35476,#35477,#35478,#35479,#35480,#35481,#35482,#35483,#35484,
#35485,#35486,#35487,#35488,#35489,#35490,#35491,#35492,#35493,#35494,#35495,
#35496,#35497,#35498,#35499,#35500,#35501,#35502,#35503,#35504,#35505,#35506,
#35507,#35508,#35509,#35510,#35511,#35512,#35513,#35514,#35515,#35516,#35517,
#35518,#35519,#35520,#35521,#35522,#35523,#35524,#35525,#35526,#35527,#35528,
#35529,#35530,#35531,#35532,#35533,#35534,#35535,#35536),(#35537,#35538,
#35539,#35540,#35541,#35542,#35543,#35544,#35545,#35546,#35547,#35548,#35549,
#35550,#35551,#35552,#35553,#35554,#35555,#35556,#35557,#35558,#35559,#35560,
#35561,#35562,#35563,#35564,#35565,#35566,#35567,#35568,#35569,#35570,#35571,
#35572,#35573,#35574,#35575,#35576,#35577,#35578,#35579,#35580,#35581,#35582,
#35583,#35584,#35585,#35586,#35587,#35588,#35589,#35590,#35591,#35592,#35593,
#35594,#35595,#35596,#35597,#35598,#35599,#35600,#35601,#35602,#35603,#35604),
(#35605,#35606,#35607,#35608,#35609,#35610,#35611,#35612,#35613,#35614,
#35615,#35616,#35617,#35618,#35619,#35620,#35621,#35622,#35623,#35624,#35625,
#35626,#35627,#35628,#35629,#35630,#35631,#35632,#35633,#35634,#35635,#35636,
#35637,#35638,#35639,#35640,#35641,#35642,#35643,#35644,#35645,#35646,#35647,
#35648,#35649,#35650,#35651,#35652,#35653,#35654,#35655,#35656,#35657,#35658,
#35659,#35660,#35661,#35662,#35663,#35664,#35665,#35666,#35667,#35668,#35669,
#35670,#35671,#35672),(#35673,#35674,#35675,#35676,#35677,#35678,#35679,
#35680,#35681,#35682,#35683,#35684,#35685,#35686,#35687,#35688,#35689,#35690,
#35691,#35692,#35693,#35694,#35695,#35696,#35697,#35698,#35699,#35700,#35701,
#35702,#35703,#35704,#35705,#35706,#35707,#35708,#35709,#35710,#35711,#35712,
#35713,#35714,#35715,#35716,#35717,#35718,#35719,#35720,#35721,#35722,#35723,
#35724,#35725,#35726,#35727,#35728,#35729,#35730,#35731,#35732,#35733,#35734,
#35735,#35736,#35737,#35738,#35739,#35740)),.UNSPECIFIED.,.F.,.F.,.F.,(4,
4),(4,1,1,1,1,1,1,1,1,1,1,1,1,1,1,1,1,1,1,1,1,1,1,1,1,1,1,1,1,1,1,1,1,1,
1,1,1,1,1,1,1,1,1,1,1,1,1,1,1,1,1,1,1,1,1,1,1,1,1,1,1,1,1,1,1,4),(0.,0.0321584099938616),
(14.3984001269718,15.3961297510265,16.3938593750811,17.3915889991358,18.3893186231905,
19.3870482472451,20.3847778712998,21.3825074953544,22.3802371194091,23.3779667434637,
24.3756963675184,25.3734259915731,26.3711556156277,27.3688852396824,28.366614863737,
29.3643444877917,30.3620741118463,31.359803735901,32.3575333599556,33.3552629840103,
34.352992608065,35.3507222321196,36.3484518561743,37.3461814802289,38.3439111042836,
39.3416407283382,40.3393703523929,41.3370999764475,42.3348296005022,43.3325592245569,
44.3302888486115,45.3280184726662,46.3257480967208,47.3234777207755,48.3212073448301,
49.3189369688848,50.3166665929395,51.3143962169941,52.3121258410488,53.3098554651034,
54.3075850891581,55.3053147132127,56.3030443372674,57.3007739613221,58.2985035853767,
59.2962332094314,60.293962833486,61.2916924575407,62.2894220815953,63.28715170565,
64.2848813297046,65.2826109537593,66.280340577814,67.2780702018686,68.2757998259233,
69.2735294499779,70.2712590740326,71.2689886980872,72.2667183221419,73.2644479461966,
74.2621775702512,75.2599071943059,76.2576368183605,77.2553664424152,78.2530960664698,
79.2508256905245),.UNSPECIFIED.);
#249=B_SPLINE_SURFACE_WITH_KNOTS('',3,3,((#35913,#35914,#35915,#35916,#35917,
#35918,#35919,#35920,#35921,#35922,#35923,#35924,#35925,#35926,#35927,#35928,
#35929,#35930,#35931,#35932,#35933,#35934,#35935,#35936,#35937,#35938,#35939,
#35940,#35941,#35942,#35943,#35944,#35945,#35946,#35947,#35948,#35949,#35950,
#35951,#35952,#35953),(#35954,#35955,#35956,#35957,#35958,#35959,#35960,
#35961,#35962,#35963,#35964,#35965,#35966,#35967,#35968,#35969,#35970,#35971,
#35972,#35973,#35974,#35975,#35976,#35977,#35978,#35979,#35980,#35981,#35982,
#35983,#35984,#35985,#35986,#35987,#35988,#35989,#35990,#35991,#35992,#35993,
#35994),(#35995,#35996,#35997,#35998,#35999,#36000,#36001,#36002,#36003,
#36004,#36005,#36006,#36007,#36008,#36009,#36010,#36011,#36012,#36013,#36014,
#36015,#36016,#36017,#36018,#36019,#36020,#36021,#36022,#36023,#36024,#36025,
#36026,#36027,#36028,#36029,#36030,#36031,#36032,#36033,#36034,#36035),
(#36036,#36037,#36038,#36039,#36040,#36041,#36042,#36043,#36044,#36045,
#36046,#36047,#36048,#36049,#36050,#36051,#36052,#36053,#36054,#36055,#36056,
#36057,#36058,#36059,#36060,#36061,#36062,#36063,#36064,#36065,#36066,#36067,
#36068,#36069,#36070,#36071,#36072,#36073,#36074,#36075,#36076),(#36077,
#36078,#36079,#36080,#36081,#36082,#36083,#36084,#36085,#36086,#36087,#36088,
#36089,#36090,#36091,#36092,#36093,#36094,#36095,#36096,#36097,#36098,#36099,
#36100,#36101,#36102,#36103,#36104,#36105,#36106,#36107,#36108,#36109,#36110,
#36111,#36112,#36113,#36114,#36115,#36116,#36117),(#36118,#36119,#36120,
#36121,#36122,#36123,#36124,#36125,#36126,#36127,#36128,#36129,#36130,#36131,
#36132,#36133,#36134,#36135,#36136,#36137,#36138,#36139,#36140,#36141,#36142,
#36143,#36144,#36145,#36146,#36147,#36148,#36149,#36150,#36151,#36152,#36153,
#36154,#36155,#36156,#36157,#36158),(#36159,#36160,#36161,#36162,#36163,
#36164,#36165,#36166,#36167,#36168,#36169,#36170,#36171,#36172,#36173,#36174,
#36175,#36176,#36177,#36178,#36179,#36180,#36181,#36182,#36183,#36184,#36185,
#36186,#36187,#36188,#36189,#36190,#36191,#36192,#36193,#36194,#36195,#36196,
#36197,#36198,#36199),(#36200,#36201,#36202,#36203,#36204,#36205,#36206,
#36207,#36208,#36209,#36210,#36211,#36212,#36213,#36214,#36215,#36216,#36217,
#36218,#36219,#36220,#36221,#36222,#36223,#36224,#36225,#36226,#36227,#36228,
#36229,#36230,#36231,#36232,#36233,#36234,#36235,#36236,#36237,#36238,#36239,
#36240),(#36241,#36242,#36243,#36244,#36245,#36246,#36247,#36248,#36249,
#36250,#36251,#36252,#36253,#36254,#36255,#36256,#36257,#36258,#36259,#36260,
#36261,#36262,#36263,#36264,#36265,#36266,#36267,#36268,#36269,#36270,#36271,
#36272,#36273,#36274,#36275,#36276,#36277,#36278,#36279,#36280,#36281),
(#36282,#36283,#36284,#36285,#36286,#36287,#36288,#36289,#36290,#36291,
#36292,#36293,#36294,#36295,#36296,#36297,#36298,#36299,#36300,#36301,#36302,
#36303,#36304,#36305,#36306,#36307,#36308,#36309,#36310,#36311,#36312,#36313,
#36314,#36315,#36316,#36317,#36318,#36319,#36320,#36321,#36322)),
 .UNSPECIFIED.,.T.,.F.,.F.,(4,1,1,1,1,1,1,4),(4,1,1,1,1,1,1,1,1,1,1,1,1,
1,1,1,1,1,1,1,1,1,1,1,1,1,1,1,1,1,1,1,1,1,1,1,1,1,4),(-3.14159265358979,
-2.24399475256414,-1.34639685153848,-0.448798950512828,0.448798950512828,
1.34639685153848,2.24399475256414,3.14159265358979),(0.,0.496040945303652,
0.992081890607303,1.48812283591095,1.98416378121461,2.48020472651826,2.97624567182191,
3.47228661712556,3.96832756242921,4.46436850773286,4.96040945303652,5.45645039834017,
5.95249134364382,6.44853228894747,6.94457323425112,7.44061417955477,7.93665512485842,
8.43269607016208,8.92873701546573,9.42477796076938,9.92081890607303,10.4168598513767,
10.9129007966803,11.408941741984,11.9049826872876,12.4010236325913,12.8970645778949,
13.3931055231986,13.8891464685022,14.3851874138059,14.8812283591095,15.3772693044132,
15.8733102497168,16.3693511950205,16.8653921403242,17.3614330856278,17.8574740309315,
18.3535149762351,18.8495559215388),.UNSPECIFIED.);
#250=B_SPLINE_SURFACE_WITH_KNOTS('',3,3,((#37705,#37706,#37707,#37708,#37709,
#37710,#37711,#37712,#37713,#37714,#37715,#37716,#37717,#37718,#37719,#37720,
#37721,#37722,#37723,#37724,#37725,#37726,#37727,#37728,#37729,#37730,#37731,
#37732,#37733,#37734,#37735,#37736,#37737,#37738,#37739,#37740,#37741,#37742,
#37743,#37744,#37745,#37746,#37747,#37748,#37749,#37750,#37751,#37752,#37753,
#37754,#37755,#37756,#37757,#37758,#37759,#37760,#37761,#37762,#37763,#37764,
#37765,#37766,#37767,#37768,#37769,#37770,#37771,#37772,#37773,#37774,#37775,
#37776,#37777,#37778,#37779,#37780,#37781,#37782,#37783,#37784,#37785,#37786,
#37787,#37788,#37789,#37790,#37791,#37792,#37793,#37794,#37795,#37796,#37797,
#37798,#37799,#37800,#37801,#37802,#37803,#37804,#37805,#37806,#37807,#37808,
#37809,#37810),(#37811,#37812,#37813,#37814,#37815,#37816,#37817,#37818,
#37819,#37820,#37821,#37822,#37823,#37824,#37825,#37826,#37827,#37828,#37829,
#37830,#37831,#37832,#37833,#37834,#37835,#37836,#37837,#37838,#37839,#37840,
#37841,#37842,#37843,#37844,#37845,#37846,#37847,#37848,#37849,#37850,#37851,
#37852,#37853,#37854,#37855,#37856,#37857,#37858,#37859,#37860,#37861,#37862,
#37863,#37864,#37865,#37866,#37867,#37868,#37869,#37870,#37871,#37872,#37873,
#37874,#37875,#37876,#37877,#37878,#37879,#37880,#37881,#37882,#37883,#37884,
#37885,#37886,#37887,#37888,#37889,#37890,#37891,#37892,#37893,#37894,#37895,
#37896,#37897,#37898,#37899,#37900,#37901,#37902,#37903,#37904,#37905,#37906,
#37907,#37908,#37909,#37910,#37911,#37912,#37913,#37914,#37915,#37916),
(#37917,#37918,#37919,#37920,#37921,#37922,#37923,#37924,#37925,#37926,
#37927,#37928,#37929,#37930,#37931,#37932,#37933,#37934,#37935,#37936,#37937,
#37938,#37939,#37940,#37941,#37942,#37943,#37944,#37945,#37946,#37947,#37948,
#37949,#37950,#37951,#37952,#37953,#37954,#37955,#37956,#37957,#37958,#37959,
#37960,#37961,#37962,#37963,#37964,#37965,#37966,#37967,#37968,#37969,#37970,
#37971,#37972,#37973,#37974,#37975,#37976,#37977,#37978,#37979,#37980,#37981,
#37982,#37983,#37984,#37985,#37986,#37987,#37988,#37989,#37990,#37991,#37992,
#37993,#37994,#37995,#37996,#37997,#37998,#37999,#38000,#38001,#38002,#38003,
#38004,#38005,#38006,#38007,#38008,#38009,#38010,#38011,#38012,#38013,#38014,
#38015,#38016,#38017,#38018,#38019,#38020,#38021,#38022),(#38023,#38024,
#38025,#38026,#38027,#38028,#38029,#38030,#38031,#38032,#38033,#38034,#38035,
#38036,#38037,#38038,#38039,#38040,#38041,#38042,#38043,#38044,#38045,#38046,
#38047,#38048,#38049,#38050,#38051,#38052,#38053,#38054,#38055,#38056,#38057,
#38058,#38059,#38060,#38061,#38062,#38063,#38064,#38065,#38066,#38067,#38068,
#38069,#38070,#38071,#38072,#38073,#38074,#38075,#38076,#38077,#38078,#38079,
#38080,#38081,#38082,#38083,#38084,#38085,#38086,#38087,#38088,#38089,#38090,
#38091,#38092,#38093,#38094,#38095,#38096,#38097,#38098,#38099,#38100,#38101,
#38102,#38103,#38104,#38105,#38106,#38107,#38108,#38109,#38110,#38111,#38112,
#38113,#38114,#38115,#38116,#38117,#38118,#38119,#38120,#38121,#38122,#38123,
#38124,#38125,#38126,#38127,#38128)),.UNSPECIFIED.,.F.,.F.,.F.,(4,4),(4,
1,1,1,1,1,1,1,1,1,1,1,1,1,1,1,1,1,1,1,1,1,1,1,1,1,1,1,1,1,1,1,1,1,1,1,1,
1,1,1,1,1,1,1,1,1,1,1,1,1,1,1,1,1,1,1,1,1,1,1,1,1,1,1,1,1,1,1,1,1,1,1,1,
1,1,1,1,1,1,1,1,1,1,1,1,1,1,1,1,1,1,1,1,1,1,1,1,1,1,1,1,1,1,4),(0.,0.0460148164544132),
(11.6154215191105,12.6127573616628,13.610093204215,14.6074290467673,15.6047648893195,
16.6021007318718,17.599436574424,18.5967724169762,19.5941082595285,20.5914441020807,
21.588779944633,22.5861157871852,23.5834516297375,24.5807874722897,25.5781233148419,
26.5754591573942,27.5727949999464,28.5701308424987,29.5674666850509,30.5648025276032,
31.5621383701554,32.5594742127077,33.5568100552599,34.5541458978121,35.5514817403644,
36.5488175829166,37.5461534254689,38.5434892680211,39.5408251105734,40.5381609531256,
41.5354967956779,42.5328326382301,43.5301684807823,44.5275043233346,45.5248401658868,
46.5221760084391,47.5195118509913,48.5168476935436,49.5141835360958,50.5115193786481,
51.5088552212003,52.5061910637525,53.5035269063048,54.500862748857,55.4981985914093,
56.4955344339615,57.4928702765138,58.490206119066,59.4875419616182,60.4848778041705,
61.4822136467227,62.479549489275,63.4768853318272,64.4742211743795,65.4715570169317,
66.468892859484,67.4662287020362,68.4635645445884,69.4609003871407,70.4582362296929,
71.4555720722452,72.4529079147974,73.4502437573497,74.4475795999019,75.4449154424541,
76.4422512850064,77.4395871275586,78.4369229701109,79.4342588126631,80.4315946552154,
81.4289304977676,82.4262663403199,83.4236021828721,84.4209380254243,85.4182738679766,
86.4156097105288,87.4129455530811,88.4102813956333,89.4076172381856,90.4049530807378,
91.4022889232901,92.3996247658423,93.3969606083945,94.3942964509468,95.391632293499,
96.3889681360513,97.3863039786035,98.3836398211558,99.380975663708,100.37831150626,
101.375647348812,102.372983191365,103.370319033917,104.367654876469,105.364990719021,
106.362326561574,107.359662404126,108.356998246678,109.35433408923,110.351669931783,
111.349005774335,112.346341616887,113.343677459439,114.341013301992),
 .UNSPECIFIED.);
#251=B_SPLINE_SURFACE_WITH_KNOTS('',3,3,((#38221,#38222,#38223,#38224,#38225,
#38226,#38227,#38228,#38229,#38230,#38231,#38232,#38233,#38234,#38235,#38236,
#38237,#38238,#38239,#38240,#38241,#38242,#38243,#38244,#38245,#38246,#38247,
#38248,#38249,#38250,#38251,#38252,#38253,#38254,#38255,#38256,#38257,#38258,
#38259,#38260,#38261,#38262,#38263,#38264,#38265,#38266,#38267,#38268,#38269,
#38270,#38271,#38272,#38273,#38274,#38275,#38276,#38277,#38278,#38279,#38280,
#38281,#38282,#38283,#38284,#38285,#38286,#38287,#38288,#38289,#38290,#38291,
#38292,#38293,#38294,#38295,#38296,#38297,#38298,#38299,#38300,#38301,#38302,
#38303,#38304,#38305,#38306,#38307,#38308,#38309,#38310,#38311,#38312,#38313,
#38314,#38315,#38316,#38317,#38318,#38319,#38320,#38321,#38322,#38323,#38324,
#38325,#38326,#38327,#38328),(#38329,#38330,#38331,#38332,#38333,#38334,
#38335,#38336,#38337,#38338,#38339,#38340,#38341,#38342,#38343,#38344,#38345,
#38346,#38347,#38348,#38349,#38350,#38351,#38352,#38353,#38354,#38355,#38356,
#38357,#38358,#38359,#38360,#38361,#38362,#38363,#38364,#38365,#38366,#38367,
#38368,#38369,#38370,#38371,#38372,#38373,#38374,#38375,#38376,#38377,#38378,
#38379,#38380,#38381,#38382,#38383,#38384,#38385,#38386,#38387,#38388,#38389,
#38390,#38391,#38392,#38393,#38394,#38395,#38396,#38397,#38398,#38399,#38400,
#38401,#38402,#38403,#38404,#38405,#38406,#38407,#38408,#38409,#38410,#38411,
#38412,#38413,#38414,#38415,#38416,#38417,#38418,#38419,#38420,#38421,#38422,
#38423,#38424,#38425,#38426,#38427,#38428,#38429,#38430,#38431,#38432,#38433,
#38434,#38435,#38436),(#38437,#38438,#38439,#38440,#38441,#38442,#38443,
#38444,#38445,#38446,#38447,#38448,#38449,#38450,#38451,#38452,#38453,#38454,
#38455,#38456,#38457,#38458,#38459,#38460,#38461,#38462,#38463,#38464,#38465,
#38466,#38467,#38468,#38469,#38470,#38471,#38472,#38473,#38474,#38475,#38476,
#38477,#38478,#38479,#38480,#38481,#38482,#38483,#38484,#38485,#38486,#38487,
#38488,#38489,#38490,#38491,#38492,#38493,#38494,#38495,#38496,#38497,#38498,
#38499,#38500,#38501,#38502,#38503,#38504,#38505,#38506,#38507,#38508,#38509,
#38510,#38511,#38512,#38513,#38514,#38515,#38516,#38517,#38518,#38519,#38520,
#38521,#38522,#38523,#38524,#38525,#38526,#38527,#38528,#38529,#38530,#38531,
#38532,#38533,#38534,#38535,#38536,#38537,#38538,#38539,#38540,#38541,#38542,
#38543,#38544),(#38545,#38546,#38547,#38548,#38549,#38550,#38551,#38552,
#38553,#38554,#38555,#38556,#38557,#38558,#38559,#38560,#38561,#38562,#38563,
#38564,#38565,#38566,#38567,#38568,#38569,#38570,#38571,#38572,#38573,#38574,
#38575,#38576,#38577,#38578,#38579,#38580,#38581,#38582,#38583,#38584,#38585,
#38586,#38587,#38588,#38589,#38590,#38591,#38592,#38593,#38594,#38595,#38596,
#38597,#38598,#38599,#38600,#38601,#38602,#38603,#38604,#38605,#38606,#38607,
#38608,#38609,#38610,#38611,#38612,#38613,#38614,#38615,#38616,#38617,#38618,
#38619,#38620,#38621,#38622,#38623,#38624,#38625,#38626,#38627,#38628,#38629,
#38630,#38631,#38632,#38633,#38634,#38635,#38636,#38637,#38638,#38639,#38640,
#38641,#38642,#38643,#38644,#38645,#38646,#38647,#38648,#38649,#38650,#38651,
#38652)),.UNSPECIFIED.,.F.,.F.,.F.,(4,4),(4,1,1,1,1,1,1,1,1,1,1,1,1,1,1,
1,1,1,1,1,1,1,1,1,1,1,1,1,1,1,1,1,1,1,1,1,1,1,1,1,1,1,1,1,1,1,1,1,1,1,1,
1,1,1,1,1,1,1,1,1,1,1,1,1,1,1,1,1,1,1,1,1,1,1,1,1,1,1,1,1,1,1,1,1,1,1,1,
1,1,1,1,1,1,1,1,1,1,1,1,1,1,1,1,1,1,4),(0.,0.0460148164544132),(8.31058692273969,
9.30859389336977,10.3066008639999,11.30460783463,12.30261480526,13.3006217758901,
14.2986287465202,15.2966357171503,16.2946426877804,17.2926496584105,18.2906566290406,
19.2886635996707,20.2866705703008,21.2846775409308,22.2826845115609,23.280691482191,
24.2786984528211,25.2767054234512,26.2747123940813,27.2727193647114,28.2707263353415,
29.2687333059716,30.2667402766016,31.2647472472317,32.2627542178618,33.2607611884919,
34.258768159122,35.2567751297521,36.2547821003822,37.2527890710123,38.2507960416424,
39.2488030122724,40.2468099829025,41.2448169535326,42.2428239241627,43.2408308947928,
44.2388378654229,45.236844836053,46.2348518066831,47.2328587773132,48.2308657479432,
49.2288727185733,50.2268796892034,51.2248866598335,52.2228936304636,53.2209006010937,
54.2189075717238,55.2169145423539,56.214921512984,57.212928483614,58.2109354542441,
59.2089424248742,60.2069493955043,61.2049563661344,62.2029633367645,63.2009703073946,
64.1989772780247,65.1969842486548,66.1949912192848,67.1929981899149,68.191005160545,
69.1890121311751,70.1870191018052,71.1850260724353,72.1830330430654,73.1810400136955,
74.1790469843256,75.1770539549557,76.1750609255857,77.1730678962158,78.1710748668459,
79.169081837476,80.1670888081061,81.1650957787362,82.1631027493663,83.1611097199964,
84.1591166906264,85.1571236612565,86.1551306318866,87.1531376025167,88.1511445731468,
89.1491515437769,90.147158514407,91.1451654850371,92.1431724556672,93.1411794262973,
94.1391863969273,95.1371933675574,96.1352003381875,97.1332073088176,98.1312142794477,
99.1292212500778,100.127228220708,101.125235191338,102.123242161968,103.121249132598,
104.119256103228,105.117263073858,106.115270044488,107.113277015118,108.111283985749,
109.109290956379,110.107297927009,111.105304897639,112.103311868269,113.101318838899),
 .UNSPECIFIED.);
#252=B_SPLINE_SURFACE_WITH_KNOTS('',3,3,((#39668,#39669,#39670,#39671,#39672,
#39673,#39674,#39675,#39676,#39677,#39678,#39679,#39680,#39681,#39682,#39683,
#39684,#39685,#39686,#39687,#39688,#39689,#39690,#39691,#39692,#39693,#39694,
#39695,#39696,#39697,#39698,#39699,#39700,#39701,#39702,#39703,#39704,#39705,
#39706,#39707,#39708,#39709,#39710,#39711,#39712,#39713,#39714,#39715,#39716,
#39717,#39718,#39719,#39720,#39721,#39722,#39723,#39724,#39725,#39726,#39727,
#39728,#39729,#39730,#39731,#39732,#39733,#39734,#39735,#39736,#39737),
(#39738,#39739,#39740,#39741,#39742,#39743,#39744,#39745,#39746,#39747,
#39748,#39749,#39750,#39751,#39752,#39753,#39754,#39755,#39756,#39757,#39758,
#39759,#39760,#39761,#39762,#39763,#39764,#39765,#39766,#39767,#39768,#39769,
#39770,#39771,#39772,#39773,#39774,#39775,#39776,#39777,#39778,#39779,#39780,
#39781,#39782,#39783,#39784,#39785,#39786,#39787,#39788,#39789,#39790,#39791,
#39792,#39793,#39794,#39795,#39796,#39797,#39798,#39799,#39800,#39801,#39802,
#39803,#39804,#39805,#39806,#39807),(#39808,#39809,#39810,#39811,#39812,
#39813,#39814,#39815,#39816,#39817,#39818,#39819,#39820,#39821,#39822,#39823,
#39824,#39825,#39826,#39827,#39828,#39829,#39830,#39831,#39832,#39833,#39834,
#39835,#39836,#39837,#39838,#39839,#39840,#39841,#39842,#39843,#39844,#39845,
#39846,#39847,#39848,#39849,#39850,#39851,#39852,#39853,#39854,#39855,#39856,
#39857,#39858,#39859,#39860,#39861,#39862,#39863,#39864,#39865,#39866,#39867,
#39868,#39869,#39870,#39871,#39872,#39873,#39874,#39875,#39876,#39877),
(#39878,#39879,#39880,#39881,#39882,#39883,#39884,#39885,#39886,#39887,
#39888,#39889,#39890,#39891,#39892,#39893,#39894,#39895,#39896,#39897,#39898,
#39899,#39900,#39901,#39902,#39903,#39904,#39905,#39906,#39907,#39908,#39909,
#39910,#39911,#39912,#39913,#39914,#39915,#39916,#39917,#39918,#39919,#39920,
#39921,#39922,#39923,#39924,#39925,#39926,#39927,#39928,#39929,#39930,#39931,
#39932,#39933,#39934,#39935,#39936,#39937,#39938,#39939,#39940,#39941,#39942,
#39943,#39944,#39945,#39946,#39947)),.UNSPECIFIED.,.F.,.F.,.F.,(4,4),(4,
1,1,1,1,1,1,1,1,1,1,1,1,1,1,1,1,1,1,1,1,1,1,1,1,1,1,1,1,1,1,1,1,1,1,1,1,
1,1,1,1,1,1,1,1,1,1,1,1,1,1,1,1,1,1,1,1,1,1,1,1,1,1,1,1,1,1,4),(0.,0.0329955678841871),
(11.6159397475004,12.6141690908179,13.6123984341354,14.6106277774529,15.6088571207704,
16.6070864640879,17.6053158074054,18.6035451507229,19.6017744940404,20.600003837358,
21.5982331806755,22.596462523993,23.5946918673105,24.592921210628,25.5911505539455,
26.589379897263,27.5876092405805,28.585838583898,29.5840679272155,30.5822972705331,
31.5805266138506,32.5787559571681,33.5769853004856,34.5752146438031,35.5734439871206,
36.5716733304381,37.5699026737556,38.5681320170731,39.5663613603907,40.5645907037082,
41.5628200470257,42.5610493903432,43.5592787336607,44.5575080769782,45.5557374202957,
46.5539667636132,47.5521961069307,48.5504254502482,49.5486547935658,50.5468841368833,
51.5451134802008,52.5433428235183,53.5415721668358,54.5398015101533,55.5380308534708,
56.5362601967883,57.5344895401058,58.5327188834233,59.5309482267409,60.5291775700584,
61.5274069133759,62.5256362566934,63.5238656000109,64.5220949433284,65.5203242866459,
66.5185536299634,67.5167829732809,68.5150123165984,69.513241659916,70.5114710032335,
71.509700346551,72.5079296898685,73.506159033186,74.5043883765035,75.502617719821,
76.5008470631385,77.499076406456,78.4973057497735),.UNSPECIFIED.);
#253=B_SPLINE_SURFACE_WITH_KNOTS('',3,3,((#40037,#40038,#40039,#40040,#40041,
#40042,#40043,#40044,#40045,#40046,#40047,#40048,#40049,#40050,#40051,#40052,
#40053,#40054,#40055,#40056,#40057,#40058,#40059,#40060,#40061,#40062,#40063,
#40064,#40065,#40066,#40067,#40068,#40069,#40070,#40071,#40072,#40073,#40074,
#40075,#40076,#40077,#40078,#40079,#40080,#40081,#40082,#40083,#40084,#40085,
#40086,#40087,#40088,#40089,#40090,#40091,#40092,#40093,#40094,#40095,#40096,
#40097,#40098,#40099,#40100,#40101,#40102,#40103,#40104,#40105,#40106,#40107,
#40108),(#40109,#40110,#40111,#40112,#40113,#40114,#40115,#40116,#40117,
#40118,#40119,#40120,#40121,#40122,#40123,#40124,#40125,#40126,#40127,#40128,
#40129,#40130,#40131,#40132,#40133,#40134,#40135,#40136,#40137,#40138,#40139,
#40140,#40141,#40142,#40143,#40144,#40145,#40146,#40147,#40148,#40149,#40150,
#40151,#40152,#40153,#40154,#40155,#40156,#40157,#40158,#40159,#40160,#40161,
#40162,#40163,#40164,#40165,#40166,#40167,#40168,#40169,#40170,#40171,#40172,
#40173,#40174,#40175,#40176,#40177,#40178,#40179,#40180),(#40181,#40182,
#40183,#40184,#40185,#40186,#40187,#40188,#40189,#40190,#40191,#40192,#40193,
#40194,#40195,#40196,#40197,#40198,#40199,#40200,#40201,#40202,#40203,#40204,
#40205,#40206,#40207,#40208,#40209,#40210,#40211,#40212,#40213,#40214,#40215,
#40216,#40217,#40218,#40219,#40220,#40221,#40222,#40223,#40224,#40225,#40226,
#40227,#40228,#40229,#40230,#40231,#40232,#40233,#40234,#40235,#40236,#40237,
#40238,#40239,#40240,#40241,#40242,#40243,#40244,#40245,#40246,#40247,#40248,
#40249,#40250,#40251,#40252),(#40253,#40254,#40255,#40256,#40257,#40258,
#40259,#40260,#40261,#40262,#40263,#40264,#40265,#40266,#40267,#40268,#40269,
#40270,#40271,#40272,#40273,#40274,#40275,#40276,#40277,#40278,#40279,#40280,
#40281,#40282,#40283,#40284,#40285,#40286,#40287,#40288,#40289,#40290,#40291,
#40292,#40293,#40294,#40295,#40296,#40297,#40298,#40299,#40300,#40301,#40302,
#40303,#40304,#40305,#40306,#40307,#40308,#40309,#40310,#40311,#40312,#40313,
#40314,#40315,#40316,#40317,#40318,#40319,#40320,#40321,#40322,#40323,#40324)),
 .UNSPECIFIED.,.F.,.F.,.F.,(4,4),(4,1,1,1,1,1,1,1,1,1,1,1,1,1,1,1,1,1,1,
1,1,1,1,1,1,1,1,1,1,1,1,1,1,1,1,1,1,1,1,1,1,1,1,1,1,1,1,1,1,1,1,1,1,1,1,
1,1,1,1,1,1,1,1,1,1,1,1,1,1,4),(0.,0.0329955678841871),(8.30203615430834,
9.30137729453432,10.3007184347603,11.3000595749863,12.2994007152123,13.2987418554383,
14.2980829956642,15.2974241358902,16.2967652761162,17.2961064163422,18.2954475565682,
19.2947886967942,20.2941298370201,21.2934709772461,22.2928121174721,23.2921532576981,
24.2914943979241,25.2908355381501,26.290176678376,27.289517818602,28.288858958828,
29.288200099054,30.28754123928,31.286882379506,32.2862235197319,33.2855646599579,
34.2849058001839,35.2842469404099,36.2835880806359,37.2829292208619,38.2822703610879,
39.2816115013138,40.2809526415398,41.2802937817658,42.2796349219918,43.2789760622178,
44.2783172024438,45.2776583426697,46.2769994828957,47.2763406231217,48.2756817633477,
49.2750229035737,50.2743640437997,51.2737051840256,52.2730463242516,53.2723874644776,
54.2717286047036,55.2710697449296,56.2704108851556,57.2697520253815,58.2690931656075,
59.2684343058335,60.2677754460595,61.2671165862855,62.2664577265115,63.2657988667374,
64.2651400069634,65.2644811471894,66.2638222874154,67.2631634276414,68.2625045678674,
69.2618457080933,70.2611868483193,71.2605279885453,72.2598691287713,73.2592102689973,
74.2585514092233,75.2578925494492,76.2572336896752,77.2565748299012),
 .UNSPECIFIED.);
#254=B_SPLINE_SURFACE_WITH_KNOTS('',3,3,((#41937,#41938,#41939,#41940,#41941,
#41942,#41943,#41944,#41945,#41946,#41947,#41948,#41949,#41950,#41951,#41952,
#41953,#41954,#41955,#41956,#41957,#41958,#41959,#41960,#41961,#41962,#41963,
#41964,#41965,#41966,#41967,#41968,#41969,#41970,#41971,#41972,#41973,#41974,
#41975,#41976,#41977,#41978,#41979,#41980,#41981,#41982,#41983,#41984,#41985,
#41986,#41987,#41988,#41989,#41990,#41991,#41992,#41993,#41994,#41995,#41996,
#41997,#41998,#41999,#42000,#42001,#42002,#42003,#42004,#42005,#42006,#42007,
#42008,#42009,#42010,#42011,#42012,#42013,#42014,#42015,#42016,#42017,#42018,
#42019,#42020,#42021,#42022,#42023,#42024,#42025,#42026,#42027,#42028,#42029,
#42030,#42031,#42032,#42033,#42034,#42035,#42036,#42037,#42038,#42039,#42040,
#42041,#42042,#42043,#42044,#42045,#42046,#42047,#42048,#42049,#42050,#42051,
#42052,#42053,#42054,#42055,#42056,#42057),(#42058,#42059,#42060,#42061,
#42062,#42063,#42064,#42065,#42066,#42067,#42068,#42069,#42070,#42071,#42072,
#42073,#42074,#42075,#42076,#42077,#42078,#42079,#42080,#42081,#42082,#42083,
#42084,#42085,#42086,#42087,#42088,#42089,#42090,#42091,#42092,#42093,#42094,
#42095,#42096,#42097,#42098,#42099,#42100,#42101,#42102,#42103,#42104,#42105,
#42106,#42107,#42108,#42109,#42110,#42111,#42112,#42113,#42114,#42115,#42116,
#42117,#42118,#42119,#42120,#42121,#42122,#42123,#42124,#42125,#42126,#42127,
#42128,#42129,#42130,#42131,#42132,#42133,#42134,#42135,#42136,#42137,#42138,
#42139,#42140,#42141,#42142,#42143,#42144,#42145,#42146,#42147,#42148,#42149,
#42150,#42151,#42152,#42153,#42154,#42155,#42156,#42157,#42158,#42159,#42160,
#42161,#42162,#42163,#42164,#42165,#42166,#42167,#42168,#42169,#42170,#42171,
#42172,#42173,#42174,#42175,#42176,#42177,#42178),(#42179,#42180,#42181,
#42182,#42183,#42184,#42185,#42186,#42187,#42188,#42189,#42190,#42191,#42192,
#42193,#42194,#42195,#42196,#42197,#42198,#42199,#42200,#42201,#42202,#42203,
#42204,#42205,#42206,#42207,#42208,#42209,#42210,#42211,#42212,#42213,#42214,
#42215,#42216,#42217,#42218,#42219,#42220,#42221,#42222,#42223,#42224,#42225,
#42226,#42227,#42228,#42229,#42230,#42231,#42232,#42233,#42234,#42235,#42236,
#42237,#42238,#42239,#42240,#42241,#42242,#42243,#42244,#42245,#42246,#42247,
#42248,#42249,#42250,#42251,#42252,#42253,#42254,#42255,#42256,#42257,#42258,
#42259,#42260,#42261,#42262,#42263,#42264,#42265,#42266,#42267,#42268,#42269,
#42270,#42271,#42272,#42273,#42274,#42275,#42276,#42277,#42278,#42279,#42280,
#42281,#42282,#42283,#42284,#42285,#42286,#42287,#42288,#42289,#42290,#42291,
#42292,#42293,#42294,#42295,#42296,#42297,#42298,#42299),(#42300,#42301,
#42302,#42303,#42304,#42305,#42306,#42307,#42308,#42309,#42310,#42311,#42312,
#42313,#42314,#42315,#42316,#42317,#42318,#42319,#42320,#42321,#42322,#42323,
#42324,#42325,#42326,#42327,#42328,#42329,#42330,#42331,#42332,#42333,#42334,
#42335,#42336,#42337,#42338,#42339,#42340,#42341,#42342,#42343,#42344,#42345,
#42346,#42347,#42348,#42349,#42350,#42351,#42352,#42353,#42354,#42355,#42356,
#42357,#42358,#42359,#42360,#42361,#42362,#42363,#42364,#42365,#42366,#42367,
#42368,#42369,#42370,#42371,#42372,#42373,#42374,#42375,#42376,#42377,#42378,
#42379,#42380,#42381,#42382,#42383,#42384,#42385,#42386,#42387,#42388,#42389,
#42390,#42391,#42392,#42393,#42394,#42395,#42396,#42397,#42398,#42399,#42400,
#42401,#42402,#42403,#42404,#42405,#42406,#42407,#42408,#42409,#42410,#42411,
#42412,#42413,#42414,#42415,#42416,#42417,#42418,#42419,#42420)),
 .UNSPECIFIED.,.F.,.F.,.F.,(4,4),(4,1,1,1,1,1,1,1,1,1,1,1,1,1,1,1,1,1,1,
1,1,1,1,1,1,1,1,1,1,1,1,1,1,1,1,1,1,1,1,1,1,1,1,1,1,1,1,1,1,1,1,1,1,1,1,
1,1,1,1,1,1,1,1,1,1,1,1,1,1,1,1,1,1,1,1,1,1,1,1,1,1,1,1,1,1,1,1,1,1,1,1,
1,1,1,1,1,1,1,1,1,1,1,1,1,1,1,1,1,1,1,1,1,1,1,1,1,1,1,4),(0.,0.0329955678841871),
(11.6159397475003,12.6087096497013,13.6014795519022,14.5942494541031,15.5870193563041,
16.579789258505,17.5725591607059,18.5653290629068,19.5580989651078,20.5508688673087,
21.5436387695096,22.5364086717106,23.5291785739115,24.5219484761124,25.5147183783134,
26.5074882805143,27.5002581827152,28.4930280849161,29.4857979871171,30.478567889318,
31.4713377915189,32.4641076937199,33.4568775959208,34.4496474981217,35.4424174003227,
36.4351873025236,37.4279572047245,38.4207271069255,39.4134970091264,40.4062669113273,
41.3990368135282,42.3918067157292,43.3845766179301,44.377346520131,45.370116422332,
46.3628863245329,47.3556562267338,48.3484261289348,49.3411960311357,50.3339659333366,
51.3267358355376,52.3195057377385,53.3122756399394,54.3050455421403,55.2978154443413,
56.2905853465422,57.2833552487431,58.2761251509441,59.268895053145,60.2616649553459,
61.2544348575469,62.2472047597478,63.2399746619487,64.2327445641497,65.2255144663506,
66.2182843685515,67.2110542707524,68.2038241729534,69.1965940751543,70.1893639773552,
71.1821338795562,72.1749037817571,73.167673683958,74.160443586159,75.1532134883599,
76.1459833905608,77.1387532927618,78.1315231949627,79.1242930971636,80.1170629993645,
81.1098329015655,82.1026028037664,83.0953727059673,84.0881426081683,85.0809125103692,
86.0736824125701,87.0664523147711,88.059222216972,89.0519921191729,90.0447620213739,
91.0375319235748,92.0303018257757,93.0230717279766,94.0158416301776,95.0086115323785,
96.0013814345794,96.9941513367804,97.9869212389813,98.9796911411822,99.9724610433832,
100.965230945584,101.958000847785,102.950770749986,103.943540652187,104.936310554388,
105.929080456589,106.92185035879,107.914620260991,108.907390163192,109.900160065392,
110.892929967593,111.885699869794,112.878469771995,113.871239674196,114.864009576397,
115.856779478598,116.849549380799,117.842319283,118.835089185201,119.827859087402,
120.820628989603,121.813398891804,122.806168794005,123.798938696205,124.791708598406,
125.784478500607,126.777248402808,127.770018305009,128.76278820721),
 .UNSPECIFIED.);
#255=B_SPLINE_SURFACE_WITH_KNOTS('',3,3,((#42516,#42517,#42518,#42519,#42520,
#42521,#42522,#42523,#42524,#42525,#42526,#42527,#42528,#42529,#42530,#42531,
#42532,#42533,#42534,#42535,#42536,#42537,#42538,#42539,#42540,#42541,#42542,
#42543,#42544,#42545,#42546,#42547,#42548,#42549,#42550,#42551,#42552,#42553,
#42554,#42555,#42556,#42557,#42558,#42559,#42560,#42561,#42562,#42563,#42564,
#42565,#42566,#42567,#42568,#42569,#42570,#42571,#42572,#42573,#42574,#42575,
#42576,#42577,#42578,#42579,#42580,#42581,#42582,#42583,#42584,#42585,#42586,
#42587,#42588,#42589,#42590,#42591,#42592,#42593,#42594,#42595,#42596,#42597,
#42598,#42599,#42600,#42601,#42602,#42603,#42604,#42605,#42606,#42607,#42608,
#42609,#42610,#42611,#42612,#42613,#42614,#42615,#42616,#42617,#42618,#42619,
#42620,#42621,#42622,#42623,#42624,#42625,#42626,#42627,#42628,#42629,#42630,
#42631,#42632,#42633,#42634,#42635,#42636,#42637,#42638),(#42639,#42640,
#42641,#42642,#42643,#42644,#42645,#42646,#42647,#42648,#42649,#42650,#42651,
#42652,#42653,#42654,#42655,#42656,#42657,#42658,#42659,#42660,#42661,#42662,
#42663,#42664,#42665,#42666,#42667,#42668,#42669,#42670,#42671,#42672,#42673,
#42674,#42675,#42676,#42677,#42678,#42679,#42680,#42681,#42682,#42683,#42684,
#42685,#42686,#42687,#42688,#42689,#42690,#42691,#42692,#42693,#42694,#42695,
#42696,#42697,#42698,#42699,#42700,#42701,#42702,#42703,#42704,#42705,#42706,
#42707,#42708,#42709,#42710,#42711,#42712,#42713,#42714,#42715,#42716,#42717,
#42718,#42719,#42720,#42721,#42722,#42723,#42724,#42725,#42726,#42727,#42728,
#42729,#42730,#42731,#42732,#42733,#42734,#42735,#42736,#42737,#42738,#42739,
#42740,#42741,#42742,#42743,#42744,#42745,#42746,#42747,#42748,#42749,#42750,
#42751,#42752,#42753,#42754,#42755,#42756,#42757,#42758,#42759,#42760,#42761),
(#42762,#42763,#42764,#42765,#42766,#42767,#42768,#42769,#42770,#42771,
#42772,#42773,#42774,#42775,#42776,#42777,#42778,#42779,#42780,#42781,#42782,
#42783,#42784,#42785,#42786,#42787,#42788,#42789,#42790,#42791,#42792,#42793,
#42794,#42795,#42796,#42797,#42798,#42799,#42800,#42801,#42802,#42803,#42804,
#42805,#42806,#42807,#42808,#42809,#42810,#42811,#42812,#42813,#42814,#42815,
#42816,#42817,#42818,#42819,#42820,#42821,#42822,#42823,#42824,#42825,#42826,
#42827,#42828,#42829,#42830,#42831,#42832,#42833,#42834,#42835,#42836,#42837,
#42838,#42839,#42840,#42841,#42842,#42843,#42844,#42845,#42846,#42847,#42848,
#42849,#42850,#42851,#42852,#42853,#42854,#42855,#42856,#42857,#42858,#42859,
#42860,#42861,#42862,#42863,#42864,#42865,#42866,#42867,#42868,#42869,#42870,
#42871,#42872,#42873,#42874,#42875,#42876,#42877,#42878,#42879,#42880,#42881,
#42882,#42883,#42884),(#42885,#42886,#42887,#42888,#42889,#42890,#42891,
#42892,#42893,#42894,#42895,#42896,#42897,#42898,#42899,#42900,#42901,#42902,
#42903,#42904,#42905,#42906,#42907,#42908,#42909,#42910,#42911,#42912,#42913,
#42914,#42915,#42916,#42917,#42918,#42919,#42920,#42921,#42922,#42923,#42924,
#42925,#42926,#42927,#42928,#42929,#42930,#42931,#42932,#42933,#42934,#42935,
#42936,#42937,#42938,#42939,#42940,#42941,#42942,#42943,#42944,#42945,#42946,
#42947,#42948,#42949,#42950,#42951,#42952,#42953,#42954,#42955,#42956,#42957,
#42958,#42959,#42960,#42961,#42962,#42963,#42964,#42965,#42966,#42967,#42968,
#42969,#42970,#42971,#42972,#42973,#42974,#42975,#42976,#42977,#42978,#42979,
#42980,#42981,#42982,#42983,#42984,#42985,#42986,#42987,#42988,#42989,#42990,
#42991,#42992,#42993,#42994,#42995,#42996,#42997,#42998,#42999,#43000,#43001,
#43002,#43003,#43004,#43005,#43006,#43007)),.UNSPECIFIED.,.F.,.F.,.F.,(4,
4),(4,1,1,1,1,1,1,1,1,1,1,1,1,1,1,1,1,1,1,1,1,1,1,1,1,1,1,1,1,1,1,1,1,1,
1,1,1,1,1,1,1,1,1,1,1,1,1,1,1,1,1,1,1,1,1,1,1,1,1,1,1,1,1,1,1,1,1,1,1,1,
1,1,1,1,1,1,1,1,1,1,1,1,1,1,1,1,1,1,1,1,1,1,1,1,1,1,1,1,1,1,1,1,1,1,1,1,
1,1,1,1,1,1,1,1,1,1,1,1,1,1,4),(0.,0.0329955678841871),(8.30203615430831,
9.29553633041689,10.2890365065255,11.282536682634,12.2760368587426,13.2695370348512,
14.2630372109598,15.2565373870684,16.2500375631769,17.2435377392855,18.2370379153941,
19.2305380915027,20.2240382676113,21.2175384437198,22.2110386198284,23.204538795937,
24.1980389720456,25.1915391481542,26.1850393242627,27.1785395003713,28.1720396764799,
29.1655398525885,30.1590400286971,31.1525402048056,32.1460403809142,33.1395405570228,
34.1330407331314,35.1265409092399,36.1200410853485,37.1135412614571,38.1070414375657,
39.1005416136743,40.0940417897828,41.0875419658914,42.081042142,43.0745423181086,
44.0680424942172,45.0615426703257,46.0550428464343,47.0485430225429,48.0420431986515,
49.0355433747601,50.0290435508686,51.0225437269772,52.0160439030858,53.0095440791944,
54.003044255303,54.9965444314115,55.9900446075201,56.9835447836287,57.9770449597373,
58.9705451358458,59.9640453119544,60.957545488063,61.9510456641716,62.9445458402802,
63.9380460163887,64.9315461924973,65.9250463686059,66.9185465447145,67.9120467208231,
68.9055468969316,69.8990470730402,70.8925472491488,71.8860474252574,72.879547601366,
73.8730477774745,74.8665479535831,75.8600481296917,76.8535483058003,77.8470484819088,
78.8405486580174,79.834048834126,80.8275490102346,81.8210491863432,82.8145493624517,
83.8080495385603,84.8015497146689,85.7950498907775,86.7885500668861,87.7820502429946,
88.7755504191032,89.7690505952118,90.7625507713204,91.756050947429,92.7495511235375,
93.7430512996461,94.7365514757547,95.7300516518633,96.7235518279718,97.7170520040804,
98.710552180189,99.7040523562976,100.697552532406,101.691052708515,102.684552884623,
103.678053060732,104.67155323684,105.665053412949,106.658553589058,107.652053765166,
108.645553941275,109.639054117383,110.632554293492,111.626054469601,112.619554645709,
113.613054821818,114.606554997926,115.600055174035,116.593555350143,117.587055526252,
118.580555702361,119.574055878469,120.567556054578,121.561056230686,122.554556406795,
123.548056582903,124.541556759012,125.535056935121,126.528557111229,127.522057287338),
 .UNSPECIFIED.);
#256=B_SPLINE_SURFACE_WITH_KNOTS('',3,3,((#43487,#43488,#43489,#43490,#43491,
#43492,#43493,#43494,#43495,#43496,#43497,#43498,#43499,#43500,#43501,#43502,
#43503,#43504,#43505,#43506,#43507,#43508),(#43509,#43510,#43511,#43512,
#43513,#43514,#43515,#43516,#43517,#43518,#43519,#43520,#43521,#43522,#43523,
#43524,#43525,#43526,#43527,#43528,#43529,#43530),(#43531,#43532,#43533,
#43534,#43535,#43536,#43537,#43538,#43539,#43540,#43541,#43542,#43543,#43544,
#43545,#43546,#43547,#43548,#43549,#43550,#43551,#43552),(#43553,#43554,
#43555,#43556,#43557,#43558,#43559,#43560,#43561,#43562,#43563,#43564,#43565,
#43566,#43567,#43568,#43569,#43570,#43571,#43572,#43573,#43574)),
 .UNSPECIFIED.,.F.,.F.,.F.,(4,4),(4,1,1,1,1,1,1,1,1,1,1,1,1,1,1,1,1,1,1,
4),(0.,0.098669161004507),(11.6147305479243,12.0988438158569,12.5829570837895,
13.5511836196547,14.5194101555198,15.487636691385,16.4558632272502,17.4240897631154,
18.3923162989806,19.3605428348458,20.3287693707109,21.2969959065761,22.2652224424413,
23.2334489783065,24.2016755141717,25.1699020500369,26.138128585902,27.1063551217672,
27.5904683896998,28.0745816576324),.UNSPECIFIED.);
#257=B_SPLINE_SURFACE_WITH_KNOTS('',3,3,((#43680,#43681,#43682,#43683,#43684,
#43685,#43686,#43687,#43688,#43689,#43690,#43691,#43692,#43693,#43694,#43695,
#43696,#43697,#43698,#43699,#43700,#43701,#43702,#43703),(#43704,#43705,
#43706,#43707,#43708,#43709,#43710,#43711,#43712,#43713,#43714,#43715,#43716,
#43717,#43718,#43719,#43720,#43721,#43722,#43723,#43724,#43725,#43726,#43727),
(#43728,#43729,#43730,#43731,#43732,#43733,#43734,#43735,#43736,#43737,
#43738,#43739,#43740,#43741,#43742,#43743,#43744,#43745,#43746,#43747,#43748,
#43749,#43750,#43751),(#43752,#43753,#43754,#43755,#43756,#43757,#43758,
#43759,#43760,#43761,#43762,#43763,#43764,#43765,#43766,#43767,#43768,#43769,
#43770,#43771,#43772,#43773,#43774,#43775)),.UNSPECIFIED.,.F.,.F.,.F.,(4,
4),(4,1,1,1,1,1,1,1,1,1,1,1,1,1,1,1,1,1,1,1,1,4),(0.,0.098669161004507),
(8.30989595155341,8.79743208801023,9.28496822446705,10.2600404973807,11.2351127702943,
12.2101850432079,13.1852573161216,14.1603295890352,15.1354018619488,16.1104741348625,
17.0855464077761,18.0606186806897,19.0356909536033,20.010763226517,20.9858354994306,
21.9609077723442,22.9359800452579,23.9110523181715,24.8861245910851,25.8611968639988,
26.3487330004556,26.8362691369124),.UNSPECIFIED.);
#258=FACE_BOUND('',#1208,.T.);
#259=FACE_BOUND('',#1212,.T.);
#260=FACE_BOUND('',#1245,.T.);
#261=FACE_BOUND('',#1250,.T.);
#262=FACE_BOUND('',#1254,.T.);
#263=FACE_BOUND('',#1256,.T.);
#264=FACE_BOUND('',#1257,.T.);
#265=FACE_BOUND('',#1258,.T.);
#266=FACE_BOUND('',#1266,.T.);
#267=FACE_BOUND('',#1272,.T.);
#268=FACE_BOUND('',#1275,.T.);
#269=FACE_BOUND('',#1276,.T.);
#270=FACE_BOUND('',#1277,.T.);
#271=FACE_BOUND('',#1278,.T.);
#272=FACE_BOUND('',#1279,.T.);
#273=FACE_BOUND('',#1281,.T.);
#274=FACE_BOUND('',#1282,.T.);
#275=FACE_BOUND('',#1283,.T.);
#276=FACE_BOUND('',#1284,.T.);
#277=FACE_BOUND('',#1308,.T.);
#278=FACE_BOUND('',#1318,.T.);
#279=FACE_BOUND('',#1321,.T.);
#280=FACE_BOUND('',#1326,.T.);
#281=FACE_BOUND('',#1328,.T.);
#282=FACE_BOUND('',#1329,.T.);
#283=FACE_BOUND('',#1330,.T.);
#284=FACE_BOUND('',#1331,.T.);
#285=FACE_BOUND('',#1332,.T.);
#286=FACE_BOUND('',#1336,.T.);
#287=FACE_BOUND('',#1339,.T.);
#288=FACE_BOUND('',#1342,.T.);
#289=FACE_BOUND('',#1350,.T.);
#290=FACE_BOUND('',#1356,.T.);
#291=FACE_BOUND('',#1357,.T.);
#292=FACE_BOUND('',#1358,.T.);
#293=FACE_BOUND('',#1359,.T.);
#294=FACE_BOUND('',#1360,.T.);
#295=FACE_BOUND('',#1362,.T.);
#296=FACE_BOUND('',#1365,.T.);
#297=FACE_BOUND('',#1369,.T.);
#298=FACE_BOUND('',#1431,.T.);
#299=FACE_BOUND('',#1432,.T.);
#300=FACE_BOUND('',#1449,.T.);
#301=FACE_BOUND('',#1451,.T.);
#302=FACE_BOUND('',#1462,.T.);
#303=FACE_BOUND('',#1464,.T.);
#304=FACE_BOUND('',#1465,.T.);
#305=FACE_BOUND('',#1466,.T.);
#306=FACE_BOUND('',#1470,.T.);
#307=FACE_BOUND('',#1473,.T.);
#308=FACE_BOUND('',#1475,.T.);
#309=FACE_BOUND('',#1478,.T.);
#310=FACE_BOUND('',#1483,.T.);
#311=FACE_BOUND('',#1491,.T.);
#312=FACE_BOUND('',#1492,.T.);
#313=FACE_BOUND('',#1494,.T.);
#314=FACE_BOUND('',#1495,.T.);
#315=FACE_BOUND('',#1577,.T.);
#316=FACE_BOUND('',#1579,.T.);
#317=FACE_BOUND('',#1609,.T.);
#318=FACE_BOUND('',#1615,.T.);
#319=FACE_BOUND('',#1616,.T.);
#320=FACE_BOUND('',#1624,.T.);
#321=FACE_BOUND('',#1626,.T.);
#322=FACE_BOUND('',#1629,.T.);
#323=FACE_BOUND('',#1682,.T.);
#324=FACE_BOUND('',#1685,.T.);
#325=FACE_BOUND('',#1720,.T.);
#326=FACE_BOUND('',#1723,.T.);
#327=FACE_BOUND('',#1774,.T.);
#328=FACE_BOUND('',#1777,.T.);
#329=FACE_BOUND('',#1796,.T.);
#330=FACE_BOUND('',#1799,.T.);
#331=PLANE('',#11561);
#332=PLANE('',#11568);
#333=PLANE('',#11575);
#334=PLANE('',#11578);
#335=PLANE('',#11581);
#336=PLANE('',#11584);
#337=PLANE('',#11587);
#338=PLANE('',#11588);
#339=PLANE('',#11589);
#340=PLANE('',#11590);
#341=PLANE('',#11597);
#342=PLANE('',#11598);
#343=PLANE('',#11599);
#344=PLANE('',#11600);
#345=PLANE('',#11601);
#346=PLANE('',#11602);
#347=PLANE('',#11603);
#348=PLANE('',#11604);
#349=PLANE('',#11611);
#350=PLANE('',#11612);
#351=PLANE('',#11619);
#352=PLANE('',#11622);
#353=PLANE('',#11625);
#354=PLANE('',#11626);
#355=PLANE('',#11629);
#356=PLANE('',#11630);
#357=PLANE('',#11631);
#358=PLANE('',#11632);
#359=PLANE('',#11633);
#360=PLANE('',#11634);
#361=PLANE('',#11635);
#362=PLANE('',#11659);
#363=PLANE('',#11661);
#364=PLANE('',#11663);
#365=PLANE('',#11664);
#366=PLANE('',#11665);
#367=PLANE('',#11667);
#368=PLANE('',#11668);
#369=PLANE('',#11669);
#370=PLANE('',#11671);
#371=PLANE('',#11675);
#372=PLANE('',#11680);
#373=PLANE('',#11684);
#374=PLANE('',#11690);
#375=PLANE('',#11691);
#376=PLANE('',#11692);
#377=PLANE('',#11701);
#378=PLANE('',#11705);
#379=PLANE('',#11708);
#380=PLANE('',#11722);
#381=PLANE('',#11723);
#382=PLANE('',#11724);
#383=PLANE('',#11725);
#384=PLANE('',#11726);
#385=PLANE('',#11728);
#386=PLANE('',#11733);
#387=PLANE('',#11739);
#388=PLANE('',#11812);
#389=PLANE('',#11817);
#390=PLANE('',#11820);
#391=PLANE('',#11832);
#392=PLANE('',#11835);
#393=PLANE('',#11840);
#394=PLANE('',#11841);
#395=PLANE('',#11842);
#396=PLANE('',#11843);
#397=PLANE('',#11844);
#398=PLANE('',#11849);
#399=PLANE('',#11850);
#400=PLANE('',#11858);
#401=PLANE('',#11863);
#402=PLANE('',#11865);
#403=PLANE('',#11869);
#404=PLANE('',#11877);
#405=PLANE('',#11885);
#406=PLANE('',#11886);
#407=PLANE('',#11887);
#408=PLANE('',#11888);
#409=PLANE('',#11889);
#410=PLANE('',#11890);
#411=PLANE('',#11894);
#412=PLANE('',#11895);
#413=PLANE('',#11969);
#414=PLANE('',#11972);
#415=PLANE('',#11973);
#416=PLANE('',#11976);
#417=PLANE('',#11977);
#418=PLANE('',#11978);
#419=PLANE('',#11979);
#420=PLANE('',#11980);
#421=PLANE('',#11981);
#422=PLANE('',#11982);
#423=PLANE('',#12010);
#424=PLANE('',#12013);
#425=PLANE('',#12017);
#426=PLANE('',#12018);
#427=PLANE('',#12019);
#428=PLANE('',#12020);
#429=PLANE('',#12021);
#430=PLANE('',#12022);
#431=PLANE('',#12023);
#432=PLANE('',#12024);
#433=PLANE('',#12029);
#434=PLANE('',#12030);
#435=PLANE('',#12031);
#436=PLANE('',#12032);
#437=PLANE('',#12033);
#438=PLANE('',#12034);
#439=PLANE('',#12039);
#440=PLANE('',#12044);
#441=PLANE('',#12047);
#442=PLANE('',#12051);
#443=PLANE('',#12052);
#444=PLANE('',#12094);
#445=PLANE('',#12095);
#446=PLANE('',#12096);
#447=PLANE('',#12097);
#448=PLANE('',#12098);
#449=PLANE('',#12099);
#450=PLANE('',#12100);
#451=PLANE('',#12101);
#452=PLANE('',#12105);
#453=PLANE('',#12106);
#454=PLANE('',#12136);
#455=PLANE('',#12137);
#456=PLANE('',#12138);
#457=PLANE('',#12139);
#458=PLANE('',#12140);
#459=PLANE('',#12141);
#460=PLANE('',#12142);
#461=PLANE('',#12143);
#462=PLANE('',#12147);
#463=PLANE('',#12148);
#464=PLANE('',#12194);
#465=PLANE('',#12195);
#466=PLANE('',#12196);
#467=PLANE('',#12197);
#468=PLANE('',#12198);
#469=PLANE('',#12199);
#470=PLANE('',#12200);
#471=PLANE('',#12201);
#472=PLANE('',#12205);
#473=PLANE('',#12206);
#474=PLANE('',#12220);
#475=PLANE('',#12221);
#476=PLANE('',#12222);
#477=PLANE('',#12223);
#478=PLANE('',#12224);
#479=PLANE('',#12225);
#480=PLANE('',#12226);
#481=PLANE('',#12227);
#482=PLANE('',#12231);
#483=PLANE('',#12232);
#484=FACE_OUTER_BOUND('',#1106,.T.);
#485=FACE_OUTER_BOUND('',#1107,.T.);
#486=FACE_OUTER_BOUND('',#1108,.T.);
#487=FACE_OUTER_BOUND('',#1109,.T.);
#488=FACE_OUTER_BOUND('',#1110,.T.);
#489=FACE_OUTER_BOUND('',#1111,.T.);
#490=FACE_OUTER_BOUND('',#1112,.T.);
#491=FACE_OUTER_BOUND('',#1113,.T.);
#492=FACE_OUTER_BOUND('',#1114,.T.);
#493=FACE_OUTER_BOUND('',#1115,.T.);
#494=FACE_OUTER_BOUND('',#1116,.T.);
#495=FACE_OUTER_BOUND('',#1117,.T.);
#496=FACE_OUTER_BOUND('',#1118,.T.);
#497=FACE_OUTER_BOUND('',#1119,.T.);
#498=FACE_OUTER_BOUND('',#1120,.T.);
#499=FACE_OUTER_BOUND('',#1121,.T.);
#500=FACE_OUTER_BOUND('',#1122,.T.);
#501=FACE_OUTER_BOUND('',#1123,.T.);
#502=FACE_OUTER_BOUND('',#1124,.T.);
#503=FACE_OUTER_BOUND('',#1125,.T.);
#504=FACE_OUTER_BOUND('',#1126,.T.);
#505=FACE_OUTER_BOUND('',#1127,.T.);
#506=FACE_OUTER_BOUND('',#1128,.T.);
#507=FACE_OUTER_BOUND('',#1129,.T.);
#508=FACE_OUTER_BOUND('',#1130,.T.);
#509=FACE_OUTER_BOUND('',#1131,.T.);
#510=FACE_OUTER_BOUND('',#1132,.T.);
#511=FACE_OUTER_BOUND('',#1133,.T.);
#512=FACE_OUTER_BOUND('',#1134,.T.);
#513=FACE_OUTER_BOUND('',#1135,.T.);
#514=FACE_OUTER_BOUND('',#1136,.T.);
#515=FACE_OUTER_BOUND('',#1137,.T.);
#516=FACE_OUTER_BOUND('',#1138,.T.);
#517=FACE_OUTER_BOUND('',#1139,.T.);
#518=FACE_OUTER_BOUND('',#1140,.T.);
#519=FACE_OUTER_BOUND('',#1141,.T.);
#520=FACE_OUTER_BOUND('',#1142,.T.);
#521=FACE_OUTER_BOUND('',#1143,.T.);
#522=FACE_OUTER_BOUND('',#1144,.T.);
#523=FACE_OUTER_BOUND('',#1145,.T.);
#524=FACE_OUTER_BOUND('',#1146,.T.);
#525=FACE_OUTER_BOUND('',#1147,.T.);
#526=FACE_OUTER_BOUND('',#1148,.T.);
#527=FACE_OUTER_BOUND('',#1149,.T.);
#528=FACE_OUTER_BOUND('',#1150,.T.);
#529=FACE_OUTER_BOUND('',#1151,.T.);
#530=FACE_OUTER_BOUND('',#1152,.T.);
#531=FACE_OUTER_BOUND('',#1153,.T.);
#532=FACE_OUTER_BOUND('',#1154,.T.);
#533=FACE_OUTER_BOUND('',#1155,.T.);
#534=FACE_OUTER_BOUND('',#1156,.T.);
#535=FACE_OUTER_BOUND('',#1157,.T.);
#536=FACE_OUTER_BOUND('',#1158,.T.);
#537=FACE_OUTER_BOUND('',#1159,.T.);
#538=FACE_OUTER_BOUND('',#1160,.T.);
#539=FACE_OUTER_BOUND('',#1161,.T.);
#540=FACE_OUTER_BOUND('',#1162,.T.);
#541=FACE_OUTER_BOUND('',#1163,.T.);
#542=FACE_OUTER_BOUND('',#1164,.T.);
#543=FACE_OUTER_BOUND('',#1165,.T.);
#544=FACE_OUTER_BOUND('',#1166,.T.);
#545=FACE_OUTER_BOUND('',#1167,.T.);
#546=FACE_OUTER_BOUND('',#1168,.T.);
#547=FACE_OUTER_BOUND('',#1169,.T.);
#548=FACE_OUTER_BOUND('',#1170,.T.);
#549=FACE_OUTER_BOUND('',#1171,.T.);
#550=FACE_OUTER_BOUND('',#1172,.T.);
#551=FACE_OUTER_BOUND('',#1173,.T.);
#552=FACE_OUTER_BOUND('',#1174,.T.);
#553=FACE_OUTER_BOUND('',#1175,.T.);
#554=FACE_OUTER_BOUND('',#1176,.T.);
#555=FACE_OUTER_BOUND('',#1177,.T.);
#556=FACE_OUTER_BOUND('',#1178,.T.);
#557=FACE_OUTER_BOUND('',#1179,.T.);
#558=FACE_OUTER_BOUND('',#1180,.T.);
#559=FACE_OUTER_BOUND('',#1181,.T.);
#560=FACE_OUTER_BOUND('',#1182,.T.);
#561=FACE_OUTER_BOUND('',#1183,.T.);
#562=FACE_OUTER_BOUND('',#1184,.T.);
#563=FACE_OUTER_BOUND('',#1185,.T.);
#564=FACE_OUTER_BOUND('',#1186,.T.);
#565=FACE_OUTER_BOUND('',#1187,.T.);
#566=FACE_OUTER_BOUND('',#1188,.T.);
#567=FACE_OUTER_BOUND('',#1189,.T.);
#568=FACE_OUTER_BOUND('',#1190,.T.);
#569=FACE_OUTER_BOUND('',#1191,.T.);
#570=FACE_OUTER_BOUND('',#1192,.T.);
#571=FACE_OUTER_BOUND('',#1193,.T.);
#572=FACE_OUTER_BOUND('',#1194,.T.);
#573=FACE_OUTER_BOUND('',#1195,.T.);
#574=FACE_OUTER_BOUND('',#1196,.T.);
#575=FACE_OUTER_BOUND('',#1197,.T.);
#576=FACE_OUTER_BOUND('',#1198,.T.);
#577=FACE_OUTER_BOUND('',#1199,.T.);
#578=FACE_OUTER_BOUND('',#1200,.T.);
#579=FACE_OUTER_BOUND('',#1201,.T.);
#580=FACE_OUTER_BOUND('',#1202,.T.);
#581=FACE_OUTER_BOUND('',#1203,.T.);
#582=FACE_OUTER_BOUND('',#1204,.T.);
#583=FACE_OUTER_BOUND('',#1205,.T.);
#584=FACE_OUTER_BOUND('',#1206,.T.);
#585=FACE_OUTER_BOUND('',#1207,.T.);
#586=FACE_OUTER_BOUND('',#1209,.T.);
#587=FACE_OUTER_BOUND('',#1210,.T.);
#588=FACE_OUTER_BOUND('',#1211,.T.);
#589=FACE_OUTER_BOUND('',#1213,.T.);
#590=FACE_OUTER_BOUND('',#1214,.T.);
#591=FACE_OUTER_BOUND('',#1215,.T.);
#592=FACE_OUTER_BOUND('',#1216,.T.);
#593=FACE_OUTER_BOUND('',#1217,.T.);
#594=FACE_OUTER_BOUND('',#1218,.T.);
#595=FACE_OUTER_BOUND('',#1219,.T.);
#596=FACE_OUTER_BOUND('',#1220,.T.);
#597=FACE_OUTER_BOUND('',#1221,.T.);
#598=FACE_OUTER_BOUND('',#1222,.T.);
#599=FACE_OUTER_BOUND('',#1223,.T.);
#600=FACE_OUTER_BOUND('',#1224,.T.);
#601=FACE_OUTER_BOUND('',#1225,.T.);
#602=FACE_OUTER_BOUND('',#1226,.T.);
#603=FACE_OUTER_BOUND('',#1227,.T.);
#604=FACE_OUTER_BOUND('',#1228,.T.);
#605=FACE_OUTER_BOUND('',#1229,.T.);
#606=FACE_OUTER_BOUND('',#1230,.T.);
#607=FACE_OUTER_BOUND('',#1231,.T.);
#608=FACE_OUTER_BOUND('',#1232,.T.);
#609=FACE_OUTER_BOUND('',#1233,.T.);
#610=FACE_OUTER_BOUND('',#1234,.T.);
#611=FACE_OUTER_BOUND('',#1235,.T.);
#612=FACE_OUTER_BOUND('',#1236,.T.);
#613=FACE_OUTER_BOUND('',#1237,.T.);
#614=FACE_OUTER_BOUND('',#1238,.T.);
#615=FACE_OUTER_BOUND('',#1239,.T.);
#616=FACE_OUTER_BOUND('',#1240,.T.);
#617=FACE_OUTER_BOUND('',#1241,.T.);
#618=FACE_OUTER_BOUND('',#1242,.T.);
#619=FACE_OUTER_BOUND('',#1243,.T.);
#620=FACE_OUTER_BOUND('',#1244,.T.);
#621=FACE_OUTER_BOUND('',#1246,.T.);
#622=FACE_OUTER_BOUND('',#1247,.T.);
#623=FACE_OUTER_BOUND('',#1248,.T.);
#624=FACE_OUTER_BOUND('',#1249,.T.);
#625=FACE_OUTER_BOUND('',#1251,.T.);
#626=FACE_OUTER_BOUND('',#1252,.T.);
#627=FACE_OUTER_BOUND('',#1253,.T.);
#628=FACE_OUTER_BOUND('',#1255,.T.);
#629=FACE_OUTER_BOUND('',#1259,.T.);
#630=FACE_OUTER_BOUND('',#1260,.T.);
#631=FACE_OUTER_BOUND('',#1261,.T.);
#632=FACE_OUTER_BOUND('',#1262,.T.);
#633=FACE_OUTER_BOUND('',#1263,.T.);
#634=FACE_OUTER_BOUND('',#1264,.T.);
#635=FACE_OUTER_BOUND('',#1265,.T.);
#636=FACE_OUTER_BOUND('',#1267,.T.);
#637=FACE_OUTER_BOUND('',#1268,.T.);
#638=FACE_OUTER_BOUND('',#1269,.T.);
#639=FACE_OUTER_BOUND('',#1270,.T.);
#640=FACE_OUTER_BOUND('',#1271,.T.);
#641=FACE_OUTER_BOUND('',#1273,.T.);
#642=FACE_OUTER_BOUND('',#1274,.T.);
#643=FACE_OUTER_BOUND('',#1280,.T.);
#644=FACE_OUTER_BOUND('',#1285,.T.);
#645=FACE_OUTER_BOUND('',#1286,.T.);
#646=FACE_OUTER_BOUND('',#1287,.T.);
#647=FACE_OUTER_BOUND('',#1288,.T.);
#648=FACE_OUTER_BOUND('',#1289,.T.);
#649=FACE_OUTER_BOUND('',#1290,.T.);
#650=FACE_OUTER_BOUND('',#1291,.T.);
#651=FACE_OUTER_BOUND('',#1292,.T.);
#652=FACE_OUTER_BOUND('',#1293,.T.);
#653=FACE_OUTER_BOUND('',#1294,.T.);
#654=FACE_OUTER_BOUND('',#1295,.T.);
#655=FACE_OUTER_BOUND('',#1296,.T.);
#656=FACE_OUTER_BOUND('',#1297,.T.);
#657=FACE_OUTER_BOUND('',#1298,.T.);
#658=FACE_OUTER_BOUND('',#1299,.T.);
#659=FACE_OUTER_BOUND('',#1300,.T.);
#660=FACE_OUTER_BOUND('',#1301,.T.);
#661=FACE_OUTER_BOUND('',#1302,.T.);
#662=FACE_OUTER_BOUND('',#1303,.T.);
#663=FACE_OUTER_BOUND('',#1304,.T.);
#664=FACE_OUTER_BOUND('',#1305,.T.);
#665=FACE_OUTER_BOUND('',#1306,.T.);
#666=FACE_OUTER_BOUND('',#1307,.T.);
#667=FACE_OUTER_BOUND('',#1309,.T.);
#668=FACE_OUTER_BOUND('',#1310,.T.);
#669=FACE_OUTER_BOUND('',#1311,.T.);
#670=FACE_OUTER_BOUND('',#1312,.T.);
#671=FACE_OUTER_BOUND('',#1313,.T.);
#672=FACE_OUTER_BOUND('',#1314,.T.);
#673=FACE_OUTER_BOUND('',#1315,.T.);
#674=FACE_OUTER_BOUND('',#1316,.T.);
#675=FACE_OUTER_BOUND('',#1317,.T.);
#676=FACE_OUTER_BOUND('',#1319,.T.);
#677=FACE_OUTER_BOUND('',#1320,.T.);
#678=FACE_OUTER_BOUND('',#1322,.T.);
#679=FACE_OUTER_BOUND('',#1323,.T.);
#680=FACE_OUTER_BOUND('',#1324,.T.);
#681=FACE_OUTER_BOUND('',#1325,.T.);
#682=FACE_OUTER_BOUND('',#1327,.T.);
#683=FACE_OUTER_BOUND('',#1333,.T.);
#684=FACE_OUTER_BOUND('',#1334,.T.);
#685=FACE_OUTER_BOUND('',#1335,.T.);
#686=FACE_OUTER_BOUND('',#1337,.T.);
#687=FACE_OUTER_BOUND('',#1338,.T.);
#688=FACE_OUTER_BOUND('',#1340,.T.);
#689=FACE_OUTER_BOUND('',#1341,.T.);
#690=FACE_OUTER_BOUND('',#1343,.T.);
#691=FACE_OUTER_BOUND('',#1344,.T.);
#692=FACE_OUTER_BOUND('',#1345,.T.);
#693=FACE_OUTER_BOUND('',#1346,.T.);
#694=FACE_OUTER_BOUND('',#1347,.T.);
#695=FACE_OUTER_BOUND('',#1348,.T.);
#696=FACE_OUTER_BOUND('',#1349,.T.);
#697=FACE_OUTER_BOUND('',#1351,.T.);
#698=FACE_OUTER_BOUND('',#1352,.T.);
#699=FACE_OUTER_BOUND('',#1353,.T.);
#700=FACE_OUTER_BOUND('',#1354,.T.);
#701=FACE_OUTER_BOUND('',#1355,.T.);
#702=FACE_OUTER_BOUND('',#1361,.T.);
#703=FACE_OUTER_BOUND('',#1363,.T.);
#704=FACE_OUTER_BOUND('',#1364,.T.);
#705=FACE_OUTER_BOUND('',#1366,.T.);
#706=FACE_OUTER_BOUND('',#1367,.T.);
#707=FACE_OUTER_BOUND('',#1368,.T.);
#708=FACE_OUTER_BOUND('',#1370,.T.);
#709=FACE_OUTER_BOUND('',#1371,.T.);
#710=FACE_OUTER_BOUND('',#1372,.T.);
#711=FACE_OUTER_BOUND('',#1373,.T.);
#712=FACE_OUTER_BOUND('',#1374,.T.);
#713=FACE_OUTER_BOUND('',#1375,.T.);
#714=FACE_OUTER_BOUND('',#1376,.T.);
#715=FACE_OUTER_BOUND('',#1377,.T.);
#716=FACE_OUTER_BOUND('',#1378,.T.);
#717=FACE_OUTER_BOUND('',#1379,.T.);
#718=FACE_OUTER_BOUND('',#1380,.T.);
#719=FACE_OUTER_BOUND('',#1381,.T.);
#720=FACE_OUTER_BOUND('',#1382,.T.);
#721=FACE_OUTER_BOUND('',#1383,.T.);
#722=FACE_OUTER_BOUND('',#1384,.T.);
#723=FACE_OUTER_BOUND('',#1385,.T.);
#724=FACE_OUTER_BOUND('',#1386,.T.);
#725=FACE_OUTER_BOUND('',#1387,.T.);
#726=FACE_OUTER_BOUND('',#1388,.T.);
#727=FACE_OUTER_BOUND('',#1389,.T.);
#728=FACE_OUTER_BOUND('',#1390,.T.);
#729=FACE_OUTER_BOUND('',#1391,.T.);
#730=FACE_OUTER_BOUND('',#1392,.T.);
#731=FACE_OUTER_BOUND('',#1393,.T.);
#732=FACE_OUTER_BOUND('',#1394,.T.);
#733=FACE_OUTER_BOUND('',#1395,.T.);
#734=FACE_OUTER_BOUND('',#1396,.T.);
#735=FACE_OUTER_BOUND('',#1397,.T.);
#736=FACE_OUTER_BOUND('',#1398,.T.);
#737=FACE_OUTER_BOUND('',#1399,.T.);
#738=FACE_OUTER_BOUND('',#1400,.T.);
#739=FACE_OUTER_BOUND('',#1401,.T.);
#740=FACE_OUTER_BOUND('',#1402,.T.);
#741=FACE_OUTER_BOUND('',#1403,.T.);
#742=FACE_OUTER_BOUND('',#1404,.T.);
#743=FACE_OUTER_BOUND('',#1405,.T.);
#744=FACE_OUTER_BOUND('',#1406,.T.);
#745=FACE_OUTER_BOUND('',#1407,.T.);
#746=FACE_OUTER_BOUND('',#1408,.T.);
#747=FACE_OUTER_BOUND('',#1409,.T.);
#748=FACE_OUTER_BOUND('',#1410,.T.);
#749=FACE_OUTER_BOUND('',#1411,.T.);
#750=FACE_OUTER_BOUND('',#1412,.T.);
#751=FACE_OUTER_BOUND('',#1413,.T.);
#752=FACE_OUTER_BOUND('',#1414,.T.);
#753=FACE_OUTER_BOUND('',#1415,.T.);
#754=FACE_OUTER_BOUND('',#1416,.T.);
#755=FACE_OUTER_BOUND('',#1417,.T.);
#756=FACE_OUTER_BOUND('',#1418,.T.);
#757=FACE_OUTER_BOUND('',#1419,.T.);
#758=FACE_OUTER_BOUND('',#1420,.T.);
#759=FACE_OUTER_BOUND('',#1421,.T.);
#760=FACE_OUTER_BOUND('',#1422,.T.);
#761=FACE_OUTER_BOUND('',#1423,.T.);
#762=FACE_OUTER_BOUND('',#1424,.T.);
#763=FACE_OUTER_BOUND('',#1425,.T.);
#764=FACE_OUTER_BOUND('',#1426,.T.);
#765=FACE_OUTER_BOUND('',#1427,.T.);
#766=FACE_OUTER_BOUND('',#1428,.T.);
#767=FACE_OUTER_BOUND('',#1429,.T.);
#768=FACE_OUTER_BOUND('',#1430,.T.);
#769=FACE_OUTER_BOUND('',#1433,.T.);
#770=FACE_OUTER_BOUND('',#1434,.T.);
#771=FACE_OUTER_BOUND('',#1435,.T.);
#772=FACE_OUTER_BOUND('',#1436,.T.);
#773=FACE_OUTER_BOUND('',#1437,.T.);
#774=FACE_OUTER_BOUND('',#1438,.T.);
#775=FACE_OUTER_BOUND('',#1439,.T.);
#776=FACE_OUTER_BOUND('',#1440,.T.);
#777=FACE_OUTER_BOUND('',#1441,.T.);
#778=FACE_OUTER_BOUND('',#1442,.T.);
#779=FACE_OUTER_BOUND('',#1443,.T.);
#780=FACE_OUTER_BOUND('',#1444,.T.);
#781=FACE_OUTER_BOUND('',#1445,.T.);
#782=FACE_OUTER_BOUND('',#1446,.T.);
#783=FACE_OUTER_BOUND('',#1447,.T.);
#784=FACE_OUTER_BOUND('',#1448,.T.);
#785=FACE_OUTER_BOUND('',#1450,.T.);
#786=FACE_OUTER_BOUND('',#1452,.T.);
#787=FACE_OUTER_BOUND('',#1453,.T.);
#788=FACE_OUTER_BOUND('',#1454,.T.);
#789=FACE_OUTER_BOUND('',#1455,.T.);
#790=FACE_OUTER_BOUND('',#1456,.T.);
#791=FACE_OUTER_BOUND('',#1457,.T.);
#792=FACE_OUTER_BOUND('',#1458,.T.);
#793=FACE_OUTER_BOUND('',#1459,.T.);
#794=FACE_OUTER_BOUND('',#1460,.T.);
#795=FACE_OUTER_BOUND('',#1461,.T.);
#796=FACE_OUTER_BOUND('',#1463,.T.);
#797=FACE_OUTER_BOUND('',#1467,.T.);
#798=FACE_OUTER_BOUND('',#1468,.T.);
#799=FACE_OUTER_BOUND('',#1469,.T.);
#800=FACE_OUTER_BOUND('',#1471,.T.);
#801=FACE_OUTER_BOUND('',#1472,.T.);
#802=FACE_OUTER_BOUND('',#1474,.T.);
#803=FACE_OUTER_BOUND('',#1476,.T.);
#804=FACE_OUTER_BOUND('',#1477,.T.);
#805=FACE_OUTER_BOUND('',#1479,.T.);
#806=FACE_OUTER_BOUND('',#1480,.T.);
#807=FACE_OUTER_BOUND('',#1481,.T.);
#808=FACE_OUTER_BOUND('',#1482,.T.);
#809=FACE_OUTER_BOUND('',#1484,.T.);
#810=FACE_OUTER_BOUND('',#1485,.T.);
#811=FACE_OUTER_BOUND('',#1486,.T.);
#812=FACE_OUTER_BOUND('',#1487,.T.);
#813=FACE_OUTER_BOUND('',#1488,.T.);
#814=FACE_OUTER_BOUND('',#1489,.T.);
#815=FACE_OUTER_BOUND('',#1490,.T.);
#816=FACE_OUTER_BOUND('',#1493,.T.);
#817=FACE_OUTER_BOUND('',#1496,.T.);
#818=FACE_OUTER_BOUND('',#1497,.T.);
#819=FACE_OUTER_BOUND('',#1498,.T.);
#820=FACE_OUTER_BOUND('',#1499,.T.);
#821=FACE_OUTER_BOUND('',#1500,.T.);
#822=FACE_OUTER_BOUND('',#1501,.T.);
#823=FACE_OUTER_BOUND('',#1502,.T.);
#824=FACE_OUTER_BOUND('',#1503,.T.);
#825=FACE_OUTER_BOUND('',#1504,.T.);
#826=FACE_OUTER_BOUND('',#1505,.T.);
#827=FACE_OUTER_BOUND('',#1506,.T.);
#828=FACE_OUTER_BOUND('',#1507,.T.);
#829=FACE_OUTER_BOUND('',#1508,.T.);
#830=FACE_OUTER_BOUND('',#1509,.T.);
#831=FACE_OUTER_BOUND('',#1510,.T.);
#832=FACE_OUTER_BOUND('',#1511,.T.);
#833=FACE_OUTER_BOUND('',#1512,.T.);
#834=FACE_OUTER_BOUND('',#1513,.T.);
#835=FACE_OUTER_BOUND('',#1514,.T.);
#836=FACE_OUTER_BOUND('',#1515,.T.);
#837=FACE_OUTER_BOUND('',#1516,.T.);
#838=FACE_OUTER_BOUND('',#1517,.T.);
#839=FACE_OUTER_BOUND('',#1518,.T.);
#840=FACE_OUTER_BOUND('',#1519,.T.);
#841=FACE_OUTER_BOUND('',#1520,.T.);
#842=FACE_OUTER_BOUND('',#1521,.T.);
#843=FACE_OUTER_BOUND('',#1522,.T.);
#844=FACE_OUTER_BOUND('',#1523,.T.);
#845=FACE_OUTER_BOUND('',#1524,.T.);
#846=FACE_OUTER_BOUND('',#1525,.T.);
#847=FACE_OUTER_BOUND('',#1526,.T.);
#848=FACE_OUTER_BOUND('',#1527,.T.);
#849=FACE_OUTER_BOUND('',#1528,.T.);
#850=FACE_OUTER_BOUND('',#1529,.T.);
#851=FACE_OUTER_BOUND('',#1530,.T.);
#852=FACE_OUTER_BOUND('',#1531,.T.);
#853=FACE_OUTER_BOUND('',#1532,.T.);
#854=FACE_OUTER_BOUND('',#1533,.T.);
#855=FACE_OUTER_BOUND('',#1534,.T.);
#856=FACE_OUTER_BOUND('',#1535,.T.);
#857=FACE_OUTER_BOUND('',#1536,.T.);
#858=FACE_OUTER_BOUND('',#1537,.T.);
#859=FACE_OUTER_BOUND('',#1538,.T.);
#860=FACE_OUTER_BOUND('',#1539,.T.);
#861=FACE_OUTER_BOUND('',#1540,.T.);
#862=FACE_OUTER_BOUND('',#1541,.T.);
#863=FACE_OUTER_BOUND('',#1542,.T.);
#864=FACE_OUTER_BOUND('',#1543,.T.);
#865=FACE_OUTER_BOUND('',#1544,.T.);
#866=FACE_OUTER_BOUND('',#1545,.T.);
#867=FACE_OUTER_BOUND('',#1546,.T.);
#868=FACE_OUTER_BOUND('',#1547,.T.);
#869=FACE_OUTER_BOUND('',#1548,.T.);
#870=FACE_OUTER_BOUND('',#1549,.T.);
#871=FACE_OUTER_BOUND('',#1550,.T.);
#872=FACE_OUTER_BOUND('',#1551,.T.);
#873=FACE_OUTER_BOUND('',#1552,.T.);
#874=FACE_OUTER_BOUND('',#1553,.T.);
#875=FACE_OUTER_BOUND('',#1554,.T.);
#876=FACE_OUTER_BOUND('',#1555,.T.);
#877=FACE_OUTER_BOUND('',#1556,.T.);
#878=FACE_OUTER_BOUND('',#1557,.T.);
#879=FACE_OUTER_BOUND('',#1558,.T.);
#880=FACE_OUTER_BOUND('',#1559,.T.);
#881=FACE_OUTER_BOUND('',#1560,.T.);
#882=FACE_OUTER_BOUND('',#1561,.T.);
#883=FACE_OUTER_BOUND('',#1562,.T.);
#884=FACE_OUTER_BOUND('',#1563,.T.);
#885=FACE_OUTER_BOUND('',#1564,.T.);
#886=FACE_OUTER_BOUND('',#1565,.T.);
#887=FACE_OUTER_BOUND('',#1566,.T.);
#888=FACE_OUTER_BOUND('',#1567,.T.);
#889=FACE_OUTER_BOUND('',#1568,.T.);
#890=FACE_OUTER_BOUND('',#1569,.T.);
#891=FACE_OUTER_BOUND('',#1570,.T.);
#892=FACE_OUTER_BOUND('',#1571,.T.);
#893=FACE_OUTER_BOUND('',#1572,.T.);
#894=FACE_OUTER_BOUND('',#1573,.T.);
#895=FACE_OUTER_BOUND('',#1574,.T.);
#896=FACE_OUTER_BOUND('',#1575,.T.);
#897=FACE_OUTER_BOUND('',#1576,.T.);
#898=FACE_OUTER_BOUND('',#1578,.T.);
#899=FACE_OUTER_BOUND('',#1580,.T.);
#900=FACE_OUTER_BOUND('',#1581,.T.);
#901=FACE_OUTER_BOUND('',#1582,.T.);
#902=FACE_OUTER_BOUND('',#1583,.T.);
#903=FACE_OUTER_BOUND('',#1584,.T.);
#904=FACE_OUTER_BOUND('',#1585,.T.);
#905=FACE_OUTER_BOUND('',#1586,.T.);
#906=FACE_OUTER_BOUND('',#1587,.T.);
#907=FACE_OUTER_BOUND('',#1588,.T.);
#908=FACE_OUTER_BOUND('',#1589,.T.);
#909=FACE_OUTER_BOUND('',#1590,.T.);
#910=FACE_OUTER_BOUND('',#1591,.T.);
#911=FACE_OUTER_BOUND('',#1592,.T.);
#912=FACE_OUTER_BOUND('',#1593,.T.);
#913=FACE_OUTER_BOUND('',#1594,.T.);
#914=FACE_OUTER_BOUND('',#1595,.T.);
#915=FACE_OUTER_BOUND('',#1596,.T.);
#916=FACE_OUTER_BOUND('',#1597,.T.);
#917=FACE_OUTER_BOUND('',#1598,.T.);
#918=FACE_OUTER_BOUND('',#1599,.T.);
#919=FACE_OUTER_BOUND('',#1600,.T.);
#920=FACE_OUTER_BOUND('',#1601,.T.);
#921=FACE_OUTER_BOUND('',#1602,.T.);
#922=FACE_OUTER_BOUND('',#1603,.T.);
#923=FACE_OUTER_BOUND('',#1604,.T.);
#924=FACE_OUTER_BOUND('',#1605,.T.);
#925=FACE_OUTER_BOUND('',#1606,.T.);
#926=FACE_OUTER_BOUND('',#1607,.T.);
#927=FACE_OUTER_BOUND('',#1608,.T.);
#928=FACE_OUTER_BOUND('',#1610,.T.);
#929=FACE_OUTER_BOUND('',#1611,.T.);
#930=FACE_OUTER_BOUND('',#1612,.T.);
#931=FACE_OUTER_BOUND('',#1613,.T.);
#932=FACE_OUTER_BOUND('',#1614,.T.);
#933=FACE_OUTER_BOUND('',#1617,.T.);
#934=FACE_OUTER_BOUND('',#1618,.T.);
#935=FACE_OUTER_BOUND('',#1619,.T.);
#936=FACE_OUTER_BOUND('',#1620,.T.);
#937=FACE_OUTER_BOUND('',#1621,.T.);
#938=FACE_OUTER_BOUND('',#1622,.T.);
#939=FACE_OUTER_BOUND('',#1623,.T.);
#940=FACE_OUTER_BOUND('',#1625,.T.);
#941=FACE_OUTER_BOUND('',#1627,.T.);
#942=FACE_OUTER_BOUND('',#1628,.T.);
#943=FACE_OUTER_BOUND('',#1630,.T.);
#944=FACE_OUTER_BOUND('',#1631,.T.);
#945=FACE_OUTER_BOUND('',#1632,.T.);
#946=FACE_OUTER_BOUND('',#1633,.T.);
#947=FACE_OUTER_BOUND('',#1634,.T.);
#948=FACE_OUTER_BOUND('',#1635,.T.);
#949=FACE_OUTER_BOUND('',#1636,.T.);
#950=FACE_OUTER_BOUND('',#1637,.T.);
#951=FACE_OUTER_BOUND('',#1638,.T.);
#952=FACE_OUTER_BOUND('',#1639,.T.);
#953=FACE_OUTER_BOUND('',#1640,.T.);
#954=FACE_OUTER_BOUND('',#1641,.T.);
#955=FACE_OUTER_BOUND('',#1642,.T.);
#956=FACE_OUTER_BOUND('',#1643,.T.);
#957=FACE_OUTER_BOUND('',#1644,.T.);
#958=FACE_OUTER_BOUND('',#1645,.T.);
#959=FACE_OUTER_BOUND('',#1646,.T.);
#960=FACE_OUTER_BOUND('',#1647,.T.);
#961=FACE_OUTER_BOUND('',#1648,.T.);
#962=FACE_OUTER_BOUND('',#1649,.T.);
#963=FACE_OUTER_BOUND('',#1650,.T.);
#964=FACE_OUTER_BOUND('',#1651,.T.);
#965=FACE_OUTER_BOUND('',#1652,.T.);
#966=FACE_OUTER_BOUND('',#1653,.T.);
#967=FACE_OUTER_BOUND('',#1654,.T.);
#968=FACE_OUTER_BOUND('',#1655,.T.);
#969=FACE_OUTER_BOUND('',#1656,.T.);
#970=FACE_OUTER_BOUND('',#1657,.T.);
#971=FACE_OUTER_BOUND('',#1658,.T.);
#972=FACE_OUTER_BOUND('',#1659,.T.);
#973=FACE_OUTER_BOUND('',#1660,.T.);
#974=FACE_OUTER_BOUND('',#1661,.T.);
#975=FACE_OUTER_BOUND('',#1662,.T.);
#976=FACE_OUTER_BOUND('',#1663,.T.);
#977=FACE_OUTER_BOUND('',#1664,.T.);
#978=FACE_OUTER_BOUND('',#1665,.T.);
#979=FACE_OUTER_BOUND('',#1666,.T.);
#980=FACE_OUTER_BOUND('',#1667,.T.);
#981=FACE_OUTER_BOUND('',#1668,.T.);
#982=FACE_OUTER_BOUND('',#1669,.T.);
#983=FACE_OUTER_BOUND('',#1670,.T.);
#984=FACE_OUTER_BOUND('',#1671,.T.);
#985=FACE_OUTER_BOUND('',#1672,.T.);
#986=FACE_OUTER_BOUND('',#1673,.T.);
#987=FACE_OUTER_BOUND('',#1674,.T.);
#988=FACE_OUTER_BOUND('',#1675,.T.);
#989=FACE_OUTER_BOUND('',#1676,.T.);
#990=FACE_OUTER_BOUND('',#1677,.T.);
#991=FACE_OUTER_BOUND('',#1678,.T.);
#992=FACE_OUTER_BOUND('',#1679,.T.);
#993=FACE_OUTER_BOUND('',#1680,.T.);
#994=FACE_OUTER_BOUND('',#1681,.T.);
#995=FACE_OUTER_BOUND('',#1683,.T.);
#996=FACE_OUTER_BOUND('',#1684,.T.);
#997=FACE_OUTER_BOUND('',#1686,.T.);
#998=FACE_OUTER_BOUND('',#1687,.T.);
#999=FACE_OUTER_BOUND('',#1688,.T.);
#1000=FACE_OUTER_BOUND('',#1689,.T.);
#1001=FACE_OUTER_BOUND('',#1690,.T.);
#1002=FACE_OUTER_BOUND('',#1691,.T.);
#1003=FACE_OUTER_BOUND('',#1692,.T.);
#1004=FACE_OUTER_BOUND('',#1693,.T.);
#1005=FACE_OUTER_BOUND('',#1694,.T.);
#1006=FACE_OUTER_BOUND('',#1695,.T.);
#1007=FACE_OUTER_BOUND('',#1696,.T.);
#1008=FACE_OUTER_BOUND('',#1697,.T.);
#1009=FACE_OUTER_BOUND('',#1698,.T.);
#1010=FACE_OUTER_BOUND('',#1699,.T.);
#1011=FACE_OUTER_BOUND('',#1700,.T.);
#1012=FACE_OUTER_BOUND('',#1701,.T.);
#1013=FACE_OUTER_BOUND('',#1702,.T.);
#1014=FACE_OUTER_BOUND('',#1703,.T.);
#1015=FACE_OUTER_BOUND('',#1704,.T.);
#1016=FACE_OUTER_BOUND('',#1705,.T.);
#1017=FACE_OUTER_BOUND('',#1706,.T.);
#1018=FACE_OUTER_BOUND('',#1707,.T.);
#1019=FACE_OUTER_BOUND('',#1708,.T.);
#1020=FACE_OUTER_BOUND('',#1709,.T.);
#1021=FACE_OUTER_BOUND('',#1710,.T.);
#1022=FACE_OUTER_BOUND('',#1711,.T.);
#1023=FACE_OUTER_BOUND('',#1712,.T.);
#1024=FACE_OUTER_BOUND('',#1713,.T.);
#1025=FACE_OUTER_BOUND('',#1714,.T.);
#1026=FACE_OUTER_BOUND('',#1715,.T.);
#1027=FACE_OUTER_BOUND('',#1716,.T.);
#1028=FACE_OUTER_BOUND('',#1717,.T.);
#1029=FACE_OUTER_BOUND('',#1718,.T.);
#1030=FACE_OUTER_BOUND('',#1719,.T.);
#1031=FACE_OUTER_BOUND('',#1721,.T.);
#1032=FACE_OUTER_BOUND('',#1722,.T.);
#1033=FACE_OUTER_BOUND('',#1724,.T.);
#1034=FACE_OUTER_BOUND('',#1725,.T.);
#1035=FACE_OUTER_BOUND('',#1726,.T.);
#1036=FACE_OUTER_BOUND('',#1727,.T.);
#1037=FACE_OUTER_BOUND('',#1728,.T.);
#1038=FACE_OUTER_BOUND('',#1729,.T.);
#1039=FACE_OUTER_BOUND('',#1730,.T.);
#1040=FACE_OUTER_BOUND('',#1731,.T.);
#1041=FACE_OUTER_BOUND('',#1732,.T.);
#1042=FACE_OUTER_BOUND('',#1733,.T.);
#1043=FACE_OUTER_BOUND('',#1734,.T.);
#1044=FACE_OUTER_BOUND('',#1735,.T.);
#1045=FACE_OUTER_BOUND('',#1736,.T.);
#1046=FACE_OUTER_BOUND('',#1737,.T.);
#1047=FACE_OUTER_BOUND('',#1738,.T.);
#1048=FACE_OUTER_BOUND('',#1739,.T.);
#1049=FACE_OUTER_BOUND('',#1740,.T.);
#1050=FACE_OUTER_BOUND('',#1741,.T.);
#1051=FACE_OUTER_BOUND('',#1742,.T.);
#1052=FACE_OUTER_BOUND('',#1743,.T.);
#1053=FACE_OUTER_BOUND('',#1744,.T.);
#1054=FACE_OUTER_BOUND('',#1745,.T.);
#1055=FACE_OUTER_BOUND('',#1746,.T.);
#1056=FACE_OUTER_BOUND('',#1747,.T.);
#1057=FACE_OUTER_BOUND('',#1748,.T.);
#1058=FACE_OUTER_BOUND('',#1749,.T.);
#1059=FACE_OUTER_BOUND('',#1750,.T.);
#1060=FACE_OUTER_BOUND('',#1751,.T.);
#1061=FACE_OUTER_BOUND('',#1752,.T.);
#1062=FACE_OUTER_BOUND('',#1753,.T.);
#1063=FACE_OUTER_BOUND('',#1754,.T.);
#1064=FACE_OUTER_BOUND('',#1755,.T.);
#1065=FACE_OUTER_BOUND('',#1756,.T.);
#1066=FACE_OUTER_BOUND('',#1757,.T.);
#1067=FACE_OUTER_BOUND('',#1758,.T.);
#1068=FACE_OUTER_BOUND('',#1759,.T.);
#1069=FACE_OUTER_BOUND('',#1760,.T.);
#1070=FACE_OUTER_BOUND('',#1761,.T.);
#1071=FACE_OUTER_BOUND('',#1762,.T.);
#1072=FACE_OUTER_BOUND('',#1763,.T.);
#1073=FACE_OUTER_BOUND('',#1764,.T.);
#1074=FACE_OUTER_BOUND('',#1765,.T.);
#1075=FACE_OUTER_BOUND('',#1766,.T.);
#1076=FACE_OUTER_BOUND('',#1767,.T.);
#1077=FACE_OUTER_BOUND('',#1768,.T.);
#1078=FACE_OUTER_BOUND('',#1769,.T.);
#1079=FACE_OUTER_BOUND('',#1770,.T.);
#1080=FACE_OUTER_BOUND('',#1771,.T.);
#1081=FACE_OUTER_BOUND('',#1772,.T.);
#1082=FACE_OUTER_BOUND('',#1773,.T.);
#1083=FACE_OUTER_BOUND('',#1775,.T.);
#1084=FACE_OUTER_BOUND('',#1776,.T.);
#1085=FACE_OUTER_BOUND('',#1778,.T.);
#1086=FACE_OUTER_BOUND('',#1779,.T.);
#1087=FACE_OUTER_BOUND('',#1780,.T.);
#1088=FACE_OUTER_BOUND('',#1781,.T.);
#1089=FACE_OUTER_BOUND('',#1782,.T.);
#1090=FACE_OUTER_BOUND('',#1783,.T.);
#1091=FACE_OUTER_BOUND('',#1784,.T.);
#1092=FACE_OUTER_BOUND('',#1785,.T.);
#1093=FACE_OUTER_BOUND('',#1786,.T.);
#1094=FACE_OUTER_BOUND('',#1787,.T.);
#1095=FACE_OUTER_BOUND('',#1788,.T.);
#1096=FACE_OUTER_BOUND('',#1789,.T.);
#1097=FACE_OUTER_BOUND('',#1790,.T.);
#1098=FACE_OUTER_BOUND('',#1791,.T.);
#1099=FACE_OUTER_BOUND('',#1792,.T.);
#1100=FACE_OUTER_BOUND('',#1793,.T.);
#1101=FACE_OUTER_BOUND('',#1794,.T.);
#1102=FACE_OUTER_BOUND('',#1795,.T.);
#1103=FACE_OUTER_BOUND('',#1797,.T.);
#1104=FACE_OUTER_BOUND('',#1798,.T.);
#1105=FACE_OUTER_BOUND('',#1800,.T.);
#1106=EDGE_LOOP('',(#6861,#6862,#6863,#6864,#6865,#6866,#6867,#6868));
#1107=EDGE_LOOP('',(#6869,#6870,#6871,#6872));
#1108=EDGE_LOOP('',(#6873,#6874,#6875,#6876));
#1109=EDGE_LOOP('',(#6877,#6878,#6879,#6880));
#1110=EDGE_LOOP('',(#6881,#6882,#6883,#6884));
#1111=EDGE_LOOP('',(#6885,#6886,#6887,#6888));
#1112=EDGE_LOOP('',(#6889,#6890,#6891,#6892));
#1113=EDGE_LOOP('',(#6893,#6894,#6895,#6896));
#1114=EDGE_LOOP('',(#6897,#6898,#6899,#6900));
#1115=EDGE_LOOP('',(#6901,#6902,#6903,#6904));
#1116=EDGE_LOOP('',(#6905,#6906,#6907,#6908));
#1117=EDGE_LOOP('',(#6909,#6910,#6911,#6912));
#1118=EDGE_LOOP('',(#6913,#6914,#6915,#6916));
#1119=EDGE_LOOP('',(#6917,#6918,#6919,#6920));
#1120=EDGE_LOOP('',(#6921,#6922,#6923,#6924));
#1121=EDGE_LOOP('',(#6925,#6926,#6927,#6928));
#1122=EDGE_LOOP('',(#6929,#6930,#6931,#6932));
#1123=EDGE_LOOP('',(#6933,#6934,#6935,#6936));
#1124=EDGE_LOOP('',(#6937,#6938,#6939,#6940));
#1125=EDGE_LOOP('',(#6941,#6942,#6943,#6944));
#1126=EDGE_LOOP('',(#6945,#6946,#6947,#6948));
#1127=EDGE_LOOP('',(#6949,#6950,#6951,#6952));
#1128=EDGE_LOOP('',(#6953,#6954,#6955,#6956));
#1129=EDGE_LOOP('',(#6957,#6958,#6959,#6960));
#1130=EDGE_LOOP('',(#6961,#6962,#6963,#6964));
#1131=EDGE_LOOP('',(#6965,#6966,#6967,#6968,#6969,#6970,#6971,#6972));
#1132=EDGE_LOOP('',(#6973,#6974,#6975,#6976));
#1133=EDGE_LOOP('',(#6977,#6978,#6979,#6980));
#1134=EDGE_LOOP('',(#6981,#6982,#6983,#6984));
#1135=EDGE_LOOP('',(#6985,#6986,#6987,#6988));
#1136=EDGE_LOOP('',(#6989,#6990,#6991,#6992));
#1137=EDGE_LOOP('',(#6993,#6994,#6995,#6996));
#1138=EDGE_LOOP('',(#6997,#6998,#6999,#7000));
#1139=EDGE_LOOP('',(#7001,#7002,#7003,#7004));
#1140=EDGE_LOOP('',(#7005,#7006,#7007,#7008));
#1141=EDGE_LOOP('',(#7009,#7010,#7011,#7012));
#1142=EDGE_LOOP('',(#7013,#7014,#7015,#7016));
#1143=EDGE_LOOP('',(#7017,#7018,#7019,#7020));
#1144=EDGE_LOOP('',(#7021,#7022,#7023,#7024));
#1145=EDGE_LOOP('',(#7025,#7026,#7027,#7028));
#1146=EDGE_LOOP('',(#7029,#7030,#7031,#7032));
#1147=EDGE_LOOP('',(#7033,#7034,#7035,#7036));
#1148=EDGE_LOOP('',(#7037,#7038,#7039,#7040));
#1149=EDGE_LOOP('',(#7041,#7042,#7043,#7044));
#1150=EDGE_LOOP('',(#7045,#7046,#7047,#7048));
#1151=EDGE_LOOP('',(#7049,#7050,#7051,#7052));
#1152=EDGE_LOOP('',(#7053,#7054,#7055,#7056));
#1153=EDGE_LOOP('',(#7057,#7058,#7059,#7060));
#1154=EDGE_LOOP('',(#7061,#7062,#7063,#7064));
#1155=EDGE_LOOP('',(#7065,#7066,#7067,#7068));
#1156=EDGE_LOOP('',(#7069,#7070,#7071,#7072,#7073,#7074,#7075,#7076));
#1157=EDGE_LOOP('',(#7077,#7078,#7079,#7080));
#1158=EDGE_LOOP('',(#7081,#7082,#7083,#7084));
#1159=EDGE_LOOP('',(#7085,#7086,#7087,#7088));
#1160=EDGE_LOOP('',(#7089,#7090,#7091,#7092));
#1161=EDGE_LOOP('',(#7093,#7094,#7095,#7096));
#1162=EDGE_LOOP('',(#7097,#7098,#7099,#7100));
#1163=EDGE_LOOP('',(#7101,#7102,#7103,#7104));
#1164=EDGE_LOOP('',(#7105,#7106,#7107,#7108));
#1165=EDGE_LOOP('',(#7109,#7110,#7111,#7112));
#1166=EDGE_LOOP('',(#7113,#7114,#7115,#7116));
#1167=EDGE_LOOP('',(#7117,#7118,#7119,#7120));
#1168=EDGE_LOOP('',(#7121,#7122,#7123,#7124));
#1169=EDGE_LOOP('',(#7125,#7126,#7127,#7128));
#1170=EDGE_LOOP('',(#7129,#7130,#7131,#7132));
#1171=EDGE_LOOP('',(#7133,#7134,#7135,#7136));
#1172=EDGE_LOOP('',(#7137,#7138,#7139,#7140));
#1173=EDGE_LOOP('',(#7141,#7142,#7143,#7144));
#1174=EDGE_LOOP('',(#7145,#7146,#7147,#7148));
#1175=EDGE_LOOP('',(#7149,#7150,#7151,#7152));
#1176=EDGE_LOOP('',(#7153,#7154,#7155,#7156));
#1177=EDGE_LOOP('',(#7157,#7158,#7159,#7160));
#1178=EDGE_LOOP('',(#7161,#7162,#7163,#7164));
#1179=EDGE_LOOP('',(#7165,#7166,#7167,#7168));
#1180=EDGE_LOOP('',(#7169,#7170,#7171,#7172));
#1181=EDGE_LOOP('',(#7173,#7174,#7175,#7176,#7177,#7178,#7179,#7180));
#1182=EDGE_LOOP('',(#7181,#7182,#7183,#7184));
#1183=EDGE_LOOP('',(#7185,#7186,#7187,#7188));
#1184=EDGE_LOOP('',(#7189,#7190,#7191,#7192));
#1185=EDGE_LOOP('',(#7193,#7194,#7195,#7196));
#1186=EDGE_LOOP('',(#7197,#7198,#7199,#7200));
#1187=EDGE_LOOP('',(#7201,#7202,#7203,#7204));
#1188=EDGE_LOOP('',(#7205,#7206,#7207,#7208));
#1189=EDGE_LOOP('',(#7209,#7210,#7211,#7212));
#1190=EDGE_LOOP('',(#7213,#7214,#7215,#7216));
#1191=EDGE_LOOP('',(#7217,#7218,#7219,#7220));
#1192=EDGE_LOOP('',(#7221,#7222,#7223,#7224));
#1193=EDGE_LOOP('',(#7225,#7226,#7227,#7228));
#1194=EDGE_LOOP('',(#7229,#7230,#7231,#7232));
#1195=EDGE_LOOP('',(#7233,#7234,#7235,#7236));
#1196=EDGE_LOOP('',(#7237,#7238,#7239,#7240));
#1197=EDGE_LOOP('',(#7241,#7242,#7243,#7244));
#1198=EDGE_LOOP('',(#7245,#7246,#7247,#7248));
#1199=EDGE_LOOP('',(#7249,#7250,#7251,#7252));
#1200=EDGE_LOOP('',(#7253,#7254,#7255,#7256));
#1201=EDGE_LOOP('',(#7257,#7258,#7259,#7260));
#1202=EDGE_LOOP('',(#7261,#7262,#7263,#7264));
#1203=EDGE_LOOP('',(#7265,#7266,#7267,#7268));
#1204=EDGE_LOOP('',(#7269,#7270,#7271,#7272));
#1205=EDGE_LOOP('',(#7273,#7274,#7275,#7276));
#1206=EDGE_LOOP('',(#7277,#7278,#7279,#7280));
#1207=EDGE_LOOP('',(#7281));
#1208=EDGE_LOOP('',(#7282));
#1209=EDGE_LOOP('',(#7283,#7284,#7285,#7286));
#1210=EDGE_LOOP('',(#7287,#7288,#7289,#7290));
#1211=EDGE_LOOP('',(#7291));
#1212=EDGE_LOOP('',(#7292));
#1213=EDGE_LOOP('',(#7293,#7294,#7295,#7296));
#1214=EDGE_LOOP('',(#7297,#7298,#7299,#7300));
#1215=EDGE_LOOP('',(#7301,#7302,#7303,#7304));
#1216=EDGE_LOOP('',(#7305,#7306,#7307,#7308));
#1217=EDGE_LOOP('',(#7309,#7310,#7311,#7312,#7313,#7314,#7315,#7316,#7317,
#7318,#7319,#7320,#7321,#7322,#7323,#7324,#7325,#7326,#7327,#7328,#7329,
#7330,#7331,#7332,#7333,#7334,#7335,#7336,#7337,#7338));
#1218=EDGE_LOOP('',(#7339,#7340,#7341,#7342,#7343,#7344,#7345,#7346,#7347,
#7348,#7349,#7350,#7351,#7352,#7353,#7354,#7355,#7356,#7357,#7358,#7359,
#7360,#7361,#7362,#7363,#7364,#7365,#7366,#7367));
#1219=EDGE_LOOP('',(#7368,#7369,#7370,#7371));
#1220=EDGE_LOOP('',(#7372,#7373,#7374,#7375));
#1221=EDGE_LOOP('',(#7376,#7377,#7378,#7379));
#1222=EDGE_LOOP('',(#7380,#7381,#7382,#7383,#7384,#7385,#7386,#7387,#7388,
#7389,#7390,#7391,#7392,#7393,#7394,#7395,#7396,#7397,#7398,#7399,#7400,
#7401,#7402,#7403,#7404,#7405,#7406,#7407,#7408,#7409));
#1223=EDGE_LOOP('',(#7410,#7411,#7412,#7413,#7414,#7415,#7416,#7417,#7418,
#7419,#7420,#7421,#7422,#7423,#7424,#7425,#7426,#7427,#7428,#7429,#7430,
#7431,#7432,#7433,#7434,#7435,#7436,#7437,#7438));
#1224=EDGE_LOOP('',(#7439,#7440,#7441,#7442));
#1225=EDGE_LOOP('',(#7443,#7444,#7445,#7446));
#1226=EDGE_LOOP('',(#7447,#7448,#7449,#7450));
#1227=EDGE_LOOP('',(#7451,#7452,#7453,#7454,#7455,#7456,#7457,#7458,#7459,
#7460,#7461,#7462,#7463,#7464,#7465,#7466,#7467,#7468,#7469,#7470,#7471,
#7472,#7473,#7474,#7475,#7476,#7477,#7478,#7479,#7480));
#1228=EDGE_LOOP('',(#7481,#7482,#7483,#7484,#7485,#7486,#7487,#7488,#7489,
#7490,#7491,#7492,#7493,#7494,#7495,#7496,#7497,#7498,#7499,#7500,#7501,
#7502,#7503,#7504,#7505,#7506,#7507,#7508,#7509));
#1229=EDGE_LOOP('',(#7510,#7511,#7512,#7513));
#1230=EDGE_LOOP('',(#7514,#7515,#7516,#7517));
#1231=EDGE_LOOP('',(#7518,#7519,#7520,#7521));
#1232=EDGE_LOOP('',(#7522,#7523,#7524,#7525,#7526,#7527,#7528,#7529,#7530,
#7531,#7532,#7533,#7534,#7535,#7536,#7537,#7538,#7539,#7540,#7541,#7542,
#7543,#7544,#7545,#7546,#7547,#7548,#7549,#7550,#7551));
#1233=EDGE_LOOP('',(#7552,#7553,#7554,#7555,#7556,#7557,#7558,#7559,#7560,
#7561,#7562,#7563,#7564,#7565,#7566,#7567,#7568,#7569,#7570,#7571,#7572,
#7573,#7574,#7575,#7576,#7577,#7578,#7579,#7580));
#1234=EDGE_LOOP('',(#7581,#7582,#7583,#7584));
#1235=EDGE_LOOP('',(#7585));
#1236=EDGE_LOOP('',(#7586));
#1237=EDGE_LOOP('',(#7587));
#1238=EDGE_LOOP('',(#7588));
#1239=EDGE_LOOP('',(#7589,#7590,#7591,#7592));
#1240=EDGE_LOOP('',(#7593,#7594,#7595,#7596));
#1241=EDGE_LOOP('',(#7597,#7598,#7599,#7600));
#1242=EDGE_LOOP('',(#7601,#7602,#7603,#7604));
#1243=EDGE_LOOP('',(#7605,#7606,#7607,#7608));
#1244=EDGE_LOOP('',(#7609,#7610,#7611,#7612));
#1245=EDGE_LOOP('',(#7613));
#1246=EDGE_LOOP('',(#7614,#7615,#7616,#7617));
#1247=EDGE_LOOP('',(#7618,#7619,#7620,#7621));
#1248=EDGE_LOOP('',(#7622,#7623,#7624,#7625));
#1249=EDGE_LOOP('',(#7626,#7627,#7628,#7629));
#1250=EDGE_LOOP('',(#7630));
#1251=EDGE_LOOP('',(#7631,#7632,#7633,#7634));
#1252=EDGE_LOOP('',(#7635,#7636,#7637,#7638));
#1253=EDGE_LOOP('',(#7639));
#1254=EDGE_LOOP('',(#7640));
#1255=EDGE_LOOP('',(#7641,#7642,#7643,#7644,#7645,#7646,#7647,#7648));
#1256=EDGE_LOOP('',(#7649));
#1257=EDGE_LOOP('',(#7650));
#1258=EDGE_LOOP('',(#7651));
#1259=EDGE_LOOP('',(#7652,#7653,#7654,#7655));
#1260=EDGE_LOOP('',(#7656,#7657,#7658,#7659));
#1261=EDGE_LOOP('',(#7660,#7661,#7662,#7663));
#1262=EDGE_LOOP('',(#7664,#7665,#7666,#7667));
#1263=EDGE_LOOP('',(#7668,#7669,#7670,#7671));
#1264=EDGE_LOOP('',(#7672));
#1265=EDGE_LOOP('',(#7673,#7674,#7675,#7676));
#1266=EDGE_LOOP('',(#7677));
#1267=EDGE_LOOP('',(#7678,#7679,#7680,#7681));
#1268=EDGE_LOOP('',(#7682,#7683,#7684,#7685));
#1269=EDGE_LOOP('',(#7686,#7687,#7688,#7689));
#1270=EDGE_LOOP('',(#7690,#7691,#7692,#7693,#7694,#7695,#7696,#7697));
#1271=EDGE_LOOP('',(#7698,#7699,#7700,#7701));
#1272=EDGE_LOOP('',(#7702));
#1273=EDGE_LOOP('',(#7703,#7704,#7705,#7706,#7707,#7708,#7709,#7710));
#1274=EDGE_LOOP('',(#7711,#7712,#7713,#7714));
#1275=EDGE_LOOP('',(#7715,#7716,#7717,#7718));
#1276=EDGE_LOOP('',(#7719,#7720,#7721,#7722));
#1277=EDGE_LOOP('',(#7723,#7724,#7725,#7726));
#1278=EDGE_LOOP('',(#7727,#7728,#7729,#7730));
#1279=EDGE_LOOP('',(#7731,#7732,#7733,#7734,#7735,#7736,#7737,#7738));
#1280=EDGE_LOOP('',(#7739,#7740,#7741,#7742,#7743,#7744,#7745,#7746,#7747,
#7748,#7749,#7750));
#1281=EDGE_LOOP('',(#7751));
#1282=EDGE_LOOP('',(#7752));
#1283=EDGE_LOOP('',(#7753));
#1284=EDGE_LOOP('',(#7754));
#1285=EDGE_LOOP('',(#7755,#7756,#7757,#7758));
#1286=EDGE_LOOP('',(#7759,#7760,#7761,#7762));
#1287=EDGE_LOOP('',(#7763,#7764,#7765,#7766));
#1288=EDGE_LOOP('',(#7767,#7768,#7769,#7770));
#1289=EDGE_LOOP('',(#7771,#7772,#7773,#7774));
#1290=EDGE_LOOP('',(#7775,#7776,#7777,#7778));
#1291=EDGE_LOOP('',(#7779,#7780,#7781,#7782));
#1292=EDGE_LOOP('',(#7783,#7784,#7785,#7786));
#1293=EDGE_LOOP('',(#7787,#7788,#7789,#7790));
#1294=EDGE_LOOP('',(#7791,#7792,#7793,#7794));
#1295=EDGE_LOOP('',(#7795,#7796,#7797,#7798));
#1296=EDGE_LOOP('',(#7799,#7800,#7801,#7802));
#1297=EDGE_LOOP('',(#7803,#7804,#7805,#7806));
#1298=EDGE_LOOP('',(#7807,#7808,#7809,#7810));
#1299=EDGE_LOOP('',(#7811,#7812,#7813));
#1300=EDGE_LOOP('',(#7814,#7815,#7816));
#1301=EDGE_LOOP('',(#7817,#7818,#7819,#7820));
#1302=EDGE_LOOP('',(#7821,#7822,#7823,#7824));
#1303=EDGE_LOOP('',(#7825,#7826,#7827));
#1304=EDGE_LOOP('',(#7828,#7829,#7830,#7831));
#1305=EDGE_LOOP('',(#7832,#7833,#7834,#7835));
#1306=EDGE_LOOP('',(#7836,#7837,#7838));
#1307=EDGE_LOOP('',(#7839,#7840,#7841,#7842,#7843,#7844,#7845,#7846,#7847,
#7848,#7849,#7850));
#1308=EDGE_LOOP('',(#7851));
#1309=EDGE_LOOP('',(#7852,#7853));
#1310=EDGE_LOOP('',(#7854,#7855,#7856,#7857));
#1311=EDGE_LOOP('',(#7858,#7859,#7860,#7861,#7862,#7863,#7864,#7865,#7866,
#7867,#7868));
#1312=EDGE_LOOP('',(#7869,#7870,#7871,#7872,#7873,#7874,#7875,#7876,#7877,
#7878,#7879));
#1313=EDGE_LOOP('',(#7880,#7881,#7882,#7883));
#1314=EDGE_LOOP('',(#7884,#7885,#7886,#7887,#7888,#7889,#7890,#7891,#7892,
#7893,#7894));
#1315=EDGE_LOOP('',(#7895,#7896,#7897,#7898,#7899,#7900,#7901,#7902,#7903,
#7904,#7905));
#1316=EDGE_LOOP('',(#7906,#7907,#7908,#7909));
#1317=EDGE_LOOP('',(#7910,#7911,#7912,#7913));
#1318=EDGE_LOOP('',(#7914));
#1319=EDGE_LOOP('',(#7915,#7916,#7917,#7918));
#1320=EDGE_LOOP('',(#7919));
#1321=EDGE_LOOP('',(#7920));
#1322=EDGE_LOOP('',(#7921,#7922,#7923,#7924,#7925));
#1323=EDGE_LOOP('',(#7926,#7927,#7928,#7929,#7930,#7931,#7932,#7933,#7934,
#7935));
#1324=EDGE_LOOP('',(#7936,#7937));
#1325=EDGE_LOOP('',(#7938,#7939));
#1326=EDGE_LOOP('',(#7940,#7941,#7942,#7943));
#1327=EDGE_LOOP('',(#7944,#7945,#7946,#7947));
#1328=EDGE_LOOP('',(#7948));
#1329=EDGE_LOOP('',(#7949));
#1330=EDGE_LOOP('',(#7950));
#1331=EDGE_LOOP('',(#7951));
#1332=EDGE_LOOP('',(#7952,#7953,#7954,#7955,#7956,#7957,#7958,#7959));
#1333=EDGE_LOOP('',(#7960,#7961,#7962,#7963,#7964,#7965));
#1334=EDGE_LOOP('',(#7966,#7967,#7968,#7969));
#1335=EDGE_LOOP('',(#7970,#7971,#7972,#7973));
#1336=EDGE_LOOP('',(#7974));
#1337=EDGE_LOOP('',(#7975,#7976,#7977,#7978));
#1338=EDGE_LOOP('',(#7979));
#1339=EDGE_LOOP('',(#7980));
#1340=EDGE_LOOP('',(#7981,#7982,#7983,#7984,#7985,#7986,#7987));
#1341=EDGE_LOOP('',(#7988,#7989));
#1342=EDGE_LOOP('',(#7990,#7991,#7992,#7993));
#1343=EDGE_LOOP('',(#7994,#7995,#7996,#7997,#7998,#7999,#8000,#8001,#8002,
#8003));
#1344=EDGE_LOOP('',(#8004,#8005,#8006,#8007,#8008,#8009));
#1345=EDGE_LOOP('',(#8010,#8011,#8012,#8013));
#1346=EDGE_LOOP('',(#8014,#8015,#8016,#8017));
#1347=EDGE_LOOP('',(#8018,#8019,#8020,#8021));
#1348=EDGE_LOOP('',(#8022,#8023,#8024,#8025));
#1349=EDGE_LOOP('',(#8026,#8027,#8028,#8029,#8030,#8031,#8032,#8033,#8034,
#8035));
#1350=EDGE_LOOP('',(#8036,#8037));
#1351=EDGE_LOOP('',(#8038,#8039,#8040,#8041));
#1352=EDGE_LOOP('',(#8042,#8043,#8044,#8045));
#1353=EDGE_LOOP('',(#8046,#8047,#8048,#8049));
#1354=EDGE_LOOP('',(#8050,#8051,#8052,#8053));
#1355=EDGE_LOOP('',(#8054,#8055,#8056,#8057));
#1356=EDGE_LOOP('',(#8058));
#1357=EDGE_LOOP('',(#8059));
#1358=EDGE_LOOP('',(#8060));
#1359=EDGE_LOOP('',(#8061));
#1360=EDGE_LOOP('',(#8062));
#1361=EDGE_LOOP('',(#8063));
#1362=EDGE_LOOP('',(#8064));
#1363=EDGE_LOOP('',(#8065,#8066,#8067,#8068));
#1364=EDGE_LOOP('',(#8069));
#1365=EDGE_LOOP('',(#8070));
#1366=EDGE_LOOP('',(#8071,#8072,#8073,#8074));
#1367=EDGE_LOOP('',(#8075,#8076,#8077,#8078));
#1368=EDGE_LOOP('',(#8079));
#1369=EDGE_LOOP('',(#8080));
#1370=EDGE_LOOP('',(#8081,#8082,#8083,#8084,#8085,#8086,#8087,#8088));
#1371=EDGE_LOOP('',(#8089,#8090,#8091,#8092));
#1372=EDGE_LOOP('',(#8093,#8094,#8095,#8096));
#1373=EDGE_LOOP('',(#8097,#8098,#8099,#8100));
#1374=EDGE_LOOP('',(#8101,#8102,#8103,#8104));
#1375=EDGE_LOOP('',(#8105,#8106,#8107,#8108));
#1376=EDGE_LOOP('',(#8109,#8110,#8111,#8112));
#1377=EDGE_LOOP('',(#8113,#8114,#8115,#8116));
#1378=EDGE_LOOP('',(#8117,#8118,#8119,#8120));
#1379=EDGE_LOOP('',(#8121,#8122,#8123,#8124));
#1380=EDGE_LOOP('',(#8125,#8126,#8127,#8128));
#1381=EDGE_LOOP('',(#8129,#8130,#8131,#8132));
#1382=EDGE_LOOP('',(#8133,#8134,#8135,#8136));
#1383=EDGE_LOOP('',(#8137,#8138,#8139,#8140));
#1384=EDGE_LOOP('',(#8141,#8142,#8143,#8144));
#1385=EDGE_LOOP('',(#8145,#8146,#8147,#8148));
#1386=EDGE_LOOP('',(#8149,#8150,#8151,#8152));
#1387=EDGE_LOOP('',(#8153,#8154,#8155,#8156));
#1388=EDGE_LOOP('',(#8157,#8158,#8159,#8160));
#1389=EDGE_LOOP('',(#8161,#8162,#8163,#8164));
#1390=EDGE_LOOP('',(#8165,#8166,#8167,#8168));
#1391=EDGE_LOOP('',(#8169,#8170,#8171,#8172));
#1392=EDGE_LOOP('',(#8173,#8174,#8175,#8176));
#1393=EDGE_LOOP('',(#8177,#8178,#8179,#8180));
#1394=EDGE_LOOP('',(#8181,#8182,#8183,#8184));
#1395=EDGE_LOOP('',(#8185,#8186,#8187,#8188));
#1396=EDGE_LOOP('',(#8189,#8190,#8191,#8192));
#1397=EDGE_LOOP('',(#8193,#8194,#8195,#8196));
#1398=EDGE_LOOP('',(#8197,#8198,#8199,#8200));
#1399=EDGE_LOOP('',(#8201,#8202,#8203,#8204));
#1400=EDGE_LOOP('',(#8205,#8206,#8207,#8208));
#1401=EDGE_LOOP('',(#8209,#8210,#8211,#8212));
#1402=EDGE_LOOP('',(#8213,#8214,#8215,#8216));
#1403=EDGE_LOOP('',(#8217,#8218,#8219,#8220));
#1404=EDGE_LOOP('',(#8221,#8222,#8223,#8224));
#1405=EDGE_LOOP('',(#8225,#8226,#8227,#8228));
#1406=EDGE_LOOP('',(#8229,#8230,#8231,#8232));
#1407=EDGE_LOOP('',(#8233,#8234,#8235,#8236));
#1408=EDGE_LOOP('',(#8237,#8238,#8239,#8240));
#1409=EDGE_LOOP('',(#8241,#8242,#8243,#8244));
#1410=EDGE_LOOP('',(#8245,#8246,#8247,#8248));
#1411=EDGE_LOOP('',(#8249,#8250,#8251,#8252));
#1412=EDGE_LOOP('',(#8253,#8254,#8255,#8256));
#1413=EDGE_LOOP('',(#8257,#8258,#8259,#8260));
#1414=EDGE_LOOP('',(#8261,#8262,#8263,#8264));
#1415=EDGE_LOOP('',(#8265,#8266,#8267,#8268));
#1416=EDGE_LOOP('',(#8269,#8270,#8271,#8272));
#1417=EDGE_LOOP('',(#8273,#8274,#8275,#8276));
#1418=EDGE_LOOP('',(#8277,#8278,#8279,#8280));
#1419=EDGE_LOOP('',(#8281,#8282,#8283,#8284));
#1420=EDGE_LOOP('',(#8285,#8286,#8287,#8288));
#1421=EDGE_LOOP('',(#8289,#8290,#8291,#8292));
#1422=EDGE_LOOP('',(#8293,#8294,#8295,#8296));
#1423=EDGE_LOOP('',(#8297,#8298,#8299,#8300));
#1424=EDGE_LOOP('',(#8301,#8302,#8303,#8304));
#1425=EDGE_LOOP('',(#8305,#8306,#8307,#8308));
#1426=EDGE_LOOP('',(#8309,#8310,#8311,#8312));
#1427=EDGE_LOOP('',(#8313,#8314,#8315,#8316));
#1428=EDGE_LOOP('',(#8317,#8318,#8319,#8320,#8321,#8322,#8323,#8324,#8325,
#8326,#8327,#8328,#8329,#8330,#8331,#8332,#8333,#8334,#8335,#8336));
#1429=EDGE_LOOP('',(#8337,#8338,#8339,#8340,#8341,#8342,#8343,#8344,#8345,
#8346,#8347,#8348,#8349,#8350,#8351,#8352,#8353,#8354,#8355,#8356));
#1430=EDGE_LOOP('',(#8357,#8358,#8359,#8360,#8361,#8362));
#1431=EDGE_LOOP('',(#8363,#8364,#8365,#8366));
#1432=EDGE_LOOP('',(#8367,#8368,#8369,#8370));
#1433=EDGE_LOOP('',(#8371,#8372,#8373,#8374));
#1434=EDGE_LOOP('',(#8375,#8376,#8377,#8378,#8379,#8380,#8381,#8382,#8383,
#8384,#8385,#8386,#8387,#8388,#8389,#8390,#8391,#8392,#8393,#8394));
#1435=EDGE_LOOP('',(#8395,#8396,#8397,#8398,#8399,#8400,#8401,#8402,#8403,
#8404,#8405,#8406,#8407,#8408,#8409,#8410,#8411,#8412,#8413,#8414));
#1436=EDGE_LOOP('',(#8415,#8416,#8417,#8418));
#1437=EDGE_LOOP('',(#8419,#8420,#8421,#8422));
#1438=EDGE_LOOP('',(#8423,#8424,#8425,#8426));
#1439=EDGE_LOOP('',(#8427,#8428,#8429,#8430));
#1440=EDGE_LOOP('',(#8431,#8432,#8433,#8434,#8435,#8436,#8437,#8438,#8439,
#8440,#8441,#8442,#8443,#8444,#8445,#8446,#8447,#8448,#8449,#8450,#8451,
#8452,#8453,#8454,#8455,#8456,#8457,#8458,#8459,#8460));
#1441=EDGE_LOOP('',(#8461,#8462,#8463,#8464,#8465,#8466,#8467,#8468,#8469,
#8470,#8471,#8472,#8473,#8474,#8475,#8476,#8477,#8478,#8479,#8480,#8481,
#8482,#8483,#8484,#8485,#8486,#8487,#8488,#8489));
#1442=EDGE_LOOP('',(#8490,#8491,#8492,#8493));
#1443=EDGE_LOOP('',(#8494));
#1444=EDGE_LOOP('',(#8495,#8496,#8497,#8498));
#1445=EDGE_LOOP('',(#8499,#8500,#8501,#8502));
#1446=EDGE_LOOP('',(#8503,#8504,#8505,#8506));
#1447=EDGE_LOOP('',(#8507,#8508,#8509,#8510));
#1448=EDGE_LOOP('',(#8511));
#1449=EDGE_LOOP('',(#8512));
#1450=EDGE_LOOP('',(#8513));
#1451=EDGE_LOOP('',(#8514));
#1452=EDGE_LOOP('',(#8515,#8516,#8517,#8518));
#1453=EDGE_LOOP('',(#8519,#8520,#8521,#8522));
#1454=EDGE_LOOP('',(#8523,#8524,#8525,#8526));
#1455=EDGE_LOOP('',(#8527,#8528,#8529,#8530));
#1456=EDGE_LOOP('',(#8531,#8532,#8533,#8534));
#1457=EDGE_LOOP('',(#8535,#8536,#8537,#8538));
#1458=EDGE_LOOP('',(#8539,#8540,#8541,#8542));
#1459=EDGE_LOOP('',(#8543,#8544,#8545,#8546));
#1460=EDGE_LOOP('',(#8547,#8548,#8549,#8550));
#1461=EDGE_LOOP('',(#8551));
#1462=EDGE_LOOP('',(#8552,#8553,#8554,#8555));
#1463=EDGE_LOOP('',(#8556,#8557,#8558,#8559,#8560,#8561));
#1464=EDGE_LOOP('',(#8562,#8563,#8564,#8565));
#1465=EDGE_LOOP('',(#8566,#8567,#8568,#8569));
#1466=EDGE_LOOP('',(#8570));
#1467=EDGE_LOOP('',(#8571,#8572,#8573,#8574));
#1468=EDGE_LOOP('',(#8575,#8576,#8577,#8578));
#1469=EDGE_LOOP('',(#8579));
#1470=EDGE_LOOP('',(#8580));
#1471=EDGE_LOOP('',(#8581,#8582,#8583,#8584));
#1472=EDGE_LOOP('',(#8585));
#1473=EDGE_LOOP('',(#8586));
#1474=EDGE_LOOP('',(#8587));
#1475=EDGE_LOOP('',(#8588));
#1476=EDGE_LOOP('',(#8589,#8590,#8591,#8592));
#1477=EDGE_LOOP('',(#8593));
#1478=EDGE_LOOP('',(#8594));
#1479=EDGE_LOOP('',(#8595,#8596,#8597,#8598));
#1480=EDGE_LOOP('',(#8599,#8600,#8601,#8602));
#1481=EDGE_LOOP('',(#8603,#8604,#8605,#8606));
#1482=EDGE_LOOP('',(#8607));
#1483=EDGE_LOOP('',(#8608));
#1484=EDGE_LOOP('',(#8609,#8610,#8611,#8612));
#1485=EDGE_LOOP('',(#8613,#8614,#8615,#8616));
#1486=EDGE_LOOP('',(#8617,#8618,#8619,#8620));
#1487=EDGE_LOOP('',(#8621,#8622,#8623,#8624));
#1488=EDGE_LOOP('',(#8625,#8626,#8627,#8628));
#1489=EDGE_LOOP('',(#8629,#8630,#8631,#8632));
#1490=EDGE_LOOP('',(#8633,#8634,#8635,#8636));
#1491=EDGE_LOOP('',(#8637));
#1492=EDGE_LOOP('',(#8638));
#1493=EDGE_LOOP('',(#8639,#8640,#8641,#8642));
#1494=EDGE_LOOP('',(#8643));
#1495=EDGE_LOOP('',(#8644));
#1496=EDGE_LOOP('',(#8645,#8646,#8647,#8648));
#1497=EDGE_LOOP('',(#8649));
#1498=EDGE_LOOP('',(#8650));
#1499=EDGE_LOOP('',(#8651,#8652,#8653,#8654,#8655,#8656,#8657,#8658));
#1500=EDGE_LOOP('',(#8659,#8660,#8661,#8662));
#1501=EDGE_LOOP('',(#8663,#8664,#8665,#8666));
#1502=EDGE_LOOP('',(#8667,#8668,#8669,#8670));
#1503=EDGE_LOOP('',(#8671,#8672,#8673,#8674));
#1504=EDGE_LOOP('',(#8675,#8676,#8677,#8678));
#1505=EDGE_LOOP('',(#8679,#8680,#8681,#8682));
#1506=EDGE_LOOP('',(#8683,#8684,#8685,#8686));
#1507=EDGE_LOOP('',(#8687,#8688,#8689,#8690));
#1508=EDGE_LOOP('',(#8691,#8692,#8693,#8694));
#1509=EDGE_LOOP('',(#8695,#8696,#8697,#8698));
#1510=EDGE_LOOP('',(#8699,#8700,#8701,#8702));
#1511=EDGE_LOOP('',(#8703,#8704,#8705,#8706));
#1512=EDGE_LOOP('',(#8707,#8708,#8709,#8710));
#1513=EDGE_LOOP('',(#8711,#8712,#8713,#8714));
#1514=EDGE_LOOP('',(#8715,#8716,#8717,#8718));
#1515=EDGE_LOOP('',(#8719,#8720,#8721,#8722));
#1516=EDGE_LOOP('',(#8723,#8724,#8725,#8726));
#1517=EDGE_LOOP('',(#8727,#8728,#8729,#8730));
#1518=EDGE_LOOP('',(#8731,#8732,#8733,#8734));
#1519=EDGE_LOOP('',(#8735,#8736,#8737,#8738));
#1520=EDGE_LOOP('',(#8739,#8740,#8741,#8742));
#1521=EDGE_LOOP('',(#8743,#8744,#8745,#8746));
#1522=EDGE_LOOP('',(#8747,#8748,#8749,#8750));
#1523=EDGE_LOOP('',(#8751,#8752,#8753,#8754));
#1524=EDGE_LOOP('',(#8755,#8756,#8757,#8758,#8759,#8760,#8761,#8762));
#1525=EDGE_LOOP('',(#8763,#8764,#8765,#8766));
#1526=EDGE_LOOP('',(#8767,#8768,#8769,#8770));
#1527=EDGE_LOOP('',(#8771,#8772,#8773,#8774));
#1528=EDGE_LOOP('',(#8775,#8776,#8777,#8778));
#1529=EDGE_LOOP('',(#8779,#8780,#8781,#8782));
#1530=EDGE_LOOP('',(#8783,#8784,#8785,#8786));
#1531=EDGE_LOOP('',(#8787,#8788,#8789,#8790));
#1532=EDGE_LOOP('',(#8791,#8792,#8793,#8794));
#1533=EDGE_LOOP('',(#8795,#8796,#8797,#8798));
#1534=EDGE_LOOP('',(#8799,#8800,#8801,#8802));
#1535=EDGE_LOOP('',(#8803,#8804,#8805,#8806));
#1536=EDGE_LOOP('',(#8807,#8808,#8809,#8810));
#1537=EDGE_LOOP('',(#8811,#8812,#8813,#8814));
#1538=EDGE_LOOP('',(#8815,#8816,#8817,#8818));
#1539=EDGE_LOOP('',(#8819,#8820,#8821,#8822));
#1540=EDGE_LOOP('',(#8823,#8824,#8825,#8826));
#1541=EDGE_LOOP('',(#8827,#8828,#8829,#8830));
#1542=EDGE_LOOP('',(#8831,#8832,#8833,#8834));
#1543=EDGE_LOOP('',(#8835,#8836,#8837,#8838));
#1544=EDGE_LOOP('',(#8839,#8840,#8841,#8842));
#1545=EDGE_LOOP('',(#8843,#8844,#8845,#8846));
#1546=EDGE_LOOP('',(#8847,#8848,#8849,#8850));
#1547=EDGE_LOOP('',(#8851,#8852,#8853,#8854));
#1548=EDGE_LOOP('',(#8855,#8856,#8857,#8858));
#1549=EDGE_LOOP('',(#8859,#8860,#8861,#8862));
#1550=EDGE_LOOP('',(#8863,#8864,#8865,#8866));
#1551=EDGE_LOOP('',(#8867,#8868,#8869,#8870));
#1552=EDGE_LOOP('',(#8871,#8872,#8873,#8874));
#1553=EDGE_LOOP('',(#8875,#8876,#8877,#8878));
#1554=EDGE_LOOP('',(#8879,#8880,#8881,#8882));
#1555=EDGE_LOOP('',(#8883,#8884,#8885,#8886));
#1556=EDGE_LOOP('',(#8887,#8888,#8889,#8890));
#1557=EDGE_LOOP('',(#8891,#8892,#8893,#8894));
#1558=EDGE_LOOP('',(#8895,#8896,#8897,#8898));
#1559=EDGE_LOOP('',(#8899,#8900,#8901,#8902));
#1560=EDGE_LOOP('',(#8903,#8904,#8905,#8906,#8907));
#1561=EDGE_LOOP('',(#8908,#8909,#8910,#8911));
#1562=EDGE_LOOP('',(#8912,#8913,#8914,#8915,#8916,#8917,#8918,#8919,#8920,
#8921,#8922,#8923,#8924,#8925,#8926,#8927,#8928,#8929,#8930,#8931,#8932,
#8933,#8934,#8935,#8936,#8937,#8938,#8939,#8940,#8941,#8942,#8943,#8944,
#8945,#8946,#8947,#8948,#8949,#8950,#8951));
#1563=EDGE_LOOP('',(#8952,#8953,#8954,#8955,#8956,#8957,#8958,#8959,#8960,
#8961,#8962,#8963,#8964,#8965,#8966,#8967,#8968,#8969,#8970,#8971,#8972,
#8973,#8974,#8975,#8976,#8977,#8978,#8979,#8980,#8981,#8982,#8983,#8984,
#8985,#8986,#8987,#8988,#8989,#8990,#8991));
#1564=EDGE_LOOP('',(#8992,#8993,#8994,#8995));
#1565=EDGE_LOOP('',(#8996));
#1566=EDGE_LOOP('',(#8997,#8998,#8999,#9000));
#1567=EDGE_LOOP('',(#9001,#9002,#9003,#9004));
#1568=EDGE_LOOP('',(#9005,#9006,#9007,#9008,#9009,#9010,#9011,#9012,#9013,
#9014,#9015,#9016,#9017,#9018,#9019,#9020,#9021,#9022,#9023,#9024,#9025,
#9026,#9027,#9028,#9029,#9030,#9031,#9032,#9033,#9034));
#1569=EDGE_LOOP('',(#9035,#9036,#9037,#9038,#9039,#9040,#9041,#9042,#9043,
#9044,#9045,#9046,#9047,#9048,#9049,#9050,#9051,#9052,#9053,#9054,#9055,
#9056,#9057,#9058,#9059,#9060,#9061,#9062,#9063));
#1570=EDGE_LOOP('',(#9064,#9065,#9066,#9067));
#1571=EDGE_LOOP('',(#9068));
#1572=EDGE_LOOP('',(#9069,#9070,#9071,#9072));
#1573=EDGE_LOOP('',(#9073,#9074,#9075,#9076));
#1574=EDGE_LOOP('',(#9077,#9078,#9079,#9080));
#1575=EDGE_LOOP('',(#9081,#9082,#9083,#9084));
#1576=EDGE_LOOP('',(#9085,#9086,#9087,#9088));
#1577=EDGE_LOOP('',(#9089,#9090,#9091,#9092));
#1578=EDGE_LOOP('',(#9093,#9094,#9095,#9096));
#1579=EDGE_LOOP('',(#9097,#9098,#9099,#9100));
#1580=EDGE_LOOP('',(#9101,#9102,#9103,#9104,#9105,#9106,#9107,#9108));
#1581=EDGE_LOOP('',(#9109,#9110,#9111,#9112));
#1582=EDGE_LOOP('',(#9113,#9114,#9115,#9116));
#1583=EDGE_LOOP('',(#9117,#9118,#9119,#9120));
#1584=EDGE_LOOP('',(#9121,#9122,#9123,#9124));
#1585=EDGE_LOOP('',(#9125,#9126,#9127,#9128));
#1586=EDGE_LOOP('',(#9129,#9130,#9131,#9132));
#1587=EDGE_LOOP('',(#9133,#9134,#9135,#9136));
#1588=EDGE_LOOP('',(#9137,#9138,#9139,#9140));
#1589=EDGE_LOOP('',(#9141,#9142,#9143,#9144));
#1590=EDGE_LOOP('',(#9145,#9146,#9147,#9148));
#1591=EDGE_LOOP('',(#9149,#9150,#9151,#9152));
#1592=EDGE_LOOP('',(#9153,#9154,#9155,#9156));
#1593=EDGE_LOOP('',(#9157,#9158,#9159,#9160));
#1594=EDGE_LOOP('',(#9161,#9162,#9163,#9164));
#1595=EDGE_LOOP('',(#9165,#9166,#9167,#9168));
#1596=EDGE_LOOP('',(#9169,#9170,#9171,#9172));
#1597=EDGE_LOOP('',(#9173,#9174,#9175,#9176));
#1598=EDGE_LOOP('',(#9177,#9178,#9179,#9180));
#1599=EDGE_LOOP('',(#9181,#9182,#9183,#9184));
#1600=EDGE_LOOP('',(#9185,#9186,#9187,#9188,#9189));
#1601=EDGE_LOOP('',(#9190,#9191,#9192,#9193));
#1602=EDGE_LOOP('',(#9194,#9195,#9196,#9197,#9198,#9199,#9200,#9201,#9202,
#9203,#9204,#9205,#9206,#9207,#9208,#9209,#9210,#9211,#9212,#9213,#9214,
#9215,#9216,#9217));
#1603=EDGE_LOOP('',(#9218,#9219,#9220,#9221,#9222,#9223,#9224,#9225,#9226,
#9227,#9228,#9229,#9230,#9231,#9232,#9233,#9234,#9235,#9236,#9237,#9238,
#9239,#9240,#9241));
#1604=EDGE_LOOP('',(#9242,#9243,#9244,#9245));
#1605=EDGE_LOOP('',(#9246));
#1606=EDGE_LOOP('',(#9247,#9248,#9249,#9250));
#1607=EDGE_LOOP('',(#9251,#9252,#9253,#9254));
#1608=EDGE_LOOP('',(#9255,#9256,#9257,#9258));
#1609=EDGE_LOOP('',(#9259));
#1610=EDGE_LOOP('',(#9260,#9261,#9262,#9263,#9264,#9265));
#1611=EDGE_LOOP('',(#9266,#9267,#9268,#9269));
#1612=EDGE_LOOP('',(#9270,#9271,#9272,#9273,#9274,#9275));
#1613=EDGE_LOOP('',(#9276,#9277,#9278,#9279));
#1614=EDGE_LOOP('',(#9280,#9281,#9282,#9283));
#1615=EDGE_LOOP('',(#9284,#9285,#9286,#9287));
#1616=EDGE_LOOP('',(#9288));
#1617=EDGE_LOOP('',(#9289,#9290,#9291,#9292));
#1618=EDGE_LOOP('',(#9293,#9294,#9295,#9296));
#1619=EDGE_LOOP('',(#9297,#9298,#9299,#9300));
#1620=EDGE_LOOP('',(#9301,#9302,#9303,#9304));
#1621=EDGE_LOOP('',(#9305,#9306,#9307,#9308));
#1622=EDGE_LOOP('',(#9309,#9310,#9311,#9312));
#1623=EDGE_LOOP('',(#9313,#9314,#9315,#9316));
#1624=EDGE_LOOP('',(#9317));
#1625=EDGE_LOOP('',(#9318,#9319,#9320,#9321));
#1626=EDGE_LOOP('',(#9322));
#1627=EDGE_LOOP('',(#9323,#9324));
#1628=EDGE_LOOP('',(#9325));
#1629=EDGE_LOOP('',(#9326));
#1630=EDGE_LOOP('',(#9327,#9328,#9329,#9330));
#1631=EDGE_LOOP('',(#9331));
#1632=EDGE_LOOP('',(#9332,#9333,#9334,#9335));
#1633=EDGE_LOOP('',(#9336));
#1634=EDGE_LOOP('',(#9337,#9338,#9339,#9340));
#1635=EDGE_LOOP('',(#9341));
#1636=EDGE_LOOP('',(#9342));
#1637=EDGE_LOOP('',(#9343,#9344,#9345,#9346));
#1638=EDGE_LOOP('',(#9347,#9348,#9349,#9350));
#1639=EDGE_LOOP('',(#9351,#9352,#9353,#9354));
#1640=EDGE_LOOP('',(#9355,#9356,#9357,#9358));
#1641=EDGE_LOOP('',(#9359,#9360,#9361,#9362));
#1642=EDGE_LOOP('',(#9363,#9364,#9365,#9366));
#1643=EDGE_LOOP('',(#9367,#9368,#9369,#9370));
#1644=EDGE_LOOP('',(#9371,#9372,#9373,#9374));
#1645=EDGE_LOOP('',(#9375,#9376,#9377,#9378));
#1646=EDGE_LOOP('',(#9379,#9380,#9381,#9382));
#1647=EDGE_LOOP('',(#9383,#9384,#9385,#9386));
#1648=EDGE_LOOP('',(#9387,#9388,#9389,#9390));
#1649=EDGE_LOOP('',(#9391,#9392,#9393,#9394));
#1650=EDGE_LOOP('',(#9395,#9396,#9397,#9398));
#1651=EDGE_LOOP('',(#9399,#9400,#9401,#9402));
#1652=EDGE_LOOP('',(#9403,#9404,#9405,#9406));
#1653=EDGE_LOOP('',(#9407,#9408,#9409,#9410));
#1654=EDGE_LOOP('',(#9411,#9412,#9413,#9414));
#1655=EDGE_LOOP('',(#9415,#9416,#9417,#9418));
#1656=EDGE_LOOP('',(#9419,#9420,#9421,#9422));
#1657=EDGE_LOOP('',(#9423,#9424,#9425,#9426));
#1658=EDGE_LOOP('',(#9427,#9428,#9429,#9430));
#1659=EDGE_LOOP('',(#9431,#9432,#9433,#9434));
#1660=EDGE_LOOP('',(#9435,#9436,#9437,#9438));
#1661=EDGE_LOOP('',(#9439,#9440,#9441,#9442));
#1662=EDGE_LOOP('',(#9443,#9444,#9445,#9446));
#1663=EDGE_LOOP('',(#9447,#9448,#9449,#9450));
#1664=EDGE_LOOP('',(#9451,#9452,#9453,#9454));
#1665=EDGE_LOOP('',(#9455,#9456,#9457,#9458));
#1666=EDGE_LOOP('',(#9459,#9460,#9461,#9462));
#1667=EDGE_LOOP('',(#9463,#9464,#9465,#9466));
#1668=EDGE_LOOP('',(#9467,#9468,#9469,#9470));
#1669=EDGE_LOOP('',(#9471,#9472,#9473,#9474,#9475,#9476,#9477,#9478));
#1670=EDGE_LOOP('',(#9479,#9480,#9481,#9482,#9483,#9484,#9485,#9486,#9487,
#9488,#9489,#9490,#9491,#9492,#9493,#9494,#9495,#9496,#9497,#9498,#9499,
#9500,#9501,#9502,#9503,#9504,#9505,#9506,#9507,#9508,#9509,#9510,#9511,
#9512,#9513,#9514));
#1671=EDGE_LOOP('',(#9515,#9516,#9517,#9518));
#1672=EDGE_LOOP('',(#9519,#9520,#9521,#9522,#9523,#9524,#9525,#9526,#9527,
#9528,#9529,#9530,#9531,#9532,#9533,#9534,#9535,#9536,#9537,#9538,#9539,
#9540,#9541,#9542,#9543,#9544,#9545,#9546,#9547,#9548,#9549,#9550,#9551,
#9552,#9553,#9554,#9555));
#1673=EDGE_LOOP('',(#9556,#9557,#9558,#9559));
#1674=EDGE_LOOP('',(#9560,#9561,#9562,#9563));
#1675=EDGE_LOOP('',(#9564,#9565,#9566,#9567));
#1676=EDGE_LOOP('',(#9568,#9569,#9570,#9571));
#1677=EDGE_LOOP('',(#9572,#9573,#9574,#9575));
#1678=EDGE_LOOP('',(#9576,#9577,#9578,#9579));
#1679=EDGE_LOOP('',(#9580,#9581,#9582,#9583));
#1680=EDGE_LOOP('',(#9584,#9585,#9586,#9587,#9588,#9589));
#1681=EDGE_LOOP('',(#9590));
#1682=EDGE_LOOP('',(#9591,#9592,#9593,#9594));
#1683=EDGE_LOOP('',(#9595,#9596,#9597,#9598));
#1684=EDGE_LOOP('',(#9599));
#1685=EDGE_LOOP('',(#9600,#9601,#9602,#9603,#9604,#9605));
#1686=EDGE_LOOP('',(#9606));
#1687=EDGE_LOOP('',(#9607,#9608,#9609,#9610));
#1688=EDGE_LOOP('',(#9611,#9612,#9613,#9614));
#1689=EDGE_LOOP('',(#9615,#9616,#9617,#9618));
#1690=EDGE_LOOP('',(#9619,#9620,#9621,#9622));
#1691=EDGE_LOOP('',(#9623,#9624,#9625,#9626));
#1692=EDGE_LOOP('',(#9627,#9628,#9629,#9630));
#1693=EDGE_LOOP('',(#9631,#9632,#9633,#9634));
#1694=EDGE_LOOP('',(#9635,#9636,#9637,#9638));
#1695=EDGE_LOOP('',(#9639,#9640,#9641,#9642));
#1696=EDGE_LOOP('',(#9643,#9644,#9645,#9646));
#1697=EDGE_LOOP('',(#9647,#9648,#9649,#9650));
#1698=EDGE_LOOP('',(#9651,#9652,#9653,#9654));
#1699=EDGE_LOOP('',(#9655,#9656,#9657,#9658));
#1700=EDGE_LOOP('',(#9659,#9660,#9661,#9662));
#1701=EDGE_LOOP('',(#9663,#9664,#9665,#9666));
#1702=EDGE_LOOP('',(#9667,#9668,#9669,#9670));
#1703=EDGE_LOOP('',(#9671,#9672,#9673,#9674));
#1704=EDGE_LOOP('',(#9675,#9676,#9677,#9678));
#1705=EDGE_LOOP('',(#9679,#9680,#9681,#9682));
#1706=EDGE_LOOP('',(#9683,#9684,#9685,#9686));
#1707=EDGE_LOOP('',(#9687,#9688,#9689,#9690,#9691,#9692,#9693,#9694));
#1708=EDGE_LOOP('',(#9695,#9696,#9697,#9698,#9699,#9700,#9701,#9702,#9703,
#9704,#9705,#9706,#9707,#9708,#9709,#9710,#9711,#9712,#9713,#9714,#9715,
#9716,#9717,#9718));
#1709=EDGE_LOOP('',(#9719,#9720,#9721,#9722));
#1710=EDGE_LOOP('',(#9723,#9724,#9725,#9726,#9727,#9728,#9729,#9730,#9731,
#9732,#9733,#9734,#9735,#9736,#9737,#9738,#9739,#9740,#9741,#9742,#9743,
#9744,#9745,#9746,#9747));
#1711=EDGE_LOOP('',(#9748,#9749,#9750,#9751));
#1712=EDGE_LOOP('',(#9752,#9753,#9754,#9755));
#1713=EDGE_LOOP('',(#9756,#9757,#9758,#9759));
#1714=EDGE_LOOP('',(#9760,#9761,#9762,#9763));
#1715=EDGE_LOOP('',(#9764,#9765,#9766,#9767));
#1716=EDGE_LOOP('',(#9768,#9769,#9770,#9771));
#1717=EDGE_LOOP('',(#9772,#9773,#9774,#9775));
#1718=EDGE_LOOP('',(#9776,#9777,#9778,#9779,#9780,#9781));
#1719=EDGE_LOOP('',(#9782));
#1720=EDGE_LOOP('',(#9783,#9784,#9785,#9786));
#1721=EDGE_LOOP('',(#9787,#9788,#9789,#9790));
#1722=EDGE_LOOP('',(#9791));
#1723=EDGE_LOOP('',(#9792,#9793,#9794,#9795,#9796,#9797));
#1724=EDGE_LOOP('',(#9798));
#1725=EDGE_LOOP('',(#9799,#9800,#9801,#9802));
#1726=EDGE_LOOP('',(#9803,#9804,#9805,#9806));
#1727=EDGE_LOOP('',(#9807,#9808,#9809,#9810));
#1728=EDGE_LOOP('',(#9811,#9812,#9813,#9814));
#1729=EDGE_LOOP('',(#9815,#9816,#9817,#9818));
#1730=EDGE_LOOP('',(#9819,#9820,#9821,#9822));
#1731=EDGE_LOOP('',(#9823,#9824,#9825,#9826));
#1732=EDGE_LOOP('',(#9827,#9828,#9829,#9830));
#1733=EDGE_LOOP('',(#9831,#9832,#9833,#9834));
#1734=EDGE_LOOP('',(#9835,#9836,#9837,#9838));
#1735=EDGE_LOOP('',(#9839,#9840,#9841,#9842));
#1736=EDGE_LOOP('',(#9843,#9844,#9845,#9846));
#1737=EDGE_LOOP('',(#9847,#9848,#9849,#9850));
#1738=EDGE_LOOP('',(#9851,#9852,#9853,#9854));
#1739=EDGE_LOOP('',(#9855,#9856,#9857,#9858));
#1740=EDGE_LOOP('',(#9859,#9860,#9861,#9862));
#1741=EDGE_LOOP('',(#9863,#9864,#9865,#9866));
#1742=EDGE_LOOP('',(#9867,#9868,#9869,#9870));
#1743=EDGE_LOOP('',(#9871,#9872,#9873,#9874));
#1744=EDGE_LOOP('',(#9875,#9876,#9877,#9878));
#1745=EDGE_LOOP('',(#9879,#9880,#9881,#9882));
#1746=EDGE_LOOP('',(#9883,#9884,#9885,#9886));
#1747=EDGE_LOOP('',(#9887,#9888,#9889,#9890));
#1748=EDGE_LOOP('',(#9891,#9892,#9893,#9894));
#1749=EDGE_LOOP('',(#9895,#9896,#9897,#9898));
#1750=EDGE_LOOP('',(#9899,#9900,#9901,#9902));
#1751=EDGE_LOOP('',(#9903,#9904,#9905,#9906));
#1752=EDGE_LOOP('',(#9907,#9908,#9909,#9910));
#1753=EDGE_LOOP('',(#9911,#9912,#9913,#9914));
#1754=EDGE_LOOP('',(#9915,#9916,#9917,#9918));
#1755=EDGE_LOOP('',(#9919,#9920,#9921,#9922));
#1756=EDGE_LOOP('',(#9923,#9924,#9925,#9926));
#1757=EDGE_LOOP('',(#9927,#9928,#9929,#9930));
#1758=EDGE_LOOP('',(#9931,#9932,#9933,#9934));
#1759=EDGE_LOOP('',(#9935,#9936,#9937,#9938));
#1760=EDGE_LOOP('',(#9939,#9940,#9941,#9942));
#1761=EDGE_LOOP('',(#9943,#9944,#9945,#9946,#9947,#9948,#9949,#9950));
#1762=EDGE_LOOP('',(#9951,#9952,#9953,#9954,#9955,#9956,#9957,#9958,#9959,
#9960,#9961,#9962,#9963,#9964,#9965,#9966,#9967,#9968,#9969,#9970,#9971,
#9972,#9973,#9974,#9975,#9976,#9977,#9978,#9979,#9980,#9981,#9982,#9983,
#9984,#9985,#9986,#9987,#9988,#9989,#9990));
#1763=EDGE_LOOP('',(#9991,#9992,#9993,#9994));
#1764=EDGE_LOOP('',(#9995,#9996,#9997,#9998,#9999,#10000,#10001,#10002,
#10003,#10004,#10005,#10006,#10007,#10008,#10009,#10010,#10011,#10012,#10013,
#10014,#10015,#10016,#10017,#10018,#10019,#10020,#10021,#10022,#10023,#10024,
#10025,#10026,#10027,#10028,#10029,#10030,#10031,#10032,#10033,#10034,#10035));
#1765=EDGE_LOOP('',(#10036,#10037,#10038,#10039));
#1766=EDGE_LOOP('',(#10040,#10041,#10042,#10043));
#1767=EDGE_LOOP('',(#10044,#10045,#10046,#10047));
#1768=EDGE_LOOP('',(#10048,#10049,#10050,#10051));
#1769=EDGE_LOOP('',(#10052,#10053,#10054,#10055));
#1770=EDGE_LOOP('',(#10056,#10057,#10058,#10059));
#1771=EDGE_LOOP('',(#10060,#10061,#10062,#10063));
#1772=EDGE_LOOP('',(#10064,#10065,#10066,#10067,#10068,#10069));
#1773=EDGE_LOOP('',(#10070));
#1774=EDGE_LOOP('',(#10071,#10072,#10073,#10074));
#1775=EDGE_LOOP('',(#10075,#10076,#10077,#10078));
#1776=EDGE_LOOP('',(#10079));
#1777=EDGE_LOOP('',(#10080,#10081,#10082,#10083,#10084,#10085));
#1778=EDGE_LOOP('',(#10086));
#1779=EDGE_LOOP('',(#10087,#10088,#10089,#10090));
#1780=EDGE_LOOP('',(#10091,#10092,#10093,#10094));
#1781=EDGE_LOOP('',(#10095,#10096,#10097,#10098));
#1782=EDGE_LOOP('',(#10099,#10100,#10101,#10102));
#1783=EDGE_LOOP('',(#10103,#10104,#10105,#10106,#10107,#10108,#10109,#10110));
#1784=EDGE_LOOP('',(#10111,#10112,#10113,#10114,#10115,#10116,#10117,#10118));
#1785=EDGE_LOOP('',(#10119,#10120,#10121,#10122));
#1786=EDGE_LOOP('',(#10123,#10124,#10125,#10126,#10127,#10128,#10129,#10130,
#10131));
#1787=EDGE_LOOP('',(#10132,#10133,#10134,#10135));
#1788=EDGE_LOOP('',(#10136,#10137,#10138,#10139));
#1789=EDGE_LOOP('',(#10140,#10141,#10142,#10143));
#1790=EDGE_LOOP('',(#10144,#10145,#10146,#10147));
#1791=EDGE_LOOP('',(#10148,#10149,#10150,#10151));
#1792=EDGE_LOOP('',(#10152,#10153,#10154,#10155));
#1793=EDGE_LOOP('',(#10156,#10157,#10158,#10159));
#1794=EDGE_LOOP('',(#10160,#10161,#10162,#10163,#10164,#10165));
#1795=EDGE_LOOP('',(#10166));
#1796=EDGE_LOOP('',(#10167,#10168,#10169,#10170));
#1797=EDGE_LOOP('',(#10171,#10172,#10173,#10174));
#1798=EDGE_LOOP('',(#10175));
#1799=EDGE_LOOP('',(#10176,#10177,#10178,#10179,#10180,#10181));
#1800=EDGE_LOOP('',(#10182));
#1801=CIRCLE('',#11439,0.1666);
#1802=CIRCLE('',#11440,0.1666);
#1803=CIRCLE('',#11452,0.1666);
#1804=CIRCLE('',#11454,0.205475000000001);
#1805=CIRCLE('',#11467,0.205475000000001);
#1806=CIRCLE('',#11469,0.1666);
#1807=CIRCLE('',#11470,0.1666);
#1808=CIRCLE('',#11482,0.1666);
#1809=CIRCLE('',#11484,0.205475000000001);
#1810=CIRCLE('',#11497,0.205475000000001);
#1811=CIRCLE('',#11499,0.1666);
#1812=CIRCLE('',#11500,0.1666);
#1813=CIRCLE('',#11512,0.1666);
#1814=CIRCLE('',#11514,0.205475);
#1815=CIRCLE('',#11527,0.205475);
#1816=CIRCLE('',#11529,0.1666);
#1817=CIRCLE('',#11530,0.1666);
#1818=CIRCLE('',#11542,0.1666);
#1819=CIRCLE('',#11544,0.205475);
#1820=CIRCLE('',#11557,0.205475);
#1821=CIRCLE('',#11559,0.6);
#1822=CIRCLE('',#11560,0.6);
#1823=CIRCLE('',#11562,0.4);
#1824=CIRCLE('',#11563,0.25);
#1825=CIRCLE('',#11565,0.4);
#1826=CIRCLE('',#11567,0.25);
#1827=CIRCLE('',#11569,0.4);
#1828=CIRCLE('',#11570,0.25);
#1829=CIRCLE('',#11572,0.4);
#1830=CIRCLE('',#11574,0.25);
#1831=CIRCLE('',#11592,0.3);
#1832=CIRCLE('',#11593,0.3);
#1833=CIRCLE('',#11595,0.3);
#1834=CIRCLE('',#11596,0.3);
#1835=CIRCLE('',#11606,0.65);
#1836=CIRCLE('',#11607,0.65);
#1837=CIRCLE('',#11609,0.8);
#1838=CIRCLE('',#11610,0.8);
#1839=CIRCLE('',#11613,0.2);
#1840=CIRCLE('',#11614,0.2);
#1841=CIRCLE('',#11615,0.2);
#1842=CIRCLE('',#11616,0.2);
#1843=CIRCLE('',#11618,0.2);
#1844=CIRCLE('',#11621,0.2);
#1845=CIRCLE('',#11624,0.2);
#1846=CIRCLE('',#11628,0.2);
#1847=CIRCLE('',#11638,0.4263);
#1848=CIRCLE('',#11641,0.4263);
#1849=CIRCLE('',#11643,0.4263);
#1850=CIRCLE('',#11646,0.4263);
#1851=CIRCLE('',#11648,0.5099);
#1852=CIRCLE('',#11652,0.5099);
#1853=CIRCLE('',#11654,0.5099);
#1854=CIRCLE('',#11658,0.5099);
#1855=CIRCLE('',#11660,0.7);
#1856=CIRCLE('',#11662,0.7);
#1857=CIRCLE('',#11666,0.7);
#1858=CIRCLE('',#11670,0.7);
#1859=CIRCLE('',#11672,2.4);
#1860=CIRCLE('',#11673,2.4);
#1861=CIRCLE('',#11674,0.6);
#1862=CIRCLE('',#11676,0.7);
#1863=CIRCLE('',#11681,0.4);
#1864=CIRCLE('',#11683,0.4);
#1865=CIRCLE('',#11685,0.2);
#1866=CIRCLE('',#11688,0.7);
#1867=CIRCLE('',#11689,0.7);
#1868=CIRCLE('',#11693,0.25);
#1869=CIRCLE('',#11694,0.25);
#1870=CIRCLE('',#11695,0.25);
#1871=CIRCLE('',#11696,0.25);
#1872=CIRCLE('',#11697,2.4);
#1873=CIRCLE('',#11698,2.4);
#1874=CIRCLE('',#11702,0.4);
#1875=CIRCLE('',#11704,0.4);
#1876=CIRCLE('',#11706,0.2);
#1877=CIRCLE('',#11709,0.7);
#1878=CIRCLE('',#11713,0.25);
#1879=CIRCLE('',#11715,0.25);
#1880=CIRCLE('',#11717,0.25);
#1881=CIRCLE('',#11719,0.25);
#1882=CIRCLE('',#11721,0.6);
#1883=CIRCLE('',#11729,0.8);
#1884=CIRCLE('',#11730,0.6);
#1885=CIRCLE('',#11732,0.8);
#1886=CIRCLE('',#11734,0.4);
#1887=CIRCLE('',#11736,0.4);
#1888=CIRCLE('',#11738,0.6);
#1889=CIRCLE('',#11742,0.1666);
#1890=CIRCLE('',#11743,0.1666);
#1891=CIRCLE('',#11755,0.1666);
#1892=CIRCLE('',#11757,0.205475);
#1893=CIRCLE('',#11770,0.205475);
#1894=CIRCLE('',#11772,0.12645);
#1895=CIRCLE('',#11780,0.12645);
#1896=CIRCLE('',#11782,0.12645);
#1897=CIRCLE('',#11790,0.12645);
#1898=CIRCLE('',#11792,0.1543);
#1899=CIRCLE('',#11800,0.1543);
#1900=CIRCLE('',#11802,0.1543);
#1901=CIRCLE('',#11810,0.1543);
#1902=CIRCLE('',#11813,1.);
#1903=CIRCLE('',#11822,0.6);
#1904=CIRCLE('',#11823,0.399999999999998);
#1905=CIRCLE('',#11824,0.6);
#1906=CIRCLE('',#11826,0.6);
#1907=CIRCLE('',#11828,0.4);
#1908=CIRCLE('',#11829,0.6);
#1909=CIRCLE('',#11831,0.6);
#1910=CIRCLE('',#11833,1.);
#1911=CIRCLE('',#11834,0.6);
#1912=CIRCLE('',#11836,1.);
#1913=CIRCLE('',#11837,0.6);
#1914=CIRCLE('',#11846,1.);
#1915=CIRCLE('',#11848,0.6);
#1916=CIRCLE('',#11853,2.);
#1917=CIRCLE('',#11854,0.2);
#1918=CIRCLE('',#11855,2.2);
#1919=CIRCLE('',#11857,2.2);
#1920=CIRCLE('',#11859,0.4);
#1921=CIRCLE('',#11861,0.2);
#1922=CIRCLE('',#11862,2.);
#1923=CIRCLE('',#11864,1.);
#1924=CIRCLE('',#11866,0.4);
#1925=CIRCLE('',#11867,0.25);
#1926=CIRCLE('',#11870,0.6);
#1927=CIRCLE('',#11871,0.25);
#1928=CIRCLE('',#11874,0.6);
#1929=CIRCLE('',#11876,1.);
#1930=CIRCLE('',#11880,0.2);
#1931=CIRCLE('',#11881,0.2);
#1932=CIRCLE('',#11883,0.2);
#1933=CIRCLE('',#11884,0.2);
#1934=CIRCLE('',#11892,0.05);
#1935=CIRCLE('',#11893,0.05);
#1936=CIRCLE('',#11898,0.1666);
#1937=CIRCLE('',#11899,0.1666);
#1938=CIRCLE('',#11911,0.1666);
#1939=CIRCLE('',#11913,0.205475);
#1940=CIRCLE('',#11926,0.205475);
#1941=CIRCLE('',#11928,0.12645);
#1942=CIRCLE('',#11929,0.12645);
#1943=CIRCLE('',#11930,0.12645);
#1944=CIRCLE('',#11948,0.12645);
#1945=CIRCLE('',#11950,0.1543);
#1946=CIRCLE('',#11968,0.1543);
#1947=CIRCLE('',#11985,0.12645);
#1948=CIRCLE('',#11986,0.12645);
#1949=CIRCLE('',#11987,0.12645);
#1950=CIRCLE('',#11997,0.12645);
#1951=CIRCLE('',#11999,0.1543);
#1952=CIRCLE('',#12009,0.1543);
#1953=CIRCLE('',#12015,0.2);
#1954=CIRCLE('',#12016,0.2);
#1955=CIRCLE('',#12027,0.2);
#1956=CIRCLE('',#12028,0.2);
#1957=CIRCLE('',#12037,0.2);
#1958=CIRCLE('',#12040,0.35);
#1959=CIRCLE('',#12041,0.2);
#1960=CIRCLE('',#12043,0.35);
#1961=CIRCLE('',#12046,0.2);
#1962=CIRCLE('',#12049,0.05);
#1963=CIRCLE('',#12050,0.05);
#1964=CIRCLE('',#12055,0.1954);
#1965=CIRCLE('',#12072,0.15555);
#1966=CIRCLE('',#12089,0.1954);
#1967=CIRCLE('',#12090,0.1);
#1968=CIRCLE('',#12092,0.15555);
#1969=CIRCLE('',#12102,0.35);
#1970=CIRCLE('',#12104,0.35);
#1971=CIRCLE('',#12109,0.14635);
#1972=CIRCLE('',#12120,0.117775);
#1973=CIRCLE('',#12131,0.14635);
#1974=CIRCLE('',#12132,0.05);
#1975=CIRCLE('',#12134,0.117775);
#1976=CIRCLE('',#12144,0.3);
#1977=CIRCLE('',#12146,0.3);
#1978=CIRCLE('',#12151,0.14635);
#1979=CIRCLE('',#12170,0.117775);
#1980=CIRCLE('',#12189,0.14635);
#1981=CIRCLE('',#12190,0.05);
#1982=CIRCLE('',#12192,0.117775);
#1983=CIRCLE('',#12202,0.3);
#1984=CIRCLE('',#12204,0.3);
#1985=CIRCLE('',#12209,0.4925);
#1986=CIRCLE('',#12212,0.40705);
#1987=CIRCLE('',#12215,0.4925);
#1988=CIRCLE('',#12216,0.4);
#1989=CIRCLE('',#12218,0.40705);
#1990=CIRCLE('',#12228,0.6);
#1991=CIRCLE('',#12230,0.6);
#1992=B_SPLINE_CURVE_WITH_KNOTS('',3,(#14568,#14569,#14570,#14571,#14572,
#14573,#14574,#14575,#14576,#14577,#14578,#14579,#14580,#14581,#14582,#14583,
#14584,#14585,#14586,#14587,#14588,#14589),.UNSPECIFIED.,.F.,.F.,(4,3,3,
3,3,3,3,4),(76.7080459413271,76.812995719686,77.8105670926689,78.8081384656519,
79.8057098386348,80.8032812116178,81.8008525846007,82.7984239575837),
 .UNSPECIFIED.);
#1993=B_SPLINE_CURVE_WITH_KNOTS('',3,(#14593,#14594,#14595,#14596,#14597,
#14598,#14599),.UNSPECIFIED.,.F.,.F.,(4,3,4),(-80.7838110923091,-79.8057098386348,
-79.2446069498473),.UNSPECIFIED.);
#1994=B_SPLINE_CURVE_WITH_KNOTS('',3,(#14603,#14604,#14605,#14606,#14607,
#14608,#14609,#14610,#14611,#14612,#14613,#14614,#14615,#14616,#14617,#14618,
#14619,#14620,#14621,#14622,#14623,#14624),.UNSPECIFIED.,.F.,.F.,(4,3,3,
3,3,3,3,4),(-79.2446069498473,-78.8081384656519,-77.8105670926689,-76.812995719686,
-75.815424346703,-74.8178529737201,-73.8202816007372,-72.9614216426678),
 .UNSPECIFIED.);
#1995=B_SPLINE_CURVE_WITH_KNOTS('',3,(#14629,#14630,#14631,#14632,#14633,
#14634,#14635,#14636,#14637,#14638,#14639,#14640,#14641,#14642,#14643,#14644,
#14645,#14646,#14647,#14648,#14649,#14650),.UNSPECIFIED.,.F.,.F.,(4,3,3,
3,3,3,3,4),(70.4248606341475,70.8275674817883,71.8251388547713,72.8227102277543,
73.8202816007372,74.8178529737201,75.815424346703,76.7080459413271),
 .UNSPECIFIED.);
#1996=B_SPLINE_CURVE_WITH_KNOTS('',3,(#14651,#14652,#14653,#14654,#14655,
#14656,#14657,#14658,#14659,#14660,#14661,#14662,#14663,#14664,#14665,#14666,
#14667,#14668,#14669,#14670,#14671,#14672,#14673,#14674,#14675),
 .UNSPECIFIED.,.F.,.F.,(4,3,3,3,3,3,3,3,4),(-72.9614216426678,-72.8227102277542,
-71.8251388547713,-70.8275674817884,-69.8299961088054,-68.8324247358225,
-67.8348533628396,-66.8372819898566,-66.6782363354882),.UNSPECIFIED.);
#1997=B_SPLINE_CURVE_WITH_KNOTS('',3,(#14680,#14681,#14682,#14683,#14684,
#14685,#14686,#14687,#14688,#14689,#14690,#14691,#14692,#14693,#14694,#14695,
#14696,#14697,#14698,#14699,#14700,#14701),.UNSPECIFIED.,.F.,.F.,(4,3,3,
3,3,3,3,4),(64.1416753269678,64.8421392438907,65.8397106168737,66.8372819898566,
67.8348533628396,68.8324247358225,69.8299961088054,70.4248606341475),
 .UNSPECIFIED.);
#1998=B_SPLINE_CURVE_WITH_KNOTS('',3,(#14702,#14703,#14704,#14705,#14706,
#14707,#14708,#14709,#14710,#14711,#14712,#14713,#14714,#14715,#14716,#14717,
#14718,#14719,#14720,#14721,#14722,#14723),.UNSPECIFIED.,.F.,.F.,(4,3,3,
3,3,3,3,4),(-66.6782363354882,-65.8397106168737,-64.8421392438908,-63.8445678709078,
-62.8469964979249,-61.849425124942,-60.851853751959,-60.3950510283085),
 .UNSPECIFIED.);
#1999=B_SPLINE_CURVE_WITH_KNOTS('',3,(#14728,#14729,#14730,#14731,#14732,
#14733,#14734,#14735,#14736,#14737,#14738,#14739,#14740,#14741,#14742,#14743,
#14744,#14745,#14746,#14747,#14748,#14749),.UNSPECIFIED.,.F.,.F.,(4,3,3,
3,3,3,3,4),(57.8584900197882,58.8567110059931,59.8542823789761,60.851853751959,
61.849425124942,62.8469964979249,63.8445678709078,64.1416753269678),
 .UNSPECIFIED.);
#2000=B_SPLINE_CURVE_WITH_KNOTS('',3,(#14750,#14751,#14752,#14753,#14754,
#14755,#14756,#14757,#14758,#14759,#14760,#14761,#14762,#14763,#14764,#14765,
#14766,#14767,#14768,#14769,#14770,#14771),.UNSPECIFIED.,.F.,.F.,(4,3,3,
3,3,3,3,4),(-60.3950510283085,-59.8542823789761,-58.8567110059932,-57.8591396330102,
-56.8615682600273,-55.8639968870443,-54.8664255140614,-54.1118657211289),
 .UNSPECIFIED.);
#2001=B_SPLINE_CURVE_WITH_KNOTS('',3,(#14776,#14777,#14778,#14779,#14780,
#14781,#14782,#14783,#14784,#14785,#14786,#14787,#14788,#14789,#14790,#14791,
#14792,#14793,#14794,#14795,#14796,#14797),.UNSPECIFIED.,.F.,.F.,(4,3,3,
3,3,3,3,4),(51.5753047126086,51.8737113951126,52.8712827680955,53.8688541410785,
54.8664255140614,55.8639968870444,56.8615682600273,57.8584900197882),
 .UNSPECIFIED.);
#2002=B_SPLINE_CURVE_WITH_KNOTS('',3,(#14798,#14799,#14800,#14801,#14802,
#14803,#14804,#14805,#14806,#14807,#14808,#14809,#14810,#14811,#14812,#14813,
#14814,#14815,#14816,#14817,#14818,#14819,#14820,#14821,#14822),
 .UNSPECIFIED.,.F.,.F.,(4,3,3,3,3,3,3,3,4),(-54.1118657211289,-53.8688541410785,
-52.8712827680955,-51.8737113951126,-50.8761400221297,-49.8785686491467,
-48.8809972761638,-47.8834259031809,-47.8286804139493),.UNSPECIFIED.);
#2003=B_SPLINE_CURVE_WITH_KNOTS('',3,(#14827,#14828,#14829,#14830,#14831,
#14832,#14833,#14834,#14835,#14836,#14837,#14838,#14839,#14840,#14841,#14842,
#14843,#14844,#14845,#14846,#14847,#14848),.UNSPECIFIED.,.F.,.F.,(4,3,3,
3,3,3,3,4),(45.2921194054291,45.888283157215,46.8858545301979,47.8834259031809,
48.8809972761638,49.8785686491467,50.8761400221297,51.5753047126086),
 .UNSPECIFIED.);
#2004=B_SPLINE_CURVE_WITH_KNOTS('',3,(#14849,#14850,#14851,#14852,#14853,
#14854,#14855,#14856,#14857,#14858,#14859,#14860,#14861,#14862,#14863,#14864,
#14865,#14866,#14867,#14868,#14869,#14870),.UNSPECIFIED.,.F.,.F.,(4,3,3,
3,3,3,3,4),(-47.8286804139493,-46.8858545301979,-45.888283157215,-44.8907117842321,
-43.8931404112491,-42.8955690382662,-41.8979976652833,-41.5454951067698),
 .UNSPECIFIED.);
#2005=B_SPLINE_CURVE_WITH_KNOTS('',3,(#14875,#14876,#14877,#14878,#14879,
#14880,#14881,#14882,#14883,#14884,#14885,#14886,#14887,#14888,#14889,#14890,
#14891,#14892,#14893,#14894,#14895,#14896),.UNSPECIFIED.,.F.,.F.,(4,3,3,
3,3,3,3,4),(39.0089340982495,39.9028549193174,40.9004262923003,41.8979976652833,
42.8955690382662,43.8931404112491,44.8907117842321,45.2921194054291),
 .UNSPECIFIED.);
#2006=B_SPLINE_CURVE_WITH_KNOTS('',3,(#14897,#14898,#14899,#14900,#14901,
#14902,#14903,#14904,#14905,#14906,#14907,#14908,#14909,#14910,#14911,#14912,
#14913,#14914,#14915,#14916,#14917,#14918),.UNSPECIFIED.,.F.,.F.,(4,3,3,
3,3,3,3,4),(-41.5454951067698,-40.9004262923003,-39.9028549193174,-38.9052835463345,
-37.9077121733515,-36.9101408003686,-35.9125694273856,-35.2623097995902),
 .UNSPECIFIED.);
#2007=B_SPLINE_CURVE_WITH_KNOTS('',3,(#14923,#14924,#14925,#14926,#14927,
#14928,#14929,#14930,#14931,#14932,#14933,#14934,#14935,#14936,#14937,#14938,
#14939,#14940,#14941,#14942,#14943,#14944,#14945,#14946,#14947),
 .UNSPECIFIED.,.F.,.F.,(4,3,3,3,3,3,3,3,4),(32.7257487910699,32.9198553084368,
33.9174266814198,34.9149980544027,35.9125694273856,36.9101408003686,37.9077121733515,
38.9052835463345,39.0089340982495),.UNSPECIFIED.);
#2008=B_SPLINE_CURVE_WITH_KNOTS('',3,(#14948,#14949,#14950,#14951,#14952,
#14953,#14954,#14955,#14956,#14957,#14958,#14959,#14960,#14961,#14962,#14963,
#14964,#14965,#14966,#14967,#14968,#14969),.UNSPECIFIED.,.F.,.F.,(4,3,3,
3,3,3,3,4),(-35.2623097995902,-34.9149980544027,-33.9174266814198,-32.9198553084368,
-31.9222839354539,-30.924712562471,-29.927141189488,-28.9791244924106),
 .UNSPECIFIED.);
#2009=B_SPLINE_CURVE_WITH_KNOTS('',3,(#14974,#14975,#14976,#14977,#14978,
#14979,#14980,#14981,#14982,#14983,#14984,#14985,#14986,#14987,#14988,#14989,
#14990,#14991,#14992,#14993,#14994,#14995),.UNSPECIFIED.,.F.,.F.,(4,3,3,
3,3,3,3,4),(26.4425634838903,26.9344270705392,27.9319984435222,28.9295698165051,
29.927141189488,30.924712562471,31.9222839354539,32.7257487910699),
 .UNSPECIFIED.);
#2010=B_SPLINE_CURVE_WITH_KNOTS('',3,(#14996,#14997,#14998,#14999,#15000,
#15001,#15002,#15003,#15004,#15005,#15006,#15007,#15008,#15009,#15010,#15011,
#15012,#15013,#15014,#15015,#15016,#15017,#15018,#15019,#15020),
 .UNSPECIFIED.,.F.,.F.,(4,3,3,3,3,3,3,3,4),(-28.9791244924106,-28.9295698165051,
-27.9319984435222,-26.9344270705392,-25.9368556975563,-24.9392843245734,
-23.9417129515904,-22.9441415786075,-22.695939185231),.UNSPECIFIED.);
#2011=B_SPLINE_CURVE_WITH_KNOTS('',3,(#15025,#15026,#15027,#15028,#15029,
#15030,#15031,#15032,#15033,#15034,#15035,#15036,#15037,#15038,#15039,#15040,
#15041,#15042,#15043,#15044,#15045,#15046),.UNSPECIFIED.,.F.,.F.,(4,3,3,
3,3,3,3,4),(20.1593781767107,20.9489988326416,21.9465702056246,22.9441415786075,
23.9417129515904,24.9392843245734,25.9368556975563,26.4425634838903),
 .UNSPECIFIED.);
#2012=B_SPLINE_CURVE_WITH_KNOTS('',3,(#15047,#15048,#15049,#15050,#15051,
#15052,#15053,#15054,#15055,#15056,#15057,#15058,#15059,#15060,#15061,#15062,
#15063,#15064,#15065,#15066,#15067,#15068),.UNSPECIFIED.,.F.,.F.,(4,3,3,
3,3,3,3,4),(-22.695939185231,-21.9465702056246,-20.9489988326416,-19.9514274596587,
-18.9538560866758,-17.9562847136928,-16.9587133407099,-16.4127538780514),
 .UNSPECIFIED.);
#2013=B_SPLINE_CURVE_WITH_KNOTS('',3,(#15073,#15074,#15075,#15076,#15077,
#15078,#15079,#15080,#15081,#15082,#15083,#15084,#15085,#15086,#15087,#15088,
#15089,#15090,#15091,#15092,#15093,#15094,#15095,#15096,#15097),
 .UNSPECIFIED.,.F.,.F.,(4,3,3,3,3,3,3,3,4),(13.8761928695311,13.9659992217611,
14.963570594744,15.961141967727,16.9587133407099,17.9562847136928,18.9538560866758,
19.9514274596587,20.1593781767107),.UNSPECIFIED.);
#2014=B_SPLINE_CURVE_WITH_KNOTS('',3,(#15098,#15099,#15100,#15101,#15102,
#15103,#15104,#15105,#15106,#15107,#15108,#15109,#15110,#15111,#15112,#15113,
#15114,#15115,#15116,#15117,#15118,#15119),.UNSPECIFIED.,.F.,.F.,(4,3,3,
3,3,3,3,4),(-16.4127538780514,-15.9611419677269,-14.963570594744,-13.9659992217611,
-12.9684278487781,-11.9708564757952,-10.9732851028123,-10.1295685708718),
 .UNSPECIFIED.);
#2015=B_SPLINE_CURVE_WITH_KNOTS('',3,(#15125,#15126,#15127,#15128,#15129,
#15130,#15131,#15132,#15133,#15134,#15135,#15136,#15137),.UNSPECIFIED.,
 .F.,.F.,(4,3,3,3,4),(-3.84638326369226,-2.9927141189488,-1.99514274596587,
-0.997571372982931,0.),.UNSPECIFIED.);
#2016=B_SPLINE_CURVE_WITH_KNOTS('',3,(#15140,#15141,#15142,#15143,#15144,
#15145,#15146,#15147,#15148,#15149,#15150,#15151,#15152,#15153,#15154,#15155,
#15156,#15157,#15158),.UNSPECIFIED.,.F.,.F.,(4,3,3,3,3,3,4),(2.01461286527457,
2.9927141189488,3.99028549193174,4.98785686491468,5.98542823789761,6.98299961088054,
7.59300756235157),.UNSPECIFIED.);
#2017=B_SPLINE_CURVE_WITH_KNOTS('',3,(#15164,#15165,#15166,#15167,#15168,
#15169,#15170),.UNSPECIFIED.,.F.,.F.,(4,1,1,1,4),(91.106186954104,91.6672898428915,
92.6648612158744,93.6624325888573,94.6600039618403),.UNSPECIFIED.);
#2018=B_SPLINE_CURVE_WITH_KNOTS('',3,(#15173,#15174,#15175,#15176,#15177,
#15178,#15179,#15180),.UNSPECIFIED.,.F.,.F.,(4,1,1,1,1,4),(91.106186954104,
91.2111367324629,92.2087081054458,93.2062794784288,94.2038508514117,95.181952105086),
 .UNSPECIFIED.);
#2019=B_SPLINE_CURVE_WITH_KNOTS('',3,(#15185,#15186,#15187,#15188,#15189,
#15190,#15191,#15192,#15193,#15194),.UNSPECIFIED.,.F.,.F.,(4,1,1,1,1,1,
1,4),(84.8230016469244,85.6818616049939,86.6794329779768,87.6770043509597,
88.6745757239427,89.6721470969256,90.6697184699085,91.106186954104),
 .UNSPECIFIED.);
#2020=B_SPLINE_CURVE_WITH_KNOTS('',3,(#15195,#15196,#15197,#15198,#15199,
#15200,#15201,#15202,#15203,#15204),.UNSPECIFIED.,.F.,.F.,(4,1,1,1,1,1,
1,4),(84.8230016469244,85.2257084945653,86.2232798675482,87.2208512405312,
88.2184226135141,89.215993986497,90.21356535948,91.106186954104),
 .UNSPECIFIED.);
#2021=B_SPLINE_CURVE_WITH_KNOTS('',3,(#15209,#15210,#15211,#15212,#15213,
#15214,#15215,#15216,#15217,#15218,#15219),.UNSPECIFIED.,.F.,.F.,(4,1,1,
1,1,1,1,1,4),(78.5398163397448,78.6988619941133,79.6964333670962,80.6940047400792,
81.6915761130621,82.689147486045,83.686718859028,84.6842902320109,84.8230016469244),
 .UNSPECIFIED.);
#2022=B_SPLINE_CURVE_WITH_KNOTS('',3,(#15220,#15221,#15222,#15223,#15224,
#15225,#15226,#15227,#15228,#15229),.UNSPECIFIED.,.F.,.F.,(4,1,1,1,1,1,
1,4),(78.5398163397448,79.2402802566677,80.2378516296506,81.2354230026336,
82.2329943756165,83.2305657485994,84.2281371215823,84.8230016469244),
 .UNSPECIFIED.);
#2023=B_SPLINE_CURVE_WITH_KNOTS('',3,(#15234,#15235,#15236,#15237,#15238,
#15239,#15240,#15241,#15242,#15243),.UNSPECIFIED.,.F.,.F.,(4,1,1,1,1,1,
1,4),(72.2566310325652,72.7134337562157,73.7110051291986,74.7085765021816,
75.7061478751645,76.7037192481474,77.7012906211304,78.5398163397448),
 .UNSPECIFIED.);
#2024=B_SPLINE_CURVE_WITH_KNOTS('',3,(#15244,#15245,#15246,#15247,#15248,
#15249,#15250,#15251,#15252,#15253,#15254),.UNSPECIFIED.,.F.,.F.,(4,1,1,
1,1,1,1,1,4),(72.2566310325652,72.2572806457871,73.2548520187701,74.252423391753,
75.2499947647359,76.2475661377189,77.2451375107018,78.2427088836847,78.5398163397448),
 .UNSPECIFIED.);
#2025=B_SPLINE_CURVE_WITH_KNOTS('',3,(#15259,#15260,#15261,#15262,#15263,
#15264,#15265,#15266,#15267,#15268),.UNSPECIFIED.,.F.,.F.,(4,1,1,1,1,1,
1,4),(65.9734457253856,66.7280055183181,67.725576891301,68.723148264284,
69.7207196372669,70.7182910102498,71.7158623832328,72.2566310325652),
 .UNSPECIFIED.);
#2026=B_SPLINE_CURVE_WITH_KNOTS('',3,(#15269,#15270,#15271,#15272,#15273,
#15274,#15275,#15276,#15277,#15278),.UNSPECIFIED.,.F.,.F.,(4,1,1,1,1,1,
1,4),(65.9734457253856,66.2718524078895,67.2694237808725,68.2669951538554,
69.2645665268383,70.2621378998213,71.2597092728042,72.2566310325652),
 .UNSPECIFIED.);
#2027=B_SPLINE_CURVE_WITH_KNOTS('',3,(#15283,#15284,#15285,#15286,#15287,
#15288,#15289,#15290,#15291,#15292,#15293),.UNSPECIFIED.,.F.,.F.,(4,1,1,
1,1,1,1,1,4),(59.690260418206,59.7450059074375,60.7425772804205,61.7401486534034,
62.7377200263864,63.7352913993693,64.7328627723522,65.7304341453352,65.9734457253856),
 .UNSPECIFIED.);
#2028=B_SPLINE_CURVE_WITH_KNOTS('',3,(#15294,#15295,#15296,#15297,#15298,
#15299,#15300,#15301,#15302,#15303),.UNSPECIFIED.,.F.,.F.,(4,1,1,1,1,1,
1,4),(59.690260418206,60.2864241699919,61.2839955429748,62.2815669159578,
63.2791382889407,64.2767096619237,65.2742810349066,65.9734457253856),
 .UNSPECIFIED.);
#2029=B_SPLINE_CURVE_WITH_KNOTS('',3,(#15308,#15309,#15310,#15311,#15312,
#15313,#15314,#15315,#15316,#15317),.UNSPECIFIED.,.F.,.F.,(4,1,1,1,1,1,
1,4),(53.4070751110264,53.7595776695399,54.7571490425229,55.7547204155058,
56.7522917884887,57.7498631614717,58.7474345344546,59.690260418206),
 .UNSPECIFIED.);
#2030=B_SPLINE_CURVE_WITH_KNOTS('',3,(#15318,#15319,#15320,#15321,#15322,
#15323,#15324,#15325,#15326,#15327),.UNSPECIFIED.,.F.,.F.,(4,1,1,1,1,1,
1,4),(53.4070751110264,54.3009959320943,55.2985673050772,56.2961386780602,
57.2937100510431,58.291281424026,59.288852797009,59.690260418206),
 .UNSPECIFIED.);
#2031=B_SPLINE_CURVE_WITH_KNOTS('',3,(#15332,#15333,#15334,#15335,#15336,
#15337,#15338,#15339,#15340,#15341),.UNSPECIFIED.,.F.,.F.,(4,1,1,1,1,1,
1,4),(47.1238898038469,47.7741494316423,48.7717208046253,49.7692921776082,
50.7668635505911,51.7644349235741,52.762006296557,53.4070751110264),
 .UNSPECIFIED.);
#2032=B_SPLINE_CURVE_WITH_KNOTS('',3,(#15342,#15343,#15344,#15345,#15346,
#15347,#15348,#15349,#15350,#15351,#15352),.UNSPECIFIED.,.F.,.F.,(4,1,1,
1,1,1,1,1,4),(47.1238898038469,47.3179963212138,48.3155676941967,49.3131390671796,
50.3107104401626,51.3082818131455,52.3058531861284,53.3034245591114,53.4070751110264),
 .UNSPECIFIED.);
#2033=B_SPLINE_CURVE_WITH_KNOTS('',3,(#15357,#15358,#15359,#15360,#15361,
#15362,#15363,#15364,#15365,#15366),.UNSPECIFIED.,.F.,.F.,(4,1,1,1,1,1,
1,4),(40.8407044966673,41.7887211937447,42.7862925667277,43.7838639397106,
44.7814353126935,45.7790066856765,46.7765780586594,47.1238898038469),
 .UNSPECIFIED.);
#2034=B_SPLINE_CURVE_WITH_KNOTS('',3,(#15367,#15368,#15369,#15370,#15371,
#15372,#15373,#15374,#15375,#15376),.UNSPECIFIED.,.F.,.F.,(4,1,1,1,1,1,
1,4),(40.8407044966673,41.3325680833162,42.3301394562991,43.327710829282,
44.325282202265,45.3228535752479,46.3204249482308,47.1238898038469),
 .UNSPECIFIED.);
#2035=B_SPLINE_CURVE_WITH_KNOTS('',3,(#15381,#15382,#15383,#15384,#15385,
#15386,#15387,#15388,#15389,#15390,#15391),.UNSPECIFIED.,.F.,.F.,(4,1,1,
1,1,1,1,1,4),(34.5575191894876,34.8057215828642,35.8032929558471,36.80086432883,
37.798435701813,38.7960070747959,39.7935784477789,40.7911498207618,40.8407044966673),
 .UNSPECIFIED.);
#2036=B_SPLINE_CURVE_WITH_KNOTS('',3,(#15392,#15393,#15394,#15395,#15396,
#15397,#15398,#15399,#15400,#15401),.UNSPECIFIED.,.F.,.F.,(4,1,1,1,1,1,
1,4),(34.5575191894876,35.3471398454185,36.3447112184015,37.3422825913844,
38.3398539643674,39.3374253373503,40.3349967103332,40.8407044966673),
 .UNSPECIFIED.);
#2037=B_SPLINE_CURVE_WITH_KNOTS('',3,(#15406,#15407,#15408,#15409,#15410,
#15411,#15412,#15413,#15414,#15415),.UNSPECIFIED.,.F.,.F.,(4,1,1,1,1,1,
1,4),(28.2743338823081,28.8202933449666,29.8178647179495,30.8154360909324,
31.8130074639154,32.8105788368983,33.8081502098812,34.5575191894876),
 .UNSPECIFIED.);
#2038=B_SPLINE_CURVE_WITH_KNOTS('',3,(#15416,#15417,#15418,#15419,#15420,
#15421,#15422,#15423,#15424,#15425,#15426),.UNSPECIFIED.,.F.,.F.,(4,1,1,
1,1,1,1,1,4),(28.2743338823081,28.364140234538,29.3617116075209,30.3592829805039,
31.3568543534868,32.3544257264697,33.3519970994527,34.3495684724356,34.5575191894876),
 .UNSPECIFIED.);
#2039=B_SPLINE_CURVE_WITH_KNOTS('',3,(#15431,#15432,#15433,#15434,#15435,
#15436,#15437,#15438,#15439,#15440),.UNSPECIFIED.,.F.,.F.,(4,1,1,1,1,1,
1,4),(21.9911485751285,22.834865107069,23.8324364800519,24.8300078530348,
25.8275792260178,26.8251505990007,27.8227219719836,28.2743338823081),
 .UNSPECIFIED.);
#2040=B_SPLINE_CURVE_WITH_KNOTS('',3,(#15441,#15442,#15443,#15444,#15445,
#15446,#15447,#15448,#15449,#15450),.UNSPECIFIED.,.F.,.F.,(4,1,1,1,1,1,
1,4),(21.9911485751285,22.3787119966404,23.3762833696233,24.3738547426063,
25.3714261155892,26.3689974885721,27.3665688615551,28.2743338823081),
 .UNSPECIFIED.);
#2041=B_SPLINE_CURVE_WITH_KNOTS('',3,(#15456,#15457,#15458,#15459,#15460),
 .UNSPECIFIED.,.F.,.F.,(4,1,4),(14.3981410127769,15.3957123857599,15.7079632679489),
 .UNSPECIFIED.);
#2042=B_SPLINE_CURVE_WITH_KNOTS('',3,(#15463,#15464,#15465,#15466,#15467),
 .UNSPECIFIED.,.F.,.F.,(4,1,4),(13.8761928695312,14.8542941232055,15.7079632679489),
 .UNSPECIFIED.);
#2043=B_SPLINE_CURVE_WITH_KNOTS('',3,(#15473,#15474,#15475,#15476,#15477,
#15478,#15479,#15480,#15481,#15482,#15483,#15484,#15485,#15486,#15487,#15488,
#15489,#15490,#15491,#15492,#15493,#15494),.UNSPECIFIED.,.F.,.F.,(4,3,3,
3,3,3,3,4),(76.7080459413271,76.8129957196859,77.8105670926688,78.8081384656517,
79.8057098386347,80.8032812116176,81.8008525846006,82.7984239575835),
 .UNSPECIFIED.);
#2044=B_SPLINE_CURVE_WITH_KNOTS('',3,(#15498,#15499,#15500,#15501,#15502,
#15503,#15504),.UNSPECIFIED.,.F.,.F.,(4,3,4),(-80.783811092309,-79.8057098386347,
-79.2446069498473),.UNSPECIFIED.);
#2045=B_SPLINE_CURVE_WITH_KNOTS('',3,(#15508,#15509,#15510,#15511,#15512,
#15513,#15514,#15515,#15516,#15517,#15518,#15519,#15520,#15521,#15522,#15523,
#15524,#15525,#15526,#15527,#15528,#15529),.UNSPECIFIED.,.F.,.F.,(4,3,3,
3,3,3,3,4),(-79.2446069498473,-78.8081384656518,-77.8105670926688,-76.8129957196859,
-75.815424346703,-74.81785297372,-73.8202816007371,-72.9614216426678),
 .UNSPECIFIED.);
#2046=B_SPLINE_CURVE_WITH_KNOTS('',3,(#15534,#15535,#15536,#15537,#15538,
#15539,#15540,#15541,#15542,#15543,#15544,#15545,#15546,#15547,#15548,#15549,
#15550,#15551,#15552,#15553,#15554,#15555),.UNSPECIFIED.,.F.,.F.,(4,3,3,
3,3,3,3,4),(70.4248606341475,70.8275674817883,71.8251388547712,72.8227102277542,
73.8202816007371,74.81785297372,75.815424346703,76.7080459413271),
 .UNSPECIFIED.);
#2047=B_SPLINE_CURVE_WITH_KNOTS('',3,(#15556,#15557,#15558,#15559,#15560,
#15561,#15562,#15563,#15564,#15565,#15566,#15567,#15568,#15569,#15570,#15571,
#15572,#15573,#15574,#15575,#15576,#15577,#15578,#15579,#15580),
 .UNSPECIFIED.,.F.,.F.,(4,3,3,3,3,3,3,3,4),(-72.9614216426678,-72.8227102277542,
-71.8251388547712,-70.8275674817883,-69.8299961088054,-68.8324247358224,
-67.8348533628395,-66.8372819898566,-66.6782363354882),.UNSPECIFIED.);
#2048=B_SPLINE_CURVE_WITH_KNOTS('',3,(#15585,#15586,#15587,#15588,#15589,
#15590,#15591,#15592,#15593,#15594,#15595,#15596,#15597,#15598,#15599,#15600,
#15601,#15602,#15603,#15604,#15605,#15606),.UNSPECIFIED.,.F.,.F.,(4,3,3,
3,3,3,3,4),(64.1416753269678,64.8421392438907,65.8397106168736,66.8372819898565,
67.8348533628395,68.8324247358224,69.8299961088054,70.4248606341475),
 .UNSPECIFIED.);
#2049=B_SPLINE_CURVE_WITH_KNOTS('',3,(#15607,#15608,#15609,#15610,#15611,
#15612,#15613,#15614,#15615,#15616,#15617,#15618,#15619,#15620,#15621,#15622,
#15623,#15624,#15625,#15626,#15627,#15628),.UNSPECIFIED.,.F.,.F.,(4,3,3,
3,3,3,3,4),(-66.6782363354882,-65.8397106168736,-64.8421392438907,-63.8445678709078,
-62.8469964979248,-61.8494251249419,-60.851853751959,-60.3950510283085),
 .UNSPECIFIED.);
#2050=B_SPLINE_CURVE_WITH_KNOTS('',3,(#15633,#15634,#15635,#15636,#15637,
#15638,#15639,#15640,#15641,#15642,#15643,#15644,#15645,#15646,#15647,#15648,
#15649,#15650,#15651,#15652,#15653,#15654),.UNSPECIFIED.,.F.,.F.,(4,3,3,
3,3,3,3,4),(57.8584900197882,58.8567110059931,59.854282378976,60.851853751959,
61.8494251249419,62.8469964979248,63.8445678709078,64.1416753269678),
 .UNSPECIFIED.);
#2051=B_SPLINE_CURVE_WITH_KNOTS('',3,(#15655,#15656,#15657,#15658,#15659,
#15660,#15661,#15662,#15663,#15664,#15665,#15666,#15667,#15668,#15669,#15670,
#15671,#15672,#15673,#15674,#15675,#15676),.UNSPECIFIED.,.F.,.F.,(4,3,3,
3,3,3,3,4),(-60.3950510283085,-59.854282378976,-58.8567110059931,-57.8591396330102,
-56.8615682600272,-55.8639968870443,-54.8664255140614,-54.1118657211289),
 .UNSPECIFIED.);
#2052=B_SPLINE_CURVE_WITH_KNOTS('',3,(#15681,#15682,#15683,#15684,#15685,
#15686,#15687,#15688,#15689,#15690,#15691,#15692,#15693,#15694,#15695,#15696,
#15697,#15698,#15699,#15700,#15701,#15702),.UNSPECIFIED.,.F.,.F.,(4,3,3,
3,3,3,3,4),(51.5753047126086,51.8737113951126,52.8712827680955,53.8688541410784,
54.8664255140613,55.8639968870443,56.8615682600272,57.8584900197882),
 .UNSPECIFIED.);
#2053=B_SPLINE_CURVE_WITH_KNOTS('',3,(#15703,#15704,#15705,#15706,#15707,
#15708,#15709,#15710,#15711,#15712,#15713,#15714,#15715,#15716,#15717,#15718,
#15719,#15720,#15721,#15722,#15723,#15724,#15725,#15726,#15727),
 .UNSPECIFIED.,.F.,.F.,(4,3,3,3,3,3,3,3,4),(-54.1118657211289,-53.8688541410784,
-52.8712827680955,-51.8737113951126,-50.8761400221296,-49.8785686491467,
-48.8809972761638,-47.8834259031808,-47.8286804139494),.UNSPECIFIED.);
#2054=B_SPLINE_CURVE_WITH_KNOTS('',3,(#15732,#15733,#15734,#15735,#15736,
#15737,#15738,#15739,#15740,#15741,#15742,#15743,#15744,#15745,#15746,#15747,
#15748,#15749,#15750,#15751,#15752,#15753),.UNSPECIFIED.,.F.,.F.,(4,3,3,
3,3,3,3,4),(45.2921194054291,45.8882831572149,46.8858545301979,47.8834259031808,
48.8809972761637,49.8785686491467,50.8761400221296,51.5753047126086),
 .UNSPECIFIED.);
#2055=B_SPLINE_CURVE_WITH_KNOTS('',3,(#15754,#15755,#15756,#15757,#15758,
#15759,#15760,#15761,#15762,#15763,#15764,#15765,#15766,#15767,#15768,#15769,
#15770,#15771,#15772,#15773,#15774,#15775),.UNSPECIFIED.,.F.,.F.,(4,3,3,
3,3,3,3,4),(-47.8286804139494,-46.8858545301979,-45.888283157215,-44.890711784232,
-43.8931404112491,-42.8955690382662,-41.8979976652832,-41.5454951067698),
 .UNSPECIFIED.);
#2056=B_SPLINE_CURVE_WITH_KNOTS('',3,(#15780,#15781,#15782,#15783,#15784,
#15785,#15786,#15787,#15788,#15789,#15790,#15791,#15792,#15793,#15794,#15795,
#15796,#15797,#15798,#15799,#15800,#15801),.UNSPECIFIED.,.F.,.F.,(4,3,3,
3,3,3,3,4),(39.0089340982495,39.9028549193173,40.9004262923003,41.8979976652832,
42.8955690382661,43.8931404112491,44.890711784232,45.2921194054291),
 .UNSPECIFIED.);
#2057=B_SPLINE_CURVE_WITH_KNOTS('',3,(#15802,#15803,#15804,#15805,#15806,
#15807,#15808,#15809,#15810,#15811,#15812,#15813,#15814,#15815,#15816,#15817,
#15818,#15819,#15820,#15821,#15822,#15823),.UNSPECIFIED.,.F.,.F.,(4,3,3,
3,3,3,3,4),(-41.5454951067698,-40.9004262923003,-39.9028549193174,-38.9052835463344,
-37.9077121733515,-36.9101408003686,-35.9125694273856,-35.2623097995902),
 .UNSPECIFIED.);
#2058=B_SPLINE_CURVE_WITH_KNOTS('',3,(#15828,#15829,#15830,#15831,#15832,
#15833,#15834,#15835,#15836,#15837,#15838,#15839,#15840,#15841,#15842,#15843,
#15844,#15845,#15846,#15847,#15848,#15849,#15850,#15851,#15852),
 .UNSPECIFIED.,.F.,.F.,(4,3,3,3,3,3,3,3,4),(32.7257487910699,32.9198553084368,
33.9174266814197,34.9149980544027,35.9125694273856,36.9101408003685,37.9077121733515,
38.9052835463344,39.0089340982495),.UNSPECIFIED.);
#2059=B_SPLINE_CURVE_WITH_KNOTS('',3,(#15853,#15854,#15855,#15856,#15857,
#15858,#15859,#15860,#15861,#15862,#15863,#15864,#15865,#15866,#15867,#15868,
#15869,#15870,#15871,#15872,#15873,#15874),.UNSPECIFIED.,.F.,.F.,(4,3,3,
3,3,3,3,4),(-35.2623097995902,-34.9149980544027,-33.9174266814198,-32.9198553084368,
-31.9222839354539,-30.924712562471,-29.927141189488,-28.9791244924106),
 .UNSPECIFIED.);
#2060=B_SPLINE_CURVE_WITH_KNOTS('',3,(#15879,#15880,#15881,#15882,#15883,
#15884,#15885,#15886,#15887,#15888,#15889,#15890,#15891,#15892,#15893,#15894,
#15895,#15896,#15897,#15898,#15899,#15900),.UNSPECIFIED.,.F.,.F.,(4,3,3,
3,3,3,3,4),(26.4425634838903,26.9344270705392,27.9319984435221,28.9295698165051,
29.927141189488,30.9247125624709,31.9222839354539,32.7257487910699),
 .UNSPECIFIED.);
#2061=B_SPLINE_CURVE_WITH_KNOTS('',3,(#15901,#15902,#15903,#15904,#15905,
#15906,#15907,#15908,#15909,#15910,#15911,#15912,#15913,#15914,#15915,#15916,
#15917,#15918,#15919,#15920,#15921,#15922,#15923,#15924,#15925),
 .UNSPECIFIED.,.F.,.F.,(4,3,3,3,3,3,3,3,4),(-28.9791244924106,-28.9295698165051,
-27.9319984435222,-26.9344270705392,-25.9368556975563,-24.9392843245733,
-23.9417129515904,-22.9441415786075,-22.695939185231),.UNSPECIFIED.);
#2062=B_SPLINE_CURVE_WITH_KNOTS('',3,(#15930,#15931,#15932,#15933,#15934,
#15935,#15936,#15937,#15938,#15939,#15940,#15941,#15942,#15943,#15944,#15945,
#15946,#15947,#15948,#15949,#15950,#15951),.UNSPECIFIED.,.F.,.F.,(4,3,3,
3,3,3,3,4),(20.1593781767107,20.9489988326416,21.9465702056245,22.9441415786075,
23.9417129515904,24.9392843245733,25.9368556975563,26.4425634838903),
 .UNSPECIFIED.);
#2063=B_SPLINE_CURVE_WITH_KNOTS('',3,(#15952,#15953,#15954,#15955,#15956,
#15957,#15958,#15959,#15960,#15961,#15962,#15963,#15964,#15965,#15966,#15967,
#15968,#15969,#15970,#15971,#15972,#15973),.UNSPECIFIED.,.F.,.F.,(4,3,3,
3,3,3,3,4),(-22.695939185231,-21.9465702056245,-20.9489988326416,-19.9514274596587,
-18.9538560866757,-17.9562847136928,-16.9587133407099,-16.4127538780514),
 .UNSPECIFIED.);
#2064=B_SPLINE_CURVE_WITH_KNOTS('',3,(#15978,#15979,#15980,#15981,#15982,
#15983,#15984,#15985,#15986,#15987,#15988,#15989,#15990,#15991,#15992,#15993,
#15994,#15995,#15996,#15997,#15998,#15999,#16000,#16001,#16002),
 .UNSPECIFIED.,.F.,.F.,(4,3,3,3,3,3,3,3,4),(13.8761928695311,13.9659992217611,
14.963570594744,15.9611419677269,16.9587133407099,17.9562847136928,18.9538560866757,
19.9514274596587,20.1593781767107),.UNSPECIFIED.);
#2065=B_SPLINE_CURVE_WITH_KNOTS('',3,(#16003,#16004,#16005,#16006,#16007,
#16008,#16009,#16010,#16011,#16012,#16013,#16014,#16015,#16016,#16017,#16018,
#16019,#16020,#16021,#16022,#16023,#16024),.UNSPECIFIED.,.F.,.F.,(4,3,3,
3,3,3,3,4),(-16.4127538780514,-15.9611419677269,-14.963570594744,-13.9659992217611,
-12.9684278487781,-11.9708564757952,-10.9732851028123,-10.1295685708718),
 .UNSPECIFIED.);
#2066=B_SPLINE_CURVE_WITH_KNOTS('',3,(#16030,#16031,#16032,#16033,#16034,
#16035,#16036,#16037,#16038,#16039,#16040,#16041,#16042),.UNSPECIFIED.,
 .F.,.F.,(4,3,3,3,4),(-3.84638326369226,-2.9927141189488,-1.99514274596587,
-0.997571372982934,0.),.UNSPECIFIED.);
#2067=B_SPLINE_CURVE_WITH_KNOTS('',3,(#16045,#16046,#16047,#16048,#16049,
#16050,#16051,#16052,#16053,#16054,#16055,#16056,#16057,#16058,#16059,#16060,
#16061,#16062,#16063),.UNSPECIFIED.,.F.,.F.,(4,3,3,3,3,3,4),(2.01461286527457,
2.9927141189488,3.99028549193173,4.98785686491467,5.9854282378976,6.98299961088054,
7.59300756235157),.UNSPECIFIED.);
#2068=B_SPLINE_CURVE_WITH_KNOTS('',3,(#16069,#16070,#16071,#16072,#16073,
#16074,#16075),.UNSPECIFIED.,.F.,.F.,(4,1,1,1,4),(91.106186954104,91.6672898428914,
92.6648612158743,93.6624325888573,94.6600039618402),.UNSPECIFIED.);
#2069=B_SPLINE_CURVE_WITH_KNOTS('',3,(#16078,#16079,#16080,#16081,#16082,
#16083,#16084,#16085),.UNSPECIFIED.,.F.,.F.,(4,1,1,1,1,4),(91.106186954104,
91.2111367324628,92.2087081054457,93.2062794784287,94.2038508514116,95.1819521050859),
 .UNSPECIFIED.);
#2070=B_SPLINE_CURVE_WITH_KNOTS('',3,(#16090,#16091,#16092,#16093,#16094,
#16095,#16096,#16097,#16098,#16099),.UNSPECIFIED.,.F.,.F.,(4,1,1,1,1,1,
1,4),(84.8230016469244,85.6818616049938,86.6794329779767,87.6770043509596,
88.6745757239426,89.6721470969255,90.6697184699085,91.106186954104),
 .UNSPECIFIED.);
#2071=B_SPLINE_CURVE_WITH_KNOTS('',3,(#16100,#16101,#16102,#16103,#16104,
#16105,#16106,#16107,#16108,#16109),.UNSPECIFIED.,.F.,.F.,(4,1,1,1,1,1,
1,4),(84.8230016469244,85.2257084945652,86.2232798675481,87.2208512405311,
88.218422613514,89.2159939864969,90.2135653594799,91.106186954104),
 .UNSPECIFIED.);
#2072=B_SPLINE_CURVE_WITH_KNOTS('',3,(#16114,#16115,#16116,#16117,#16118,
#16119,#16120,#16121,#16122,#16123,#16124),.UNSPECIFIED.,.F.,.F.,(4,1,1,
1,1,1,1,1,4),(78.5398163397448,78.6988619941132,79.6964333670962,80.6940047400791,
81.6915761130621,82.689147486045,83.6867188590279,84.6842902320109,84.8230016469244),
 .UNSPECIFIED.);
#2073=B_SPLINE_CURVE_WITH_KNOTS('',3,(#16125,#16126,#16127,#16128,#16129,
#16130,#16131,#16132,#16133,#16134),.UNSPECIFIED.,.F.,.F.,(4,1,1,1,1,1,
1,4),(78.5398163397448,79.2402802566676,80.2378516296505,81.2354230026335,
82.2329943756164,83.2305657485993,84.2281371215823,84.8230016469244),
 .UNSPECIFIED.);
#2074=B_SPLINE_CURVE_WITH_KNOTS('',3,(#16139,#16140,#16141,#16142,#16143,
#16144,#16145,#16146,#16147,#16148),.UNSPECIFIED.,.F.,.F.,(4,1,1,1,1,1,
1,4),(72.2566310325652,72.7134337562156,73.7110051291986,74.7085765021815,
75.7061478751644,76.7037192481474,77.7012906211303,78.5398163397448),
 .UNSPECIFIED.);
#2075=B_SPLINE_CURVE_WITH_KNOTS('',3,(#16149,#16150,#16151,#16152,#16153,
#16154,#16155,#16156,#16157,#16158,#16159),.UNSPECIFIED.,.F.,.F.,(4,1,1,
1,1,1,1,1,4),(72.2566310325652,72.2572806457871,73.25485201877,74.2524233917529,
75.2499947647359,76.2475661377188,77.2451375107017,78.2427088836847,78.5398163397448),
 .UNSPECIFIED.);
#2076=B_SPLINE_CURVE_WITH_KNOTS('',3,(#16164,#16165,#16166,#16167,#16168,
#16169,#16170,#16171,#16172,#16173),.UNSPECIFIED.,.F.,.F.,(4,1,1,1,1,1,
1,4),(65.9734457253856,66.728005518318,67.725576891301,68.7231482642839,
69.7207196372668,70.7182910102498,71.7158623832327,72.2566310325652),
 .UNSPECIFIED.);
#2077=B_SPLINE_CURVE_WITH_KNOTS('',3,(#16174,#16175,#16176,#16177,#16178,
#16179,#16180,#16181,#16182,#16183),.UNSPECIFIED.,.F.,.F.,(4,1,1,1,1,1,
1,4),(65.9734457253856,66.2718524078895,67.2694237808724,68.2669951538553,
69.2645665268383,70.2621378998212,71.2597092728041,72.2566310325652),
 .UNSPECIFIED.);
#2078=B_SPLINE_CURVE_WITH_KNOTS('',3,(#16188,#16189,#16190,#16191,#16192,
#16193,#16194,#16195,#16196,#16197,#16198),.UNSPECIFIED.,.F.,.F.,(4,1,1,
1,1,1,1,1,4),(59.690260418206,59.7450059074375,60.7425772804204,61.7401486534034,
62.7377200263863,63.7352913993692,64.7328627723522,65.7304341453351,65.9734457253856),
 .UNSPECIFIED.);
#2079=B_SPLINE_CURVE_WITH_KNOTS('',3,(#16199,#16200,#16201,#16202,#16203,
#16204,#16205,#16206,#16207,#16208),.UNSPECIFIED.,.F.,.F.,(4,1,1,1,1,1,
1,4),(59.690260418206,60.2864241699919,61.2839955429748,62.2815669159577,
63.2791382889407,64.2767096619236,65.2742810349065,65.9734457253856),
 .UNSPECIFIED.);
#2080=B_SPLINE_CURVE_WITH_KNOTS('',3,(#16213,#16214,#16215,#16216,#16217,
#16218,#16219,#16220,#16221,#16222),.UNSPECIFIED.,.F.,.F.,(4,1,1,1,1,1,
1,4),(53.4070751110264,53.7595776695399,54.7571490425228,55.7547204155058,
56.7522917884887,57.7498631614716,58.7474345344546,59.690260418206),
 .UNSPECIFIED.);
#2081=B_SPLINE_CURVE_WITH_KNOTS('',3,(#16223,#16224,#16225,#16226,#16227,
#16228,#16229,#16230,#16231,#16232),.UNSPECIFIED.,.F.,.F.,(4,1,1,1,1,1,
1,4),(53.4070751110264,54.3009959320943,55.2985673050772,56.2961386780601,
57.2937100510431,58.291281424026,59.2888527970089,59.690260418206),
 .UNSPECIFIED.);
#2082=B_SPLINE_CURVE_WITH_KNOTS('',3,(#16237,#16238,#16239,#16240,#16241,
#16242,#16243,#16244,#16245,#16246),.UNSPECIFIED.,.F.,.F.,(4,1,1,1,1,1,
1,4),(47.1238898038469,47.7741494316423,48.7717208046252,49.7692921776082,
50.7668635505911,51.764434923574,52.762006296557,53.4070751110264),
 .UNSPECIFIED.);
#2083=B_SPLINE_CURVE_WITH_KNOTS('',3,(#16247,#16248,#16249,#16250,#16251,
#16252,#16253,#16254,#16255,#16256,#16257),.UNSPECIFIED.,.F.,.F.,(4,1,1,
1,1,1,1,1,4),(47.1238898038469,47.3179963212137,48.3155676941967,49.3131390671796,
50.3107104401625,51.3082818131455,52.3058531861284,53.3034245591113,53.4070751110264),
 .UNSPECIFIED.);
#2084=B_SPLINE_CURVE_WITH_KNOTS('',3,(#16262,#16263,#16264,#16265,#16266,
#16267,#16268,#16269,#16270,#16271),.UNSPECIFIED.,.F.,.F.,(4,1,1,1,1,1,
1,4),(40.8407044966673,41.7887211937447,42.7862925667276,43.7838639397106,
44.7814353126935,45.7790066856764,46.7765780586594,47.1238898038469),
 .UNSPECIFIED.);
#2085=B_SPLINE_CURVE_WITH_KNOTS('',3,(#16272,#16273,#16274,#16275,#16276,
#16277,#16278,#16279,#16280,#16281),.UNSPECIFIED.,.F.,.F.,(4,1,1,1,1,1,
1,4),(40.8407044966673,41.3325680833161,42.3301394562991,43.327710829282,
44.3252822022649,45.3228535752479,46.3204249482308,47.1238898038469),
 .UNSPECIFIED.);
#2086=B_SPLINE_CURVE_WITH_KNOTS('',3,(#16286,#16287,#16288,#16289,#16290,
#16291,#16292,#16293,#16294,#16295,#16296),.UNSPECIFIED.,.F.,.F.,(4,1,1,
1,1,1,1,1,4),(34.5575191894876,34.8057215828642,35.8032929558471,36.80086432883,
37.798435701813,38.7960070747959,39.7935784477788,40.7911498207618,40.8407044966673),
 .UNSPECIFIED.);
#2087=B_SPLINE_CURVE_WITH_KNOTS('',3,(#16297,#16298,#16299,#16300,#16301,
#16302,#16303,#16304,#16305,#16306),.UNSPECIFIED.,.F.,.F.,(4,1,1,1,1,1,
1,4),(34.5575191894876,35.3471398454185,36.3447112184015,37.3422825913844,
38.3398539643673,39.3374253373503,40.3349967103332,40.8407044966673),
 .UNSPECIFIED.);
#2088=B_SPLINE_CURVE_WITH_KNOTS('',3,(#16311,#16312,#16313,#16314,#16315,
#16316,#16317,#16318,#16319,#16320),.UNSPECIFIED.,.F.,.F.,(4,1,1,1,1,1,
1,4),(28.2743338823081,28.8202933449666,29.8178647179495,30.8154360909324,
31.8130074639154,32.8105788368983,33.8081502098812,34.5575191894876),
 .UNSPECIFIED.);
#2089=B_SPLINE_CURVE_WITH_KNOTS('',3,(#16321,#16322,#16323,#16324,#16325,
#16326,#16327,#16328,#16329,#16330,#16331),.UNSPECIFIED.,.F.,.F.,(4,1,1,
1,1,1,1,1,4),(28.2743338823081,28.364140234538,29.3617116075209,30.3592829805039,
31.3568543534868,32.3544257264697,33.3519970994527,34.3495684724356,34.5575191894876),
 .UNSPECIFIED.);
#2090=B_SPLINE_CURVE_WITH_KNOTS('',3,(#16336,#16337,#16338,#16339,#16340,
#16341,#16342,#16343,#16344,#16345),.UNSPECIFIED.,.F.,.F.,(4,1,1,1,1,1,
1,4),(21.9911485751285,22.8348651070689,23.8324364800519,24.8300078530348,
25.8275792260178,26.8251505990007,27.8227219719836,28.2743338823081),
 .UNSPECIFIED.);
#2091=B_SPLINE_CURVE_WITH_KNOTS('',3,(#16346,#16347,#16348,#16349,#16350,
#16351,#16352,#16353,#16354,#16355),.UNSPECIFIED.,.F.,.F.,(4,1,1,1,1,1,
1,4),(21.9911485751285,22.3787119966404,23.3762833696233,24.3738547426063,
25.3714261155892,26.3689974885721,27.3665688615551,28.2743338823081),
 .UNSPECIFIED.);
#2092=B_SPLINE_CURVE_WITH_KNOTS('',3,(#16361,#16362,#16363,#16364,#16365),
 .UNSPECIFIED.,.F.,.F.,(4,1,4),(14.3981410127769,15.3957123857599,15.7079632679489),
 .UNSPECIFIED.);
#2093=B_SPLINE_CURVE_WITH_KNOTS('',3,(#16368,#16369,#16370,#16371,#16372),
 .UNSPECIFIED.,.F.,.F.,(4,1,4),(13.8761928695312,14.8542941232055,15.7079632679489),
 .UNSPECIFIED.);
#2094=B_SPLINE_CURVE_WITH_KNOTS('',3,(#16378,#16379,#16380,#16381,#16382,
#16383,#16384,#16385,#16386,#16387,#16388,#16389,#16390,#16391,#16392,#16393,
#16394,#16395,#16396,#16397,#16398,#16399),.UNSPECIFIED.,.F.,.F.,(4,3,3,
3,3,3,3,4),(76.708045941327,76.8129957196859,77.8105670926688,78.8081384656518,
79.8057098386347,80.8032812116176,81.8008525846006,82.7984239575835),
 .UNSPECIFIED.);
#2095=B_SPLINE_CURVE_WITH_KNOTS('',3,(#16403,#16404,#16405,#16406,#16407,
#16408,#16409),.UNSPECIFIED.,.F.,.F.,(4,3,4),(-80.783811092309,-79.8057098386347,
-79.2446069498473),.UNSPECIFIED.);
#2096=B_SPLINE_CURVE_WITH_KNOTS('',3,(#16413,#16414,#16415,#16416,#16417,
#16418,#16419,#16420,#16421,#16422,#16423,#16424,#16425,#16426,#16427,#16428,
#16429,#16430,#16431,#16432,#16433,#16434),.UNSPECIFIED.,.F.,.F.,(4,3,3,
3,3,3,3,4),(-79.2446069498473,-78.8081384656518,-77.8105670926688,-76.8129957196859,
-75.815424346703,-74.81785297372,-73.8202816007371,-72.9614216426678),
 .UNSPECIFIED.);
#2097=B_SPLINE_CURVE_WITH_KNOTS('',3,(#16439,#16440,#16441,#16442,#16443,
#16444,#16445,#16446,#16447,#16448,#16449,#16450,#16451,#16452,#16453,#16454,
#16455,#16456,#16457,#16458,#16459,#16460),.UNSPECIFIED.,.F.,.F.,(4,3,3,
3,3,3,3,4),(70.4248606341475,70.8275674817883,71.8251388547712,72.8227102277542,
73.8202816007371,74.81785297372,75.815424346703,76.708045941327),
 .UNSPECIFIED.);
#2098=B_SPLINE_CURVE_WITH_KNOTS('',3,(#16461,#16462,#16463,#16464,#16465,
#16466,#16467,#16468,#16469,#16470,#16471,#16472,#16473,#16474,#16475,#16476,
#16477,#16478,#16479,#16480,#16481,#16482,#16483,#16484,#16485),
 .UNSPECIFIED.,.F.,.F.,(4,3,3,3,3,3,3,3,4),(-72.9614216426678,-72.8227102277542,
-71.8251388547712,-70.8275674817883,-69.8299961088054,-68.8324247358224,
-67.8348533628395,-66.8372819898566,-66.6782363354882),.UNSPECIFIED.);
#2099=B_SPLINE_CURVE_WITH_KNOTS('',3,(#16490,#16491,#16492,#16493,#16494,
#16495,#16496,#16497,#16498,#16499,#16500,#16501,#16502,#16503,#16504,#16505,
#16506,#16507,#16508,#16509,#16510,#16511),.UNSPECIFIED.,.F.,.F.,(4,3,3,
3,3,3,3,4),(64.1416753269678,64.8421392438907,65.8397106168736,66.8372819898565,
67.8348533628395,68.8324247358224,69.8299961088054,70.4248606341475),
 .UNSPECIFIED.);
#2100=B_SPLINE_CURVE_WITH_KNOTS('',3,(#16512,#16513,#16514,#16515,#16516,
#16517,#16518,#16519,#16520,#16521,#16522,#16523,#16524,#16525,#16526,#16527,
#16528,#16529,#16530,#16531,#16532,#16533),.UNSPECIFIED.,.F.,.F.,(4,3,3,
3,3,3,3,4),(-66.6782363354882,-65.8397106168736,-64.8421392438907,-63.8445678709078,
-62.8469964979248,-61.8494251249419,-60.851853751959,-60.3950510283085),
 .UNSPECIFIED.);
#2101=B_SPLINE_CURVE_WITH_KNOTS('',3,(#16538,#16539,#16540,#16541,#16542,
#16543,#16544,#16545,#16546,#16547,#16548,#16549,#16550,#16551,#16552,#16553,
#16554,#16555,#16556,#16557,#16558,#16559),.UNSPECIFIED.,.F.,.F.,(4,3,3,
3,3,3,3,4),(57.8584900197882,58.8567110059931,59.854282378976,60.8518537519589,
61.8494251249419,62.8469964979248,63.8445678709078,64.1416753269678),
 .UNSPECIFIED.);
#2102=B_SPLINE_CURVE_WITH_KNOTS('',3,(#16560,#16561,#16562,#16563,#16564,
#16565,#16566,#16567,#16568,#16569,#16570,#16571,#16572,#16573,#16574,#16575,
#16576,#16577,#16578,#16579,#16580,#16581),.UNSPECIFIED.,.F.,.F.,(4,3,3,
3,3,3,3,4),(-60.3950510283085,-59.854282378976,-58.8567110059931,-57.8591396330102,
-56.8615682600272,-55.8639968870443,-54.8664255140614,-54.1118657211289),
 .UNSPECIFIED.);
#2103=B_SPLINE_CURVE_WITH_KNOTS('',3,(#16586,#16587,#16588,#16589,#16590,
#16591,#16592,#16593,#16594,#16595,#16596,#16597,#16598,#16599,#16600,#16601,
#16602,#16603,#16604,#16605,#16606,#16607),.UNSPECIFIED.,.F.,.F.,(4,3,3,
3,3,3,3,4),(51.5753047126087,51.8737113951126,52.8712827680955,53.8688541410784,
54.8664255140614,55.8639968870443,56.8615682600272,57.8584900197882),
 .UNSPECIFIED.);
#2104=B_SPLINE_CURVE_WITH_KNOTS('',3,(#16608,#16609,#16610,#16611,#16612,
#16613,#16614,#16615,#16616,#16617,#16618,#16619,#16620,#16621,#16622,#16623,
#16624,#16625,#16626,#16627,#16628,#16629,#16630,#16631,#16632),
 .UNSPECIFIED.,.F.,.F.,(4,3,3,3,3,3,3,3,4),(-54.1118657211289,-53.8688541410784,
-52.8712827680955,-51.8737113951126,-50.8761400221296,-49.8785686491467,
-48.8809972761638,-47.8834259031808,-47.8286804139493),.UNSPECIFIED.);
#2105=B_SPLINE_CURVE_WITH_KNOTS('',3,(#16637,#16638,#16639,#16640,#16641,
#16642,#16643,#16644,#16645,#16646,#16647,#16648,#16649,#16650,#16651,#16652,
#16653,#16654,#16655,#16656,#16657,#16658),.UNSPECIFIED.,.F.,.F.,(4,3,3,
3,3,3,3,4),(45.2921194054291,45.888283157215,46.8858545301979,47.8834259031808,
48.8809972761637,49.8785686491467,50.8761400221296,51.5753047126087),
 .UNSPECIFIED.);
#2106=B_SPLINE_CURVE_WITH_KNOTS('',3,(#16659,#16660,#16661,#16662,#16663,
#16664,#16665,#16666,#16667,#16668,#16669,#16670,#16671,#16672,#16673,#16674,
#16675,#16676,#16677,#16678,#16679,#16680),.UNSPECIFIED.,.F.,.F.,(4,3,3,
3,3,3,3,4),(-47.8286804139493,-46.8858545301979,-45.888283157215,-44.890711784232,
-43.8931404112491,-42.8955690382662,-41.8979976652832,-41.5454951067698),
 .UNSPECIFIED.);
#2107=B_SPLINE_CURVE_WITH_KNOTS('',3,(#16685,#16686,#16687,#16688,#16689,
#16690,#16691,#16692,#16693,#16694,#16695,#16696,#16697,#16698,#16699,#16700,
#16701,#16702,#16703,#16704,#16705,#16706),.UNSPECIFIED.,.F.,.F.,(4,3,3,
3,3,3,3,4),(39.0089340982495,39.9028549193174,40.9004262923003,41.8979976652832,
42.8955690382662,43.8931404112491,44.890711784232,45.2921194054291),
 .UNSPECIFIED.);
#2108=B_SPLINE_CURVE_WITH_KNOTS('',3,(#16707,#16708,#16709,#16710,#16711,
#16712,#16713,#16714,#16715,#16716,#16717,#16718,#16719,#16720,#16721,#16722,
#16723,#16724,#16725,#16726,#16727,#16728),.UNSPECIFIED.,.F.,.F.,(4,3,3,
3,3,3,3,4),(-41.5454951067698,-40.9004262923003,-39.9028549193174,-38.9052835463344,
-37.9077121733515,-36.9101408003686,-35.9125694273856,-35.2623097995902),
 .UNSPECIFIED.);
#2109=B_SPLINE_CURVE_WITH_KNOTS('',3,(#16733,#16734,#16735,#16736,#16737,
#16738,#16739,#16740,#16741,#16742,#16743,#16744,#16745,#16746,#16747,#16748,
#16749,#16750,#16751,#16752,#16753,#16754,#16755,#16756,#16757),
 .UNSPECIFIED.,.F.,.F.,(4,3,3,3,3,3,3,3,4),(32.7257487910699,32.9198553084368,
33.9174266814197,34.9149980544027,35.9125694273856,36.9101408003685,37.9077121733515,
38.9052835463344,39.0089340982495),.UNSPECIFIED.);
#2110=B_SPLINE_CURVE_WITH_KNOTS('',3,(#16758,#16759,#16760,#16761,#16762,
#16763,#16764,#16765,#16766,#16767,#16768,#16769,#16770,#16771,#16772,#16773,
#16774,#16775,#16776,#16777,#16778,#16779),.UNSPECIFIED.,.F.,.F.,(4,3,3,
3,3,3,3,4),(-35.2623097995902,-34.9149980544027,-33.9174266814198,-32.9198553084368,
-31.9222839354539,-30.924712562471,-29.927141189488,-28.9791244924106),
 .UNSPECIFIED.);
#2111=B_SPLINE_CURVE_WITH_KNOTS('',3,(#16784,#16785,#16786,#16787,#16788,
#16789,#16790,#16791,#16792,#16793,#16794,#16795,#16796,#16797,#16798,#16799,
#16800,#16801,#16802,#16803,#16804,#16805),.UNSPECIFIED.,.F.,.F.,(4,3,3,
3,3,3,3,4),(26.4425634838903,26.9344270705392,27.9319984435221,28.9295698165051,
29.927141189488,30.9247125624709,31.9222839354539,32.7257487910699),
 .UNSPECIFIED.);
#2112=B_SPLINE_CURVE_WITH_KNOTS('',3,(#16806,#16807,#16808,#16809,#16810,
#16811,#16812,#16813,#16814,#16815,#16816,#16817,#16818,#16819,#16820,#16821,
#16822,#16823,#16824,#16825,#16826,#16827,#16828,#16829,#16830),
 .UNSPECIFIED.,.F.,.F.,(4,3,3,3,3,3,3,3,4),(-28.9791244924106,-28.9295698165051,
-27.9319984435222,-26.9344270705392,-25.9368556975563,-24.9392843245734,
-23.9417129515904,-22.9441415786075,-22.695939185231),.UNSPECIFIED.);
#2113=B_SPLINE_CURVE_WITH_KNOTS('',3,(#16835,#16836,#16837,#16838,#16839,
#16840,#16841,#16842,#16843,#16844,#16845,#16846,#16847,#16848,#16849,#16850,
#16851,#16852,#16853,#16854,#16855,#16856),.UNSPECIFIED.,.F.,.F.,(4,3,3,
3,3,3,3,4),(20.1593781767107,20.9489988326416,21.9465702056245,22.9441415786075,
23.9417129515904,24.9392843245733,25.9368556975563,26.4425634838903),
 .UNSPECIFIED.);
#2114=B_SPLINE_CURVE_WITH_KNOTS('',3,(#16857,#16858,#16859,#16860,#16861,
#16862,#16863,#16864,#16865,#16866,#16867,#16868,#16869,#16870,#16871,#16872,
#16873,#16874,#16875,#16876,#16877,#16878),.UNSPECIFIED.,.F.,.F.,(4,3,3,
3,3,3,3,4),(-22.695939185231,-21.9465702056245,-20.9489988326416,-19.9514274596587,
-18.9538560866757,-17.9562847136928,-16.9587133407099,-16.4127538780514),
 .UNSPECIFIED.);
#2115=B_SPLINE_CURVE_WITH_KNOTS('',3,(#16883,#16884,#16885,#16886,#16887,
#16888,#16889,#16890,#16891,#16892,#16893,#16894,#16895,#16896,#16897,#16898,
#16899,#16900,#16901,#16902,#16903,#16904,#16905,#16906,#16907),
 .UNSPECIFIED.,.F.,.F.,(4,3,3,3,3,3,3,3,4),(13.8761928695311,13.9659992217611,
14.963570594744,15.9611419677269,16.9587133407099,17.9562847136928,18.9538560866757,
19.9514274596587,20.1593781767107),.UNSPECIFIED.);
#2116=B_SPLINE_CURVE_WITH_KNOTS('',3,(#16908,#16909,#16910,#16911,#16912,
#16913,#16914,#16915,#16916,#16917,#16918,#16919,#16920,#16921,#16922,#16923,
#16924,#16925,#16926,#16927,#16928,#16929),.UNSPECIFIED.,.F.,.F.,(4,3,3,
3,3,3,3,4),(-16.4127538780514,-15.9611419677269,-14.963570594744,-13.9659992217611,
-12.9684278487781,-11.9708564757952,-10.9732851028123,-10.1295685708718),
 .UNSPECIFIED.);
#2117=B_SPLINE_CURVE_WITH_KNOTS('',3,(#16935,#16936,#16937,#16938,#16939,
#16940,#16941,#16942,#16943,#16944,#16945,#16946,#16947),.UNSPECIFIED.,
 .F.,.F.,(4,3,3,3,4),(-3.84638326369226,-2.9927141189488,-1.99514274596587,
-0.997571372982934,0.),.UNSPECIFIED.);
#2118=B_SPLINE_CURVE_WITH_KNOTS('',3,(#16950,#16951,#16952,#16953,#16954,
#16955,#16956,#16957,#16958,#16959,#16960,#16961,#16962,#16963,#16964,#16965,
#16966,#16967,#16968),.UNSPECIFIED.,.F.,.F.,(4,3,3,3,3,3,4),(2.01461286527449,
2.9927141189488,3.99028549193174,4.98785686491467,5.9854282378976,6.98299961088054,
7.59300756235157),.UNSPECIFIED.);
#2119=B_SPLINE_CURVE_WITH_KNOTS('',3,(#16974,#16975,#16976,#16977,#16978,
#16979,#16980),.UNSPECIFIED.,.F.,.F.,(4,1,1,1,4),(91.106186954104,91.6672898428914,
92.6648612158743,93.6624325888573,94.6600039618402),.UNSPECIFIED.);
#2120=B_SPLINE_CURVE_WITH_KNOTS('',3,(#16983,#16984,#16985,#16986,#16987,
#16988,#16989,#16990),.UNSPECIFIED.,.F.,.F.,(4,1,1,1,1,4),(91.106186954104,
91.2111367324628,92.2087081054457,93.2062794784287,94.2038508514116,95.1819521050859),
 .UNSPECIFIED.);
#2121=B_SPLINE_CURVE_WITH_KNOTS('',3,(#16995,#16996,#16997,#16998,#16999,
#17000,#17001,#17002,#17003,#17004),.UNSPECIFIED.,.F.,.F.,(4,1,1,1,1,1,
1,4),(84.8230016469245,85.6818616049938,86.6794329779767,87.6770043509596,
88.6745757239426,89.6721470969255,90.6697184699085,91.106186954104),
 .UNSPECIFIED.);
#2122=B_SPLINE_CURVE_WITH_KNOTS('',3,(#17005,#17006,#17007,#17008,#17009,
#17010,#17011,#17012,#17013,#17014),.UNSPECIFIED.,.F.,.F.,(4,1,1,1,1,1,
1,4),(84.8230016469244,85.2257084945652,86.2232798675481,87.2208512405311,
88.218422613514,89.2159939864969,90.2135653594799,91.106186954104),
 .UNSPECIFIED.);
#2123=B_SPLINE_CURVE_WITH_KNOTS('',3,(#17019,#17020,#17021,#17022,#17023,
#17024,#17025,#17026,#17027,#17028,#17029),.UNSPECIFIED.,.F.,.F.,(4,1,1,
1,1,1,1,1,4),(78.5398163397448,78.6988619941132,79.6964333670962,80.6940047400791,
81.6915761130621,82.689147486045,83.6867188590279,84.6842902320109,84.8230016469245),
 .UNSPECIFIED.);
#2124=B_SPLINE_CURVE_WITH_KNOTS('',3,(#17030,#17031,#17032,#17033,#17034,
#17035,#17036,#17037,#17038,#17039),.UNSPECIFIED.,.F.,.F.,(4,1,1,1,1,1,
1,4),(78.5398163397448,79.2402802566676,80.2378516296505,81.2354230026335,
82.2329943756164,83.2305657485993,84.2281371215823,84.8230016469244),
 .UNSPECIFIED.);
#2125=B_SPLINE_CURVE_WITH_KNOTS('',3,(#17044,#17045,#17046,#17047,#17048,
#17049,#17050,#17051,#17052,#17053),.UNSPECIFIED.,.F.,.F.,(4,1,1,1,1,1,
1,4),(72.2566310325652,72.7134337562156,73.7110051291986,74.7085765021815,
75.7061478751644,76.7037192481474,77.7012906211303,78.5398163397448),
 .UNSPECIFIED.);
#2126=B_SPLINE_CURVE_WITH_KNOTS('',3,(#17054,#17055,#17056,#17057,#17058,
#17059,#17060,#17061,#17062,#17063,#17064),.UNSPECIFIED.,.F.,.F.,(4,1,1,
1,1,1,1,1,4),(72.2566310325652,72.2572806457871,73.25485201877,74.2524233917529,
75.2499947647359,76.2475661377188,77.2451375107017,78.2427088836847,78.5398163397448),
 .UNSPECIFIED.);
#2127=B_SPLINE_CURVE_WITH_KNOTS('',3,(#17069,#17070,#17071,#17072,#17073,
#17074,#17075,#17076,#17077,#17078),.UNSPECIFIED.,.F.,.F.,(4,1,1,1,1,1,
1,4),(65.9734457253856,66.728005518318,67.725576891301,68.7231482642839,
69.7207196372669,70.7182910102498,71.7158623832327,72.2566310325652),
 .UNSPECIFIED.);
#2128=B_SPLINE_CURVE_WITH_KNOTS('',3,(#17079,#17080,#17081,#17082,#17083,
#17084,#17085,#17086,#17087,#17088),.UNSPECIFIED.,.F.,.F.,(4,1,1,1,1,1,
1,4),(65.9734457253856,66.2718524078895,67.2694237808724,68.2669951538553,
69.2645665268383,70.2621378998212,71.2597092728041,72.2566310325652),
 .UNSPECIFIED.);
#2129=B_SPLINE_CURVE_WITH_KNOTS('',3,(#17093,#17094,#17095,#17096,#17097,
#17098,#17099,#17100,#17101,#17102,#17103),.UNSPECIFIED.,.F.,.F.,(4,1,1,
1,1,1,1,1,4),(59.690260418206,59.7450059074375,60.7425772804204,61.7401486534034,
62.7377200263863,63.7352913993692,64.7328627723522,65.7304341453351,65.9734457253856),
 .UNSPECIFIED.);
#2130=B_SPLINE_CURVE_WITH_KNOTS('',3,(#17104,#17105,#17106,#17107,#17108,
#17109,#17110,#17111,#17112,#17113),.UNSPECIFIED.,.F.,.F.,(4,1,1,1,1,1,
1,4),(59.690260418206,60.2864241699919,61.2839955429748,62.2815669159577,
63.2791382889407,64.2767096619236,65.2742810349065,65.9734457253856),
 .UNSPECIFIED.);
#2131=B_SPLINE_CURVE_WITH_KNOTS('',3,(#17118,#17119,#17120,#17121,#17122,
#17123,#17124,#17125,#17126,#17127),.UNSPECIFIED.,.F.,.F.,(4,1,1,1,1,1,
1,4),(53.4070751110265,53.7595776695399,54.7571490425228,55.7547204155058,
56.7522917884887,57.7498631614716,58.7474345344546,59.690260418206),
 .UNSPECIFIED.);
#2132=B_SPLINE_CURVE_WITH_KNOTS('',3,(#17128,#17129,#17130,#17131,#17132,
#17133,#17134,#17135,#17136,#17137),.UNSPECIFIED.,.F.,.F.,(4,1,1,1,1,1,
1,4),(53.4070751110264,54.3009959320943,55.2985673050772,56.2961386780601,
57.2937100510431,58.291281424026,59.2888527970089,59.690260418206),
 .UNSPECIFIED.);
#2133=B_SPLINE_CURVE_WITH_KNOTS('',3,(#17142,#17143,#17144,#17145,#17146,
#17147,#17148,#17149,#17150,#17151),.UNSPECIFIED.,.F.,.F.,(4,1,1,1,1,1,
1,4),(47.1238898038469,47.7741494316423,48.7717208046252,49.7692921776082,
50.7668635505911,51.764434923574,52.762006296557,53.4070751110265),
 .UNSPECIFIED.);
#2134=B_SPLINE_CURVE_WITH_KNOTS('',3,(#17152,#17153,#17154,#17155,#17156,
#17157,#17158,#17159,#17160,#17161,#17162),.UNSPECIFIED.,.F.,.F.,(4,1,1,
1,1,1,1,1,4),(47.1238898038469,47.3179963212137,48.3155676941967,49.3131390671796,
50.3107104401625,51.3082818131455,52.3058531861284,53.3034245591113,53.4070751110264),
 .UNSPECIFIED.);
#2135=B_SPLINE_CURVE_WITH_KNOTS('',3,(#17167,#17168,#17169,#17170,#17171,
#17172,#17173,#17174,#17175,#17176),.UNSPECIFIED.,.F.,.F.,(4,1,1,1,1,1,
1,4),(40.8407044966673,41.7887211937447,42.7862925667276,43.7838639397106,
44.7814353126935,45.7790066856764,46.7765780586594,47.1238898038469),
 .UNSPECIFIED.);
#2136=B_SPLINE_CURVE_WITH_KNOTS('',3,(#17177,#17178,#17179,#17180,#17181,
#17182,#17183,#17184,#17185,#17186),.UNSPECIFIED.,.F.,.F.,(4,1,1,1,1,1,
1,4),(40.8407044966673,41.3325680833161,42.3301394562991,43.327710829282,
44.3252822022649,45.3228535752479,46.3204249482308,47.1238898038469),
 .UNSPECIFIED.);
#2137=B_SPLINE_CURVE_WITH_KNOTS('',3,(#17191,#17192,#17193,#17194,#17195,
#17196,#17197,#17198,#17199,#17200,#17201),.UNSPECIFIED.,.F.,.F.,(4,1,1,
1,1,1,1,1,4),(34.5575191894876,34.8057215828642,35.8032929558471,36.80086432883,
37.798435701813,38.7960070747959,39.7935784477788,40.7911498207618,40.8407044966673),
 .UNSPECIFIED.);
#2138=B_SPLINE_CURVE_WITH_KNOTS('',3,(#17202,#17203,#17204,#17205,#17206,
#17207,#17208,#17209,#17210,#17211),.UNSPECIFIED.,.F.,.F.,(4,1,1,1,1,1,
1,4),(34.5575191894876,35.3471398454185,36.3447112184015,37.3422825913844,
38.3398539643673,39.3374253373503,40.3349967103332,40.8407044966673),
 .UNSPECIFIED.);
#2139=B_SPLINE_CURVE_WITH_KNOTS('',3,(#17216,#17217,#17218,#17219,#17220,
#17221,#17222,#17223,#17224,#17225),.UNSPECIFIED.,.F.,.F.,(4,1,1,1,1,1,
1,4),(28.2743338823081,28.8202933449666,29.8178647179495,30.8154360909324,
31.8130074639154,32.8105788368983,33.8081502098812,34.5575191894876),
 .UNSPECIFIED.);
#2140=B_SPLINE_CURVE_WITH_KNOTS('',3,(#17226,#17227,#17228,#17229,#17230,
#17231,#17232,#17233,#17234,#17235,#17236),.UNSPECIFIED.,.F.,.F.,(4,1,1,
1,1,1,1,1,4),(28.2743338823081,28.364140234538,29.3617116075209,30.3592829805039,
31.3568543534868,32.3544257264697,33.3519970994527,34.3495684724356,34.5575191894876),
 .UNSPECIFIED.);
#2141=B_SPLINE_CURVE_WITH_KNOTS('',3,(#17241,#17242,#17243,#17244,#17245,
#17246,#17247,#17248,#17249,#17250),.UNSPECIFIED.,.F.,.F.,(4,1,1,1,1,1,
1,4),(21.9911485751285,22.834865107069,23.8324364800519,24.8300078530348,
25.8275792260178,26.8251505990007,27.8227219719836,28.2743338823081),
 .UNSPECIFIED.);
#2142=B_SPLINE_CURVE_WITH_KNOTS('',3,(#17251,#17252,#17253,#17254,#17255,
#17256,#17257,#17258,#17259,#17260),.UNSPECIFIED.,.F.,.F.,(4,1,1,1,1,1,
1,4),(21.9911485751285,22.3787119966404,23.3762833696233,24.3738547426063,
25.3714261155892,26.3689974885721,27.3665688615551,28.2743338823081),
 .UNSPECIFIED.);
#2143=B_SPLINE_CURVE_WITH_KNOTS('',3,(#17266,#17267,#17268,#17269,#17270),
 .UNSPECIFIED.,.F.,.F.,(4,1,4),(14.3981410127769,15.3957123857599,15.7079632679489),
 .UNSPECIFIED.);
#2144=B_SPLINE_CURVE_WITH_KNOTS('',3,(#17273,#17274,#17275,#17276,#17277),
 .UNSPECIFIED.,.F.,.F.,(4,1,4),(13.8761928695312,14.8542941232055,15.7079632679489),
 .UNSPECIFIED.);
#2145=B_SPLINE_CURVE_WITH_KNOTS('',3,(#17283,#17284,#17285,#17286,#17287,
#17288,#17289,#17290,#17291,#17292,#17293,#17294,#17295,#17296,#17297,#17298,
#17299,#17300,#17301,#17302,#17303,#17304),.UNSPECIFIED.,.F.,.F.,(4,3,3,
3,3,3,3,4),(76.708045941327,76.812995719686,77.8105670926689,78.8081384656519,
79.8057098386348,80.8032812116177,81.8008525846006,82.7984239575836),
 .UNSPECIFIED.);
#2146=B_SPLINE_CURVE_WITH_KNOTS('',3,(#17308,#17309,#17310,#17311,#17312,
#17313,#17314),.UNSPECIFIED.,.F.,.F.,(4,3,4),(-80.7838110923091,-79.8057098386348,
-79.2446069498473),.UNSPECIFIED.);
#2147=B_SPLINE_CURVE_WITH_KNOTS('',3,(#17318,#17319,#17320,#17321,#17322,
#17323,#17324,#17325,#17326,#17327,#17328,#17329,#17330,#17331,#17332,#17333,
#17334,#17335,#17336,#17337,#17338,#17339),.UNSPECIFIED.,.F.,.F.,(4,3,3,
3,3,3,3,4),(-79.2446069498473,-78.8081384656519,-77.8105670926689,-76.812995719686,
-75.815424346703,-74.8178529737201,-73.8202816007372,-72.9614216426678),
 .UNSPECIFIED.);
#2148=B_SPLINE_CURVE_WITH_KNOTS('',3,(#17344,#17345,#17346,#17347,#17348,
#17349,#17350,#17351,#17352,#17353,#17354,#17355,#17356,#17357,#17358,#17359,
#17360,#17361,#17362,#17363,#17364,#17365),.UNSPECIFIED.,.F.,.F.,(4,3,3,
3,3,3,3,4),(70.4248606341475,70.8275674817884,71.8251388547713,72.8227102277542,
73.8202816007372,74.8178529737201,75.815424346703,76.708045941327),
 .UNSPECIFIED.);
#2149=B_SPLINE_CURVE_WITH_KNOTS('',3,(#17366,#17367,#17368,#17369,#17370,
#17371,#17372,#17373,#17374,#17375,#17376,#17377,#17378,#17379,#17380,#17381,
#17382,#17383,#17384,#17385,#17386,#17387,#17388,#17389,#17390),
 .UNSPECIFIED.,.F.,.F.,(4,3,3,3,3,3,3,3,4),(-72.9614216426678,-72.8227102277542,
-71.8251388547713,-70.8275674817884,-69.8299961088054,-68.8324247358225,
-67.8348533628396,-66.8372819898566,-66.6782363354882),.UNSPECIFIED.);
#2150=B_SPLINE_CURVE_WITH_KNOTS('',3,(#17395,#17396,#17397,#17398,#17399,
#17400,#17401,#17402,#17403,#17404,#17405,#17406,#17407,#17408,#17409,#17410,
#17411,#17412,#17413,#17414,#17415,#17416),.UNSPECIFIED.,.F.,.F.,(4,3,3,
3,3,3,3,4),(64.1416753269678,64.8421392438907,65.8397106168737,66.8372819898566,
67.8348533628396,68.8324247358225,69.8299961088054,70.4248606341475),
 .UNSPECIFIED.);
#2151=B_SPLINE_CURVE_WITH_KNOTS('',3,(#17417,#17418,#17419,#17420,#17421,
#17422,#17423,#17424,#17425,#17426,#17427,#17428,#17429,#17430,#17431,#17432,
#17433,#17434,#17435,#17436,#17437,#17438),.UNSPECIFIED.,.F.,.F.,(4,3,3,
3,3,3,3,4),(-66.6782363354882,-65.8397106168737,-64.8421392438908,-63.8445678709078,
-62.8469964979249,-61.849425124942,-60.851853751959,-60.3950510283085),
 .UNSPECIFIED.);
#2152=B_SPLINE_CURVE_WITH_KNOTS('',3,(#17443,#17444,#17445,#17446,#17447,
#17448,#17449,#17450,#17451,#17452,#17453,#17454,#17455,#17456,#17457,#17458,
#17459,#17460,#17461,#17462,#17463,#17464),.UNSPECIFIED.,.F.,.F.,(4,3,3,
3,3,3,3,4),(57.8584900197882,58.8567110059932,59.8542823789761,60.851853751959,
61.849425124942,62.8469964979249,63.8445678709078,64.1416753269678),
 .UNSPECIFIED.);
#2153=B_SPLINE_CURVE_WITH_KNOTS('',3,(#17465,#17466,#17467,#17468,#17469,
#17470,#17471,#17472,#17473,#17474,#17475,#17476,#17477,#17478,#17479,#17480,
#17481,#17482,#17483,#17484,#17485,#17486),.UNSPECIFIED.,.F.,.F.,(4,3,3,
3,3,3,3,4),(-60.3950510283085,-59.8542823789761,-58.8567110059932,-57.8591396330102,
-56.8615682600273,-55.8639968870443,-54.8664255140614,-54.1118657211289),
 .UNSPECIFIED.);
#2154=B_SPLINE_CURVE_WITH_KNOTS('',3,(#17491,#17492,#17493,#17494,#17495,
#17496,#17497,#17498,#17499,#17500,#17501,#17502,#17503,#17504,#17505,#17506,
#17507,#17508,#17509,#17510,#17511,#17512),.UNSPECIFIED.,.F.,.F.,(4,3,3,
3,3,3,3,4),(51.5753047126087,51.8737113951126,52.8712827680955,53.8688541410785,
54.8664255140614,55.8639968870443,56.8615682600273,57.8584900197882),
 .UNSPECIFIED.);
#2155=B_SPLINE_CURVE_WITH_KNOTS('',3,(#17513,#17514,#17515,#17516,#17517,
#17518,#17519,#17520,#17521,#17522,#17523,#17524,#17525,#17526,#17527,#17528,
#17529,#17530,#17531,#17532,#17533,#17534,#17535,#17536,#17537),
 .UNSPECIFIED.,.F.,.F.,(4,3,3,3,3,3,3,3,4),(-54.1118657211289,-53.8688541410785,
-52.8712827680955,-51.8737113951126,-50.8761400221297,-49.8785686491467,
-48.8809972761638,-47.8834259031809,-47.8286804139493),.UNSPECIFIED.);
#2156=B_SPLINE_CURVE_WITH_KNOTS('',3,(#17542,#17543,#17544,#17545,#17546,
#17547,#17548,#17549,#17550,#17551,#17552,#17553,#17554,#17555,#17556,#17557,
#17558,#17559,#17560,#17561,#17562,#17563),.UNSPECIFIED.,.F.,.F.,(4,3,3,
3,3,3,3,4),(45.2921194054291,45.888283157215,46.8858545301979,47.8834259031809,
48.8809972761638,49.8785686491467,50.8761400221297,51.5753047126087),
 .UNSPECIFIED.);
#2157=B_SPLINE_CURVE_WITH_KNOTS('',3,(#17564,#17565,#17566,#17567,#17568,
#17569,#17570,#17571,#17572,#17573,#17574,#17575,#17576,#17577,#17578,#17579,
#17580,#17581,#17582,#17583,#17584,#17585),.UNSPECIFIED.,.F.,.F.,(4,3,3,
3,3,3,3,4),(-47.8286804139493,-46.8858545301979,-45.888283157215,-44.8907117842321,
-43.8931404112491,-42.8955690382662,-41.8979976652833,-41.5454951067698),
 .UNSPECIFIED.);
#2158=B_SPLINE_CURVE_WITH_KNOTS('',3,(#17590,#17591,#17592,#17593,#17594,
#17595,#17596,#17597,#17598,#17599,#17600,#17601,#17602,#17603,#17604,#17605,
#17606,#17607,#17608,#17609,#17610,#17611),.UNSPECIFIED.,.F.,.F.,(4,3,3,
3,3,3,3,4),(39.0089340982495,39.9028549193174,40.9004262923003,41.8979976652833,
42.8955690382662,43.8931404112491,44.8907117842321,45.2921194054291),
 .UNSPECIFIED.);
#2159=B_SPLINE_CURVE_WITH_KNOTS('',3,(#17612,#17613,#17614,#17615,#17616,
#17617,#17618,#17619,#17620,#17621,#17622,#17623,#17624,#17625,#17626,#17627,
#17628,#17629,#17630,#17631,#17632,#17633),.UNSPECIFIED.,.F.,.F.,(4,3,3,
3,3,3,3,4),(-41.5454951067698,-40.9004262923003,-39.9028549193174,-38.9052835463345,
-37.9077121733515,-36.9101408003686,-35.9125694273856,-35.2623097995902),
 .UNSPECIFIED.);
#2160=B_SPLINE_CURVE_WITH_KNOTS('',3,(#17638,#17639,#17640,#17641,#17642,
#17643,#17644,#17645,#17646,#17647,#17648,#17649,#17650,#17651,#17652,#17653,
#17654,#17655,#17656,#17657,#17658,#17659,#17660,#17661,#17662),
 .UNSPECIFIED.,.F.,.F.,(4,3,3,3,3,3,3,3,4),(32.7257487910699,32.9198553084369,
33.9174266814198,34.9149980544027,35.9125694273857,36.9101408003686,37.9077121733515,
38.9052835463345,39.0089340982495),.UNSPECIFIED.);
#2161=B_SPLINE_CURVE_WITH_KNOTS('',3,(#17663,#17664,#17665,#17666,#17667,
#17668,#17669,#17670,#17671,#17672,#17673,#17674,#17675,#17676,#17677,#17678,
#17679,#17680,#17681,#17682,#17683,#17684),.UNSPECIFIED.,.F.,.F.,(4,3,3,
3,3,3,3,4),(-35.2623097995902,-34.9149980544027,-33.9174266814198,-32.9198553084368,
-31.9222839354539,-30.924712562471,-29.927141189488,-28.9791244924106),
 .UNSPECIFIED.);
#2162=B_SPLINE_CURVE_WITH_KNOTS('',3,(#17689,#17690,#17691,#17692,#17693,
#17694,#17695,#17696,#17697,#17698,#17699,#17700,#17701,#17702,#17703,#17704,
#17705,#17706,#17707,#17708,#17709,#17710),.UNSPECIFIED.,.F.,.F.,(4,3,3,
3,3,3,3,4),(26.4425634838903,26.9344270705392,27.9319984435222,28.9295698165051,
29.927141189488,30.924712562471,31.9222839354539,32.7257487910699),
 .UNSPECIFIED.);
#2163=B_SPLINE_CURVE_WITH_KNOTS('',3,(#17711,#17712,#17713,#17714,#17715,
#17716,#17717,#17718,#17719,#17720,#17721,#17722,#17723,#17724,#17725,#17726,
#17727,#17728,#17729,#17730,#17731,#17732,#17733,#17734,#17735),
 .UNSPECIFIED.,.F.,.F.,(4,3,3,3,3,3,3,3,4),(-28.9791244924106,-28.9295698165051,
-27.9319984435222,-26.9344270705392,-25.9368556975563,-24.9392843245734,
-23.9417129515904,-22.9441415786075,-22.695939185231),.UNSPECIFIED.);
#2164=B_SPLINE_CURVE_WITH_KNOTS('',3,(#17740,#17741,#17742,#17743,#17744,
#17745,#17746,#17747,#17748,#17749,#17750,#17751,#17752,#17753,#17754,#17755,
#17756,#17757,#17758,#17759,#17760,#17761),.UNSPECIFIED.,.F.,.F.,(4,3,3,
3,3,3,3,4),(20.1593781767107,20.9489988326416,21.9465702056246,22.9441415786075,
23.9417129515904,24.9392843245734,25.9368556975563,26.4425634838903),
 .UNSPECIFIED.);
#2165=B_SPLINE_CURVE_WITH_KNOTS('',3,(#17762,#17763,#17764,#17765,#17766,
#17767,#17768,#17769,#17770,#17771,#17772,#17773,#17774,#17775,#17776,#17777,
#17778,#17779,#17780,#17781,#17782,#17783),.UNSPECIFIED.,.F.,.F.,(4,3,3,
3,3,3,3,4),(-22.695939185231,-21.9465702056246,-20.9489988326416,-19.9514274596587,
-18.9538560866758,-17.9562847136928,-16.9587133407099,-16.4127538780514),
 .UNSPECIFIED.);
#2166=B_SPLINE_CURVE_WITH_KNOTS('',3,(#17788,#17789,#17790,#17791,#17792,
#17793,#17794,#17795,#17796,#17797,#17798,#17799,#17800,#17801,#17802,#17803,
#17804,#17805,#17806,#17807,#17808,#17809,#17810,#17811,#17812),
 .UNSPECIFIED.,.F.,.F.,(4,3,3,3,3,3,3,3,4),(13.8761928695311,13.9659992217611,
14.963570594744,15.961141967727,16.9587133407099,17.9562847136928,18.9538560866758,
19.9514274596587,20.1593781767107),.UNSPECIFIED.);
#2167=B_SPLINE_CURVE_WITH_KNOTS('',3,(#17813,#17814,#17815,#17816,#17817,
#17818,#17819,#17820,#17821,#17822,#17823,#17824,#17825,#17826,#17827,#17828,
#17829,#17830,#17831,#17832,#17833,#17834),.UNSPECIFIED.,.F.,.F.,(4,3,3,
3,3,3,3,4),(-16.4127538780514,-15.961141967727,-14.963570594744,-13.9659992217611,
-12.9684278487782,-11.9708564757952,-10.9732851028123,-10.1295685708718),
 .UNSPECIFIED.);
#2168=B_SPLINE_CURVE_WITH_KNOTS('',3,(#17840,#17841,#17842,#17843,#17844,
#17845,#17846,#17847,#17848,#17849,#17850,#17851,#17852),.UNSPECIFIED.,
 .F.,.F.,(4,3,3,3,4),(-3.84638326369226,-2.9927141189488,-1.99514274596587,
-0.997571372982934,0.),.UNSPECIFIED.);
#2169=B_SPLINE_CURVE_WITH_KNOTS('',3,(#17855,#17856,#17857,#17858,#17859,
#17860,#17861,#17862,#17863,#17864,#17865,#17866,#17867,#17868,#17869,#17870,
#17871,#17872,#17873),.UNSPECIFIED.,.F.,.F.,(4,3,3,3,3,3,4),(2.01461286527449,
2.99271411894881,3.99028549193174,4.98785686491468,5.98542823789761,6.98299961088054,
7.59300756235157),.UNSPECIFIED.);
#2170=B_SPLINE_CURVE_WITH_KNOTS('',3,(#17879,#17880,#17881,#17882,#17883,
#17884,#17885),.UNSPECIFIED.,.F.,.F.,(4,1,1,1,4),(91.106186954104,91.6672898428915,
92.6648612158744,93.6624325888573,94.6600039618403),.UNSPECIFIED.);
#2171=B_SPLINE_CURVE_WITH_KNOTS('',3,(#17888,#17889,#17890,#17891,#17892,
#17893,#17894,#17895),.UNSPECIFIED.,.F.,.F.,(4,1,1,1,1,4),(91.106186954104,
91.2111367324629,92.2087081054458,93.2062794784288,94.2038508514117,95.181952105086),
 .UNSPECIFIED.);
#2172=B_SPLINE_CURVE_WITH_KNOTS('',3,(#17900,#17901,#17902,#17903,#17904,
#17905,#17906,#17907,#17908,#17909),.UNSPECIFIED.,.F.,.F.,(4,1,1,1,1,1,
1,4),(84.8230016469245,85.6818616049939,86.6794329779768,87.6770043509597,
88.6745757239427,89.6721470969256,90.6697184699085,91.106186954104),
 .UNSPECIFIED.);
#2173=B_SPLINE_CURVE_WITH_KNOTS('',3,(#17910,#17911,#17912,#17913,#17914,
#17915,#17916,#17917,#17918,#17919),.UNSPECIFIED.,.F.,.F.,(4,1,1,1,1,1,
1,4),(84.8230016469244,85.2257084945653,86.2232798675482,87.2208512405312,
88.2184226135141,89.215993986497,90.21356535948,91.106186954104),
 .UNSPECIFIED.);
#2174=B_SPLINE_CURVE_WITH_KNOTS('',3,(#17924,#17925,#17926,#17927,#17928,
#17929,#17930,#17931,#17932,#17933,#17934),.UNSPECIFIED.,.F.,.F.,(4,1,1,
1,1,1,1,1,4),(78.5398163397448,78.6988619941133,79.6964333670962,80.6940047400792,
81.6915761130621,82.689147486045,83.686718859028,84.6842902320109,84.8230016469245),
 .UNSPECIFIED.);
#2175=B_SPLINE_CURVE_WITH_KNOTS('',3,(#17935,#17936,#17937,#17938,#17939,
#17940,#17941,#17942,#17943,#17944),.UNSPECIFIED.,.F.,.F.,(4,1,1,1,1,1,
1,4),(78.5398163397448,79.2402802566677,80.2378516296506,81.2354230026336,
82.2329943756165,83.2305657485994,84.2281371215823,84.8230016469244),
 .UNSPECIFIED.);
#2176=B_SPLINE_CURVE_WITH_KNOTS('',3,(#17949,#17950,#17951,#17952,#17953,
#17954,#17955,#17956,#17957,#17958),.UNSPECIFIED.,.F.,.F.,(4,1,1,1,1,1,
1,4),(72.2566310325652,72.7134337562157,73.7110051291986,74.7085765021816,
75.7061478751645,76.7037192481474,77.7012906211304,78.5398163397448),
 .UNSPECIFIED.);
#2177=B_SPLINE_CURVE_WITH_KNOTS('',3,(#17959,#17960,#17961,#17962,#17963,
#17964,#17965,#17966,#17967,#17968,#17969),.UNSPECIFIED.,.F.,.F.,(4,1,1,
1,1,1,1,1,4),(72.2566310325652,72.2572806457871,73.2548520187701,74.252423391753,
75.2499947647359,76.2475661377189,77.2451375107018,78.2427088836847,78.5398163397448),
 .UNSPECIFIED.);
#2178=B_SPLINE_CURVE_WITH_KNOTS('',3,(#17974,#17975,#17976,#17977,#17978,
#17979,#17980,#17981,#17982,#17983),.UNSPECIFIED.,.F.,.F.,(4,1,1,1,1,1,
1,4),(65.9734457253856,66.7280055183181,67.725576891301,68.723148264284,
69.7207196372669,70.7182910102498,71.7158623832328,72.2566310325652),
 .UNSPECIFIED.);
#2179=B_SPLINE_CURVE_WITH_KNOTS('',3,(#17984,#17985,#17986,#17987,#17988,
#17989,#17990,#17991,#17992,#17993),.UNSPECIFIED.,.F.,.F.,(4,1,1,1,1,1,
1,4),(65.9734457253856,66.2718524078895,67.2694237808725,68.2669951538554,
69.2645665268383,70.2621378998213,71.2597092728042,72.2566310325652),
 .UNSPECIFIED.);
#2180=B_SPLINE_CURVE_WITH_KNOTS('',3,(#17998,#17999,#18000,#18001,#18002,
#18003,#18004,#18005,#18006,#18007,#18008),.UNSPECIFIED.,.F.,.F.,(4,1,1,
1,1,1,1,1,4),(59.690260418206,59.7450059074375,60.7425772804205,61.7401486534034,
62.7377200263864,63.7352913993693,64.7328627723522,65.7304341453352,65.9734457253856),
 .UNSPECIFIED.);
#2181=B_SPLINE_CURVE_WITH_KNOTS('',3,(#18009,#18010,#18011,#18012,#18013,
#18014,#18015,#18016,#18017,#18018),.UNSPECIFIED.,.F.,.F.,(4,1,1,1,1,1,
1,4),(59.690260418206,60.2864241699919,61.2839955429748,62.2815669159578,
63.2791382889407,64.2767096619236,65.2742810349066,65.9734457253856),
 .UNSPECIFIED.);
#2182=B_SPLINE_CURVE_WITH_KNOTS('',3,(#18023,#18024,#18025,#18026,#18027,
#18028,#18029,#18030,#18031,#18032),.UNSPECIFIED.,.F.,.F.,(4,1,1,1,1,1,
1,4),(53.4070751110265,53.7595776695399,54.7571490425229,55.7547204155058,
56.7522917884887,57.7498631614717,58.7474345344546,59.690260418206),
 .UNSPECIFIED.);
#2183=B_SPLINE_CURVE_WITH_KNOTS('',3,(#18033,#18034,#18035,#18036,#18037,
#18038,#18039,#18040,#18041,#18042),.UNSPECIFIED.,.F.,.F.,(4,1,1,1,1,1,
1,4),(53.4070751110264,54.3009959320943,55.2985673050772,56.2961386780602,
57.2937100510431,58.291281424026,59.288852797009,59.690260418206),
 .UNSPECIFIED.);
#2184=B_SPLINE_CURVE_WITH_KNOTS('',3,(#18047,#18048,#18049,#18050,#18051,
#18052,#18053,#18054,#18055,#18056),.UNSPECIFIED.,.F.,.F.,(4,1,1,1,1,1,
1,4),(47.1238898038469,47.7741494316423,48.7717208046253,49.7692921776082,
50.7668635505911,51.7644349235741,52.762006296557,53.4070751110265),
 .UNSPECIFIED.);
#2185=B_SPLINE_CURVE_WITH_KNOTS('',3,(#18057,#18058,#18059,#18060,#18061,
#18062,#18063,#18064,#18065,#18066,#18067),.UNSPECIFIED.,.F.,.F.,(4,1,1,
1,1,1,1,1,4),(47.1238898038469,47.3179963212138,48.3155676941967,49.3131390671796,
50.3107104401626,51.3082818131455,52.3058531861284,53.3034245591114,53.4070751110264),
 .UNSPECIFIED.);
#2186=B_SPLINE_CURVE_WITH_KNOTS('',3,(#18072,#18073,#18074,#18075,#18076,
#18077,#18078,#18079,#18080,#18081),.UNSPECIFIED.,.F.,.F.,(4,1,1,1,1,1,
1,4),(40.8407044966673,41.7887211937447,42.7862925667277,43.7838639397106,
44.7814353126935,45.7790066856765,46.7765780586594,47.1238898038469),
 .UNSPECIFIED.);
#2187=B_SPLINE_CURVE_WITH_KNOTS('',3,(#18082,#18083,#18084,#18085,#18086,
#18087,#18088,#18089,#18090,#18091),.UNSPECIFIED.,.F.,.F.,(4,1,1,1,1,1,
1,4),(40.8407044966673,41.3325680833162,42.3301394562991,43.327710829282,
44.325282202265,45.3228535752479,46.3204249482308,47.1238898038469),
 .UNSPECIFIED.);
#2188=B_SPLINE_CURVE_WITH_KNOTS('',3,(#18096,#18097,#18098,#18099,#18100,
#18101,#18102,#18103,#18104,#18105,#18106),.UNSPECIFIED.,.F.,.F.,(4,1,1,
1,1,1,1,1,4),(34.5575191894876,34.8057215828642,35.8032929558471,36.80086432883,
37.798435701813,38.7960070747959,39.7935784477789,40.7911498207618,40.8407044966673),
 .UNSPECIFIED.);
#2189=B_SPLINE_CURVE_WITH_KNOTS('',3,(#18107,#18108,#18109,#18110,#18111,
#18112,#18113,#18114,#18115,#18116),.UNSPECIFIED.,.F.,.F.,(4,1,1,1,1,1,
1,4),(34.5575191894876,35.3471398454185,36.3447112184015,37.3422825913844,
38.3398539643674,39.3374253373503,40.3349967103332,40.8407044966673),
 .UNSPECIFIED.);
#2190=B_SPLINE_CURVE_WITH_KNOTS('',3,(#18121,#18122,#18123,#18124,#18125,
#18126,#18127,#18128,#18129,#18130),.UNSPECIFIED.,.F.,.F.,(4,1,1,1,1,1,
1,4),(28.2743338823081,28.8202933449666,29.8178647179495,30.8154360909324,
31.8130074639154,32.8105788368983,33.8081502098812,34.5575191894876),
 .UNSPECIFIED.);
#2191=B_SPLINE_CURVE_WITH_KNOTS('',3,(#18131,#18132,#18133,#18134,#18135,
#18136,#18137,#18138,#18139,#18140,#18141),.UNSPECIFIED.,.F.,.F.,(4,1,1,
1,1,1,1,1,4),(28.2743338823081,28.364140234538,29.3617116075209,30.3592829805039,
31.3568543534868,32.3544257264697,33.3519970994527,34.3495684724356,34.5575191894876),
 .UNSPECIFIED.);
#2192=B_SPLINE_CURVE_WITH_KNOTS('',3,(#18146,#18147,#18148,#18149,#18150,
#18151,#18152,#18153,#18154,#18155),.UNSPECIFIED.,.F.,.F.,(4,1,1,1,1,1,
1,4),(21.9911485751285,22.834865107069,23.8324364800519,24.8300078530348,
25.8275792260178,26.8251505990007,27.8227219719836,28.2743338823081),
 .UNSPECIFIED.);
#2193=B_SPLINE_CURVE_WITH_KNOTS('',3,(#18156,#18157,#18158,#18159,#18160,
#18161,#18162,#18163,#18164,#18165),.UNSPECIFIED.,.F.,.F.,(4,1,1,1,1,1,
1,4),(21.9911485751285,22.3787119966404,23.3762833696233,24.3738547426063,
25.3714261155892,26.3689974885721,27.3665688615551,28.2743338823081),
 .UNSPECIFIED.);
#2194=B_SPLINE_CURVE_WITH_KNOTS('',3,(#18171,#18172,#18173,#18174,#18175),
 .UNSPECIFIED.,.F.,.F.,(4,1,4),(14.3981410127769,15.3957123857599,15.7079632679489),
 .UNSPECIFIED.);
#2195=B_SPLINE_CURVE_WITH_KNOTS('',3,(#18178,#18179,#18180,#18181,#18182),
 .UNSPECIFIED.,.F.,.F.,(4,1,4),(13.8761928695312,14.8542941232055,15.7079632679489),
 .UNSPECIFIED.);
#2196=B_SPLINE_CURVE_WITH_KNOTS('',3,(#18216,#18217,#18218,#18219,#18220,
#18221,#18222,#18223,#18224,#18225,#18226,#18227,#18228,#18229,#18230,#18231,
#18232,#18233,#18234,#18235,#18236,#18237,#18238,#18239,#18240,#18241,#18242,
#18243,#18244,#18245,#18246,#18247,#18248,#18249,#18250,#18251,#18252,#18253,
#18254,#18255,#18256,#18257,#18258,#18259,#18260,#18261,#18262,#18263,#18264,
#18265,#18266,#18267,#18268,#18269,#18270),.UNSPECIFIED.,.F.,.F.,(4,3,3,
3,3,3,3,3,3,3,3,3,3,3,3,3,3,3,4),(-0.378621596831442,-0.353562246097462,
-0.339726792951542,-0.324795397581524,-0.299967980662127,-0.289118724731059,
-0.252370044287308,-0.234474300298533,-0.219335629396853,-0.200829495678085,
-0.174827324623006,-0.15584693665932,-0.144923737522316,-0.109696956092963,
-0.0896699638623999,-0.0773387259299598,-0.0372142298588392,-0.00401661180490446,
0.),.UNSPECIFIED.);
#2197=B_SPLINE_CURVE_WITH_KNOTS('',3,(#18271,#18272,#18273,#18274,#18275,
#18276,#18277,#18278,#18279,#18280,#18281,#18282,#18283,#18284,#18285,#18286,
#18287,#18288,#18289,#18290,#18291,#18292,#18293,#18294,#18295,#18296,#18297,
#18298,#18299,#18300,#18301,#18302,#18303,#18304,#18305,#18306,#18307,#18308,
#18309,#18310,#18311,#18312,#18313,#18314,#18315,#18316,#18317,#18318,#18319,
#18320,#18321,#18322,#18323,#18324,#18325),.UNSPECIFIED.,.F.,.F.,(4,3,3,
3,3,3,3,3,3,3,3,3,3,3,3,3,3,3,4),(-0.376940817211619,-0.351602437043448,
-0.332519408379845,-0.318228058131088,-0.288333449384516,-0.272718117105765,
-0.234505377427356,-0.216962131374135,-0.205493408420767,-0.180854828870943,
-0.153734180151122,-0.136643041471865,-0.126205700111191,-0.0954718773410078,
-0.0666269097764766,-0.0558557551097461,-0.0219614248579871,-0.00327040903045905,
0.),.UNSPECIFIED.);
#2198=B_SPLINE_CURVE_WITH_KNOTS('',3,(#18327,#18328,#18329,#18330,#18331,
#18332,#18333,#18334,#18335,#18336,#18337),.UNSPECIFIED.,.F.,.F.,(4,1,1,
1,1,1,1,1,4),(15.7079632679489,15.8518654961884,16.8494368691714,17.8470082421543,
18.8445796151372,19.8421509881202,20.8397223611031,21.837293734086,21.9911485751285),
 .UNSPECIFIED.);
#2199=B_SPLINE_CURVE_WITH_KNOTS('',3,(#18338,#18339,#18340,#18341,#18342,
#18343,#18344,#18345,#18346,#18347),.UNSPECIFIED.,.F.,.F.,(4,1,1,1,1,1,
1,4),(15.7079632679489,16.3932837587428,17.3908551317257,18.3884265047087,
19.3859978776916,20.3835692506745,21.3811406236575,21.9911485751285),
 .UNSPECIFIED.);
#2200=B_SPLINE_CURVE_WITH_KNOTS('',3,(#18692,#18693,#18694,#18695,#18696,
#18697,#18698,#18699,#18700,#18701,#18702,#18703,#18704,#18705,#18706,#18707,
#18708,#18709,#18710,#18711,#18712,#18713,#18714,#18715,#18716,#18717,#18718,
#18719,#18720,#18721,#18722,#18723,#18724,#18725,#18726,#18727,#18728,#18729,
#18730,#18731,#18732,#18733,#18734,#18735,#18736,#18737,#18738,#18739,#18740,
#18741,#18742,#18743),.UNSPECIFIED.,.F.,.F.,(4,3,3,3,3,3,3,3,3,3,3,3,3,
3,3,3,3,4),(0.,0.0336910847235707,0.0587346654534766,0.0734852364994148,
0.109792238871862,0.132864830837164,0.143632030356024,0.17720525627004,
0.195911997060402,0.20761397219,0.244895171883038,0.269599304636634,0.282507756557061,
0.310158174405463,0.327757797512771,0.342580165552076,0.372940760482292,
0.376940817211643),.UNSPECIFIED.);
#2201=B_SPLINE_CURVE_WITH_KNOTS('',3,(#18744,#18745,#18746,#18747,#18748,
#18749,#18750,#18751,#18752,#18753,#18754,#18755,#18756,#18757,#18758,#18759,
#18760,#18761,#18762,#18763,#18764,#18765,#18766,#18767,#18768),
 .UNSPECIFIED.,.F.,.F.,(4,3,3,3,3,3,3,3,4),(-10.1295685708718,-9.97571372982935,
-8.97814235684642,-7.98057098386348,-6.98299961088054,-5.98542823789761,
-4.98785686491468,-3.99028549193174,-3.84638326369226),.UNSPECIFIED.);
#2202=B_SPLINE_CURVE_WITH_KNOTS('',3,(#19113,#19114,#19115,#19116,#19117,
#19118,#19119,#19120,#19121,#19122,#19123,#19124,#19125,#19126,#19127,#19128,
#19129,#19130,#19131,#19132,#19133,#19134),.UNSPECIFIED.,.F.,.F.,(4,3,3,
3,3,3,3,4),(7.59300756235157,7.98057098386348,8.97814235684642,9.97571372982935,
10.9732851028123,11.9708564757952,12.9684278487781,13.8761928695311),
 .UNSPECIFIED.);
#2203=B_SPLINE_CURVE_WITH_KNOTS('',3,(#19135,#19136,#19137,#19138,#19139,
#19140,#19141,#19142,#19143,#19144,#19145,#19146,#19147,#19148,#19149,#19150,
#19151,#19152,#19153,#19154,#19155,#19156,#19157,#19158,#19159,#19160,#19161,
#19162,#19163,#19164,#19165,#19166,#19167,#19168,#19169,#19170,#19171,#19172,
#19173,#19174,#19175,#19176,#19177,#19178,#19179,#19180,#19181,#19182,#19183,
#19184,#19185,#19186),.UNSPECIFIED.,.F.,.F.,(4,3,3,3,3,3,3,3,3,3,3,3,3,
3,3,3,3,4),(0.,0.039679134584082,0.0597937574063347,0.077198275206118,0.0898304469160062,
0.128492621633409,0.153526594220962,0.165101500237275,0.197163594226419,
0.224452129979101,0.234160526966568,0.26945519714964,0.287578609071477,
0.305421511169844,0.333081607138838,0.347224899232131,0.375339207698859,
0.378621596831424),.UNSPECIFIED.);
#2204=B_SPLINE_CURVE_WITH_KNOTS('',3,(#19189,#19190,#19191,#19192,#19193,
#19194,#19195,#19196,#19197,#19198,#19199,#19200,#19201,#19202,#19203,#19204,
#19205,#19206,#19207,#19208,#19209,#19210,#19211,#19212,#19213,#19214,#19215,
#19216,#19217,#19218,#19219,#19220,#19221,#19222,#19223,#19224,#19225,#19226,
#19227,#19228,#19229,#19230,#19231,#19232,#19233,#19234,#19235,#19236,#19237,
#19238,#19239,#19240,#19241,#19242,#19243),.UNSPECIFIED.,.F.,.F.,(4,3,3,
3,3,3,3,3,3,3,3,3,3,3,3,3,3,3,4),(-0.378621596831421,-0.35356224610225,
-0.339726792605717,-0.324795397019123,-0.299967964935665,-0.289118709747788,
-0.252370025571504,-0.234474277842488,-0.219335629751949,-0.200829495678081,
-0.174827335946658,-0.155846980593001,-0.144923798098897,-0.109697001525397,
-0.0896700514919927,-0.0773387576028108,-0.0372142610763827,-0.00401661180489582,
0.),.UNSPECIFIED.);
#2205=B_SPLINE_CURVE_WITH_KNOTS('',3,(#19244,#19245,#19246,#19247,#19248,
#19249,#19250,#19251,#19252,#19253,#19254,#19255,#19256,#19257,#19258,#19259,
#19260,#19261,#19262,#19263,#19264,#19265,#19266,#19267,#19268,#19269,#19270,
#19271,#19272,#19273,#19274,#19275,#19276,#19277,#19278,#19279,#19280,#19281,
#19282,#19283,#19284,#19285,#19286,#19287,#19288,#19289,#19290,#19291,#19292,
#19293,#19294,#19295,#19296,#19297,#19298),.UNSPECIFIED.,.F.,.F.,(4,3,3,
3,3,3,3,3,3,3,3,3,3,3,3,3,3,3,4),(-0.376940817211658,-0.35160243790482,
-0.332519425088979,-0.318228074800829,-0.288333550643748,-0.272718146690274,
-0.234505396639293,-0.21696217861614,-0.205493442096022,-0.18085482887096,
-0.153734148588707,-0.136642726461199,-0.12620501784944,-0.095471365644694,
-0.0666260826793201,-0.0558555936353674,-0.021961250336811,-0.00327040903045685,
0.),.UNSPECIFIED.);
#2206=B_SPLINE_CURVE_WITH_KNOTS('',3,(#19300,#19301,#19302,#19303,#19304,
#19305,#19306,#19307,#19308,#19309,#19310),.UNSPECIFIED.,.F.,.F.,(4,1,1,
1,1,1,1,1,4),(15.7079632679489,15.8518654961884,16.8494368691713,17.8470082421543,
18.8445796151372,19.8421509881202,20.8397223611031,21.837293734086,21.9911485751285),
 .UNSPECIFIED.);
#2207=B_SPLINE_CURVE_WITH_KNOTS('',3,(#19311,#19312,#19313,#19314,#19315,
#19316,#19317,#19318,#19319,#19320),.UNSPECIFIED.,.F.,.F.,(4,1,1,1,1,1,
1,4),(15.7079632679489,16.3932837587428,17.3908551317257,18.3884265047087,
19.3859978776916,20.3835692506745,21.3811406236575,21.9911485751285),
 .UNSPECIFIED.);
#2208=B_SPLINE_CURVE_WITH_KNOTS('',3,(#19665,#19666,#19667,#19668,#19669,
#19670,#19671,#19672,#19673,#19674,#19675,#19676,#19677,#19678,#19679,#19680,
#19681,#19682,#19683,#19684,#19685,#19686,#19687,#19688,#19689,#19690,#19691,
#19692,#19693,#19694,#19695,#19696,#19697,#19698,#19699,#19700,#19701,#19702,
#19703,#19704,#19705,#19706,#19707,#19708,#19709,#19710,#19711,#19712,#19713,
#19714,#19715,#19716),.UNSPECIFIED.,.F.,.F.,(4,3,3,3,3,3,3,3,3,3,3,3,3,
3,3,3,3,4),(0.,0.0336910497355155,0.058734651365868,0.0734852344555961,
0.109792226014928,0.132864806965475,0.143631988775342,0.17720525627004,
0.1959120018626,0.20761397470913,0.244895197064516,0.269599368515367,0.282507810536056,
0.310158254371969,0.327758642889101,0.342580296989548,0.372940760482291,
0.376940817211643),.UNSPECIFIED.);
#2209=B_SPLINE_CURVE_WITH_KNOTS('',3,(#19717,#19718,#19719,#19720,#19721,
#19722,#19723,#19724,#19725,#19726,#19727,#19728,#19729,#19730,#19731,#19732,
#19733,#19734,#19735,#19736,#19737,#19738,#19739,#19740,#19741),
 .UNSPECIFIED.,.F.,.F.,(4,3,3,3,3,3,3,3,4),(-10.1295685708718,-9.97571372982934,
-8.97814235684641,-7.98057098386347,-6.98299961088054,-5.9854282378976,
-4.98785686491467,-3.99028549193173,-3.84638326369226),.UNSPECIFIED.);
#2210=B_SPLINE_CURVE_WITH_KNOTS('',3,(#20086,#20087,#20088,#20089,#20090,
#20091,#20092,#20093,#20094,#20095,#20096,#20097,#20098,#20099,#20100,#20101,
#20102,#20103,#20104,#20105,#20106,#20107),.UNSPECIFIED.,.F.,.F.,(4,3,3,
3,3,3,3,4),(7.59300756235157,7.98057098386347,8.9781423568464,9.97571372982934,
10.9732851028123,11.9708564757952,12.9684278487781,13.8761928695311),
 .UNSPECIFIED.);
#2211=B_SPLINE_CURVE_WITH_KNOTS('',3,(#20108,#20109,#20110,#20111,#20112,
#20113,#20114,#20115,#20116,#20117,#20118,#20119,#20120,#20121,#20122,#20123,
#20124,#20125,#20126,#20127,#20128,#20129,#20130,#20131,#20132,#20133,#20134,
#20135,#20136,#20137,#20138,#20139,#20140,#20141,#20142,#20143,#20144,#20145,
#20146,#20147,#20148,#20149,#20150,#20151,#20152,#20153,#20154,#20155,#20156,
#20157,#20158,#20159),.UNSPECIFIED.,.F.,.F.,(4,3,3,3,3,3,3,3,3,3,3,3,3,
3,3,3,3,4),(0.,0.0396791423592224,0.0597938176449427,0.0771989368507012,
0.0898305980572942,0.128492765250004,0.153526730198623,0.165101530608957,
0.197163594226419,0.224452126331546,0.234160522045081,0.269455193458526,
0.287578665402526,0.305421500398064,0.333081575029239,0.347224893982947,
0.375339207698863,0.378621596831429),.UNSPECIFIED.);
#2212=B_SPLINE_CURVE_WITH_KNOTS('',3,(#20162,#20163,#20164,#20165,#20166,
#20167,#20168,#20169,#20170,#20171,#20172,#20173,#20174,#20175,#20176,#20177,
#20178,#20179,#20180,#20181,#20182,#20183,#20184,#20185,#20186,#20187,#20188,
#20189,#20190,#20191,#20192,#20193,#20194,#20195,#20196,#20197,#20198,#20199,
#20200,#20201,#20202,#20203,#20204,#20205,#20206,#20207,#20208,#20209,#20210,
#20211,#20212,#20213,#20214,#20215,#20216),.UNSPECIFIED.,.F.,.F.,(4,3,3,
3,3,3,3,3,3,3,3,3,3,3,3,3,3,3,4),(-0.378621596831421,-0.353562246109156,
-0.3397267922352,-0.324795396410533,-0.299967947923947,-0.289118693566506,
-0.252370005353849,-0.234474253593686,-0.219335630122499,-0.200829495678059,
-0.174827348196324,-0.155847028127452,-0.144923863657138,-0.109697050694078,
-0.089670146324546,-0.0773387918294275,-0.0372142948109077,-0.00401661180489871,
0.),.UNSPECIFIED.);
#2213=B_SPLINE_CURVE_WITH_KNOTS('',3,(#20217,#20218,#20219,#20220,#20221,
#20222,#20223,#20224,#20225,#20226,#20227,#20228,#20229,#20230,#20231,#20232,
#20233,#20234,#20235,#20236,#20237,#20238,#20239,#20240,#20241,#20242,#20243,
#20244,#20245,#20246,#20247,#20248,#20249,#20250,#20251,#20252,#20253,#20254,
#20255,#20256,#20257,#20258,#20259,#20260,#20261,#20262,#20263,#20264,#20265,
#20266,#20267,#20268,#20269,#20270,#20271),.UNSPECIFIED.,.F.,.F.,(4,3,3,
3,3,3,3,3,3,3,3,3,3,3,3,3,3,3,4),(-0.376940817211661,-0.351602437644044,
-0.332519420023622,-0.318228069756221,-0.288333520013757,-0.272718137738777,
-0.234505390822111,-0.216962164313794,-0.205493431901863,-0.180854828870961,
-0.15373415812608,-0.13664282164838,-0.126205224016848,-0.0954715202702509,
-0.0666263326168646,-0.0558556424387309,-0.0219613030816618,-0.00327040903045922,
0.),.UNSPECIFIED.);
#2214=B_SPLINE_CURVE_WITH_KNOTS('',3,(#20273,#20274,#20275,#20276,#20277,
#20278,#20279,#20280,#20281,#20282,#20283),.UNSPECIFIED.,.F.,.F.,(4,1,1,
1,1,1,1,1,4),(15.7079632679489,15.8518654961884,16.8494368691713,17.8470082421543,
18.8445796151372,19.8421509881201,20.8397223611031,21.837293734086,21.9911485751285),
 .UNSPECIFIED.);
#2215=B_SPLINE_CURVE_WITH_KNOTS('',3,(#20284,#20285,#20286,#20287,#20288,
#20289,#20290,#20291,#20292,#20293),.UNSPECIFIED.,.F.,.F.,(4,1,1,1,1,1,
1,4),(15.7079632679489,16.3932837587428,17.3908551317257,18.3884265047087,
19.3859978776916,20.3835692506745,21.3811406236575,21.9911485751285),
 .UNSPECIFIED.);
#2216=B_SPLINE_CURVE_WITH_KNOTS('',3,(#20638,#20639,#20640,#20641,#20642,
#20643,#20644,#20645,#20646,#20647,#20648,#20649,#20650,#20651,#20652,#20653,
#20654,#20655,#20656,#20657,#20658,#20659,#20660,#20661,#20662,#20663,#20664,
#20665,#20666,#20667,#20668,#20669,#20670,#20671,#20672,#20673,#20674,#20675,
#20676,#20677,#20678,#20679,#20680,#20681,#20682,#20683,#20684,#20685,#20686,
#20687,#20688,#20689),.UNSPECIFIED.,.F.,.F.,(4,3,3,3,3,3,3,3,3,3,3,3,3,
3,3,3,3,4),(0.,0.0336910603093437,0.0587346556237836,0.0734852350726252,
0.109792229900142,0.132864814179886,0.143632001341265,0.177205256270027,
0.195912000411831,0.207613973950097,0.244895189457593,0.269599349217699,
0.282507794231336,0.310158230215905,0.327758387489592,0.342580257274108,
0.372940760482283,0.376940817211633),.UNSPECIFIED.);
#2217=B_SPLINE_CURVE_WITH_KNOTS('',3,(#20690,#20691,#20692,#20693,#20694,
#20695,#20696,#20697,#20698,#20699,#20700,#20701,#20702,#20703,#20704,#20705,
#20706,#20707,#20708,#20709,#20710,#20711,#20712,#20713,#20714),
 .UNSPECIFIED.,.F.,.F.,(4,3,3,3,3,3,3,3,4),(-10.1295685708718,-9.97571372982934,
-8.97814235684641,-7.98057098386347,-6.98299961088054,-5.9854282378976,
-4.98785686491467,-3.99028549193173,-3.84638326369226),.UNSPECIFIED.);
#2218=B_SPLINE_CURVE_WITH_KNOTS('',3,(#21059,#21060,#21061,#21062,#21063,
#21064,#21065,#21066,#21067,#21068,#21069,#21070,#21071,#21072,#21073,#21074,
#21075,#21076,#21077,#21078,#21079,#21080),.UNSPECIFIED.,.F.,.F.,(4,3,3,
3,3,3,3,4),(7.59300756235157,7.98057098386347,8.9781423568464,9.97571372982934,
10.9732851028123,11.9708564757952,12.9684278487781,13.8761928695311),
 .UNSPECIFIED.);
#2219=B_SPLINE_CURVE_WITH_KNOTS('',3,(#21081,#21082,#21083,#21084,#21085,
#21086,#21087,#21088,#21089,#21090,#21091,#21092,#21093,#21094,#21095,#21096,
#21097,#21098,#21099,#21100,#21101,#21102,#21103,#21104,#21105,#21106,#21107,
#21108,#21109,#21110,#21111,#21112,#21113,#21114,#21115,#21116,#21117,#21118,
#21119,#21120,#21121,#21122,#21123,#21124,#21125,#21126,#21127,#21128,#21129,
#21130,#21131,#21132),.UNSPECIFIED.,.F.,.F.,(4,3,3,3,3,3,3,3,3,3,3,3,3,
3,3,3,3,4),(0.,0.0396791507684394,0.0597938827984087,0.0771996525601983,
0.0898307615993676,0.128492920651297,0.153526877334627,0.165101563474246,
0.197163594226425,0.22445212238587,0.234160516714088,0.269455189460283,
0.287578726323234,0.30542148874616,0.333081540294033,0.34722488830939,0.375339207698871,
0.378621596831437),.UNSPECIFIED.);
#2220=B_SPLINE_CURVE_WITH_KNOTS('',3,(#21135,#21136,#21137,#21138,#21139,
#21140,#21141,#21142,#21143,#21144,#21145,#21146,#21147,#21148,#21149,#21150,
#21151,#21152,#21153,#21154,#21155,#21156,#21157,#21158,#21159,#21160,#21161,
#21162,#21163,#21164,#21165,#21166,#21167,#21168,#21169,#21170,#21171,#21172,
#21173,#21174,#21175,#21176,#21177,#21178,#21179,#21180,#21181,#21182,#21183,
#21184,#21185,#21186,#21187,#21188,#21189),.UNSPECIFIED.,.F.,.F.,(4,3,3,
3,3,3,3,3,3,3,3,3,3,3,3,3,3,3,4),(-0.378621596831443,-0.353562246091994,
-0.33972679327765,-0.324795398102486,-0.29996799510237,-0.289118738473772,
-0.252370061457217,-0.234474320899414,-0.219335629080767,-0.200829495678084,
-0.174827314232915,-0.155846896352443,-0.144923681945981,-0.109696914410712,
-0.0896698834676189,-0.0773386968783234,-0.0372142012245099,-0.00401661180490457,
0.),.UNSPECIFIED.);
#2221=B_SPLINE_CURVE_WITH_KNOTS('',3,(#21190,#21191,#21192,#21193,#21194,
#21195,#21196,#21197,#21198,#21199,#21200,#21201,#21202,#21203,#21204,#21205,
#21206,#21207,#21208,#21209,#21210,#21211,#21212,#21213,#21214,#21215,#21216,
#21217,#21218,#21219,#21220,#21221,#21222,#21223,#21224,#21225,#21226,#21227,
#21228,#21229,#21230,#21231,#21232,#21233,#21234,#21235,#21236,#21237,#21238,
#21239,#21240,#21241,#21242,#21243,#21244),.UNSPECIFIED.,.F.,.F.,(4,3,3,
3,3,3,3,3,3,3,3,3,3,3,3,3,3,3,4),(-0.376940817211611,-0.351602437357937,
-0.332519414484987,-0.318228064219006,-0.288333486347302,-0.272718127906801,
-0.234505384447309,-0.21696214863526,-0.205493420723107,-0.180854828870948,
-0.153734168647042,-0.136642926650914,-0.126205451446247,-0.0954716908423004,
-0.0666266083256078,-0.0558556962658209,-0.0219613612575045,-0.00327040903046154,
0.),.UNSPECIFIED.);
#2222=B_SPLINE_CURVE_WITH_KNOTS('',3,(#21246,#21247,#21248,#21249,#21250,
#21251,#21252,#21253,#21254,#21255,#21256),.UNSPECIFIED.,.F.,.F.,(4,1,1,
1,1,1,1,1,4),(15.7079632679489,15.8518654961884,16.8494368691714,17.8470082421543,
18.8445796151372,19.8421509881202,20.8397223611031,21.837293734086,21.9911485751285),
 .UNSPECIFIED.);
#2223=B_SPLINE_CURVE_WITH_KNOTS('',3,(#21257,#21258,#21259,#21260,#21261,
#21262,#21263,#21264,#21265,#21266),.UNSPECIFIED.,.F.,.F.,(4,1,1,1,1,1,
1,4),(15.7079632679489,16.3932837587428,17.3908551317257,18.3884265047087,
19.3859978776916,20.3835692506745,21.3811406236575,21.9911485751285),
 .UNSPECIFIED.);
#2224=B_SPLINE_CURVE_WITH_KNOTS('',3,(#21611,#21612,#21613,#21614,#21615,
#21616,#21617,#21618,#21619,#21620,#21621,#21622,#21623,#21624,#21625,#21626,
#21627,#21628,#21629,#21630,#21631,#21632,#21633,#21634,#21635,#21636,#21637,
#21638,#21639,#21640,#21641,#21642,#21643,#21644,#21645,#21646,#21647,#21648,
#21649,#21650,#21651,#21652,#21653,#21654,#21655,#21656,#21657,#21658,#21659,
#21660,#21661,#21662),.UNSPECIFIED.,.F.,.F.,(4,3,3,3,3,3,3,3,3,3,3,3,3,
3,3,3,3,4),(0.,0.0336910719722371,0.0587346603191241,0.0734852357557152,
0.109792234187795,0.132864822139093,0.143632015204812,0.177205256270034,
0.195911998811098,0.207613973107216,0.244895181060382,0.269599327917347,
0.282507776228681,0.310158203547799,0.327758105582494,0.342580213444175,
0.372940760482282,0.376940817211633),.UNSPECIFIED.);
#2225=B_SPLINE_CURVE_WITH_KNOTS('',3,(#21663,#21664,#21665,#21666,#21667,
#21668,#21669,#21670,#21671,#21672,#21673,#21674,#21675,#21676,#21677,#21678,
#21679,#21680,#21681,#21682,#21683,#21684,#21685,#21686,#21687),
 .UNSPECIFIED.,.F.,.F.,(4,3,3,3,3,3,3,3,4),(-10.1295685708718,-9.97571372982935,
-8.97814235684641,-7.98057098386348,-6.98299961088054,-5.98542823789761,
-4.98785686491467,-3.99028549193174,-3.84638326369226),.UNSPECIFIED.);
#2226=B_SPLINE_CURVE_WITH_KNOTS('',3,(#22032,#22033,#22034,#22035,#22036,
#22037,#22038,#22039,#22040,#22041,#22042,#22043,#22044,#22045,#22046,#22047,
#22048,#22049,#22050,#22051,#22052,#22053),.UNSPECIFIED.,.F.,.F.,(4,3,3,
3,3,3,3,4),(7.59300756235157,7.98057098386348,8.97814235684641,9.97571372982935,
10.9732851028123,11.9708564757952,12.9684278487782,13.8761928695311),
 .UNSPECIFIED.);
#2227=B_SPLINE_CURVE_WITH_KNOTS('',3,(#22054,#22055,#22056,#22057,#22058,
#22059,#22060,#22061,#22062,#22063,#22064,#22065,#22066,#22067,#22068,#22069,
#22070,#22071,#22072,#22073,#22074,#22075,#22076,#22077,#22078,#22079,#22080,
#22081,#22082,#22083,#22084,#22085,#22086,#22087,#22088,#22089,#22090,#22091,
#22092,#22093,#22094,#22095,#22096,#22097,#22098,#22099,#22100,#22101,#22102,
#22103,#22104,#22105),.UNSPECIFIED.,.F.,.F.,(4,3,3,3,3,3,3,3,3,3,3,3,3,
3,3,3,3,4),(0.,0.0396791274481056,0.0597937021224953,0.0771976680457239,
0.0898303082602208,0.12849248988162,0.15352646947755,0.165101472375799,
0.197163594226428,0.224452133325792,0.23416053148377,0.269455200537544,
0.287578557392714,0.305421521052156,0.333081636597174,0.347224904045167,
0.375339207698866,0.378621596831432),.UNSPECIFIED.);
#2228=B_SPLINE_CURVE_WITH_KNOTS('',3,(#22266,#22267,#22268,#22269,#22270,
#22271,#22272,#22273,#22274,#22275,#22276,#22277,#22278,#22279,#22280,#22281,
#22282,#22283,#22284),.UNSPECIFIED.,.F.,.F.,(4,3,3,3,3,3,4),(20.1579098629397,
20.4694574201275,20.968712479155,21.4679675381825,21.96722259721,22.4664776562375,
22.965732715265),.UNSPECIFIED.);
#2229=B_SPLINE_CURVE_WITH_KNOTS('',3,(#22287,#22288,#22289,#22290,#22291,
#22292,#22293,#22294,#22295,#22296,#22297,#22298,#22299,#22300,#22301,#22302,
#22303,#22304,#22305,#22306,#22307,#22308,#22309,#22310,#22311,#22312,#22313,
#22314,#22315,#22316,#22317),.UNSPECIFIED.,.F.,.F.,(4,3,3,3,3,3,3,3,3,3,
4),(-20.9439510239319,-20.4694574201275,-19.9702023611,-19.4709473020725,
-18.971692243045,-18.4724371840175,-17.97318212499,-17.4739270659625,-16.974672006935,
-16.4754169479075,-16.4213910178811),.UNSPECIFIED.);
#2230=B_SPLINE_CURVE_WITH_KNOTS('',3,(#22322,#22323,#22324,#22325,#22326,
#22327,#22328,#22329,#22330,#22331,#22332,#22333,#22334,#22335,#22336,#22337,
#22338,#22339,#22340,#22341,#22342,#22343,#22344,#22345,#22346,#22347,#22348,
#22349,#22350,#22351,#22352,#22353,#22354,#22355,#22356,#22357,#22358,#22359,
#22360,#22361,#22362,#22363,#22364),.UNSPECIFIED.,.F.,.F.,(4,3,3,3,3,3,
3,3,3,3,3,3,3,3,4),(13.8747245557602,13.97914165277,14.4783967117975,14.977651770825,
15.4769068298525,15.97616188888,16.4754169479075,16.974672006935,17.4739270659625,
17.97318212499,18.4724371840175,18.971692243045,19.4709473020725,19.9702023611,
20.1579098629397),.UNSPECIFIED.);
#2231=B_SPLINE_CURVE_WITH_KNOTS('',3,(#22365,#22366,#22367,#22368,#22369,
#22370,#22371,#22372,#22373,#22374,#22375,#22376,#22377,#22378,#22379,#22380,
#22381,#22382,#22383,#22384,#22385,#22386,#22387,#22388,#22389,#22390,#22391,
#22392,#22393,#22394,#22395,#22396,#22397,#22398,#22399,#22400,#22401,#22402,
#22403,#22404),.UNSPECIFIED.,.F.,.F.,(4,3,3,3,3,3,3,3,3,3,3,3,3,4),(-16.4213910178811,
-15.97616188888,-15.4769068298525,-14.977651770825,-14.4783967117975,-13.97914165277,
-13.4798865937425,-12.980631534715,-12.4813764756875,-11.98212141666,-11.4828663576325,
-10.983611298605,-10.4843562395775,-10.1382057107016),.UNSPECIFIED.);
#2232=B_SPLINE_CURVE_WITH_KNOTS('',3,(#22410,#22411,#22412,#22413,#22414,
#22415,#22416,#22417,#22418,#22419,#22420,#22421,#22422,#22423,#22424,#22425,
#22426,#22427,#22428,#22429,#22430,#22431,#22432,#22433,#22434),
 .UNSPECIFIED.,.F.,.F.,(4,3,3,3,3,3,3,3,4),(-3.85502040352197,-3.49478541319251,
-2.995530354165,-2.4962752951375,-1.99702023611001,-1.4977651770825,-0.998510118055002,
-0.499255059027501,0.),.UNSPECIFIED.);
#2233=B_SPLINE_CURVE_WITH_KNOTS('',3,(#22437,#22438,#22439,#22440,#22441,
#22442,#22443,#22444,#22445,#22446,#22447,#22448,#22449,#22450,#22451,#22452,
#22453,#22454,#22455,#22456,#22457,#22458,#22459,#22460,#22461,#22462,#22463,
#22464,#22465,#22466,#22467,#22468,#22469,#22470,#22471,#22472,#22473),
 .UNSPECIFIED.,.F.,.F.,(4,3,3,3,3,3,3,3,3,3,3,3,4),(2.02178169133306,2.4962752951375,
2.99553035416501,3.49478541319251,3.99404047222001,4.49329553124751,4.99255059027501,
5.49180564930251,5.99106070833001,6.49031576735751,6.98957082638501,7.48882588541252,
7.59153924858057),.UNSPECIFIED.);
#2234=B_SPLINE_CURVE_WITH_KNOTS('',3,(#22479,#22480,#22481,#22482,#22483,
#22484,#22485,#22486,#22487,#22488,#22489,#22490,#22491,#22492,#22493,#22494,
#22495,#22496,#22497),.UNSPECIFIED.,.F.,.F.,(4,3,3,3,3,3,4),(20.1579098629397,
20.4694574201275,20.968712479155,21.4679675381825,21.96722259721,22.4664776562375,
22.965732715265),.UNSPECIFIED.);
#2235=B_SPLINE_CURVE_WITH_KNOTS('',3,(#22500,#22501,#22502,#22503,#22504,
#22505,#22506,#22507,#22508,#22509,#22510,#22511,#22512,#22513,#22514,#22515,
#22516,#22517,#22518,#22519,#22520,#22521,#22522,#22523,#22524,#22525,#22526,
#22527,#22528,#22529,#22530),.UNSPECIFIED.,.F.,.F.,(4,3,3,3,3,3,3,3,3,3,
4),(-20.9439510239319,-20.4694574201275,-19.9702023611,-19.4709473020725,
-18.971692243045,-18.4724371840175,-17.97318212499,-17.4739270659625,-16.974672006935,
-16.4754169479075,-16.4213910178811),.UNSPECIFIED.);
#2236=B_SPLINE_CURVE_WITH_KNOTS('',3,(#22535,#22536,#22537,#22538,#22539,
#22540,#22541,#22542,#22543,#22544,#22545,#22546,#22547,#22548,#22549,#22550,
#22551,#22552,#22553,#22554,#22555,#22556,#22557,#22558,#22559,#22560,#22561,
#22562,#22563,#22564,#22565,#22566,#22567,#22568,#22569,#22570,#22571,#22572,
#22573,#22574,#22575,#22576,#22577),.UNSPECIFIED.,.F.,.F.,(4,3,3,3,3,3,
3,3,3,3,3,3,3,3,4),(13.8747245557602,13.97914165277,14.4783967117975,14.977651770825,
15.4769068298525,15.97616188888,16.4754169479075,16.974672006935,17.4739270659625,
17.97318212499,18.4724371840175,18.971692243045,19.4709473020725,19.9702023611,
20.1579098629397),.UNSPECIFIED.);
#2237=B_SPLINE_CURVE_WITH_KNOTS('',3,(#22578,#22579,#22580,#22581,#22582,
#22583,#22584,#22585,#22586,#22587,#22588,#22589,#22590,#22591,#22592,#22593,
#22594,#22595,#22596,#22597,#22598,#22599,#22600,#22601,#22602,#22603,#22604,
#22605,#22606,#22607,#22608,#22609,#22610,#22611,#22612,#22613,#22614,#22615,
#22616,#22617),.UNSPECIFIED.,.F.,.F.,(4,3,3,3,3,3,3,3,3,3,3,3,3,4),(-16.4213910178811,
-15.97616188888,-15.4769068298525,-14.977651770825,-14.4783967117975,-13.97914165277,
-13.4798865937425,-12.980631534715,-12.4813764756875,-11.98212141666,-11.4828663576325,
-10.983611298605,-10.4843562395775,-10.1382057107016),.UNSPECIFIED.);
#2238=B_SPLINE_CURVE_WITH_KNOTS('',3,(#22623,#22624,#22625,#22626,#22627,
#22628,#22629,#22630,#22631,#22632,#22633,#22634,#22635,#22636,#22637,#22638,
#22639,#22640,#22641,#22642,#22643,#22644,#22645,#22646,#22647),
 .UNSPECIFIED.,.F.,.F.,(4,3,3,3,3,3,3,3,4),(-3.85502040352197,-3.49478541319251,
-2.995530354165,-2.4962752951375,-1.99702023611001,-1.4977651770825,-0.998510118055002,
-0.499255059027501,0.),.UNSPECIFIED.);
#2239=B_SPLINE_CURVE_WITH_KNOTS('',3,(#22650,#22651,#22652,#22653,#22654,
#22655,#22656,#22657,#22658,#22659,#22660,#22661,#22662,#22663,#22664,#22665,
#22666,#22667,#22668,#22669,#22670,#22671,#22672,#22673,#22674,#22675,#22676,
#22677,#22678,#22679,#22680,#22681,#22682,#22683,#22684,#22685,#22686),
 .UNSPECIFIED.,.F.,.F.,(4,3,3,3,3,3,3,3,3,3,3,3,4),(2.02178169133306,2.4962752951375,
2.99553035416501,3.49478541319251,3.99404047222001,4.49329553124751,4.99255059027501,
5.49180564930251,5.99106070833001,6.49031576735751,6.98957082638501,7.48882588541252,
7.59153924858057),.UNSPECIFIED.);
#2240=B_SPLINE_CURVE_WITH_KNOTS('',3,(#22692,#22693,#22694,#22695),
 .UNSPECIFIED.,.F.,.F.,(4,4),(34.5575191894877,34.818675579692),
 .UNSPECIFIED.);
#2241=B_SPLINE_CURVE_WITH_KNOTS('',3,(#22698,#22699,#22700,#22701,#22702),
 .UNSPECIFIED.,.F.,.F.,(4,1,4),(34.5575191894877,34.8690667466755,35.3435603504799),
 .UNSPECIFIED.);
#2242=B_SPLINE_CURVE_WITH_KNOTS('',3,(#22707,#22708,#22709,#22710,#22711,
#22712,#22713,#22714,#22715,#22716,#22717,#22718,#22719,#22720,#22721,#22722,
#22723),.UNSPECIFIED.,.F.,.F.,(4,1,1,1,1,1,1,1,1,1,1,1,1,1,4),(28.2743338823081,
28.3283598123345,28.827614871362,29.3268699303895,29.826124989417,30.3253800484445,
30.824635107472,31.3238901664995,31.823145225527,32.3224002845545,32.821655343582,
33.3209104026095,33.820165461637,34.3194205206645,34.5575191894877),
 .UNSPECIFIED.);
#2243=B_SPLINE_CURVE_WITH_KNOTS('',3,(#22724,#22725,#22726,#22727,#22728,
#22729,#22730,#22731,#22732,#22733,#22734,#22735,#22736,#22737,#22738,#22739,
#22740),.UNSPECIFIED.,.F.,.F.,(4,1,1,1,1,1,1,1,1,1,1,1,1,1,4),(28.2743338823081,
28.378750979318,28.8780060383455,29.377261097373,29.8765161564005,30.375771215428,
30.8750262744555,31.374281333483,31.8735363925105,32.372791451538,32.8720465105655,
33.371301569593,33.8705566286205,34.369811687648,34.5575191894877),
 .UNSPECIFIED.);
#2244=B_SPLINE_CURVE_WITH_KNOTS('',3,(#22745,#22746,#22747,#22748,#22749,
#22750,#22751,#22752,#22753,#22754,#22755,#22756,#22757,#22758,#22759,#22760),
 .UNSPECIFIED.,.F.,.F.,(4,1,1,1,1,1,1,1,1,1,1,1,1,4),(21.9911485751285,
22.3372991040045,22.836554163032,23.3358092220595,23.835064281087,24.3343193401145,
24.833574399142,25.3328294581695,25.832084517197,26.3313395762245,26.830594635252,
27.3298496942795,27.829104753307,28.2743338823081),.UNSPECIFIED.);
#2245=B_SPLINE_CURVE_WITH_KNOTS('',3,(#22761,#22762,#22763,#22764,#22765,
#22766,#22767,#22768,#22769,#22770,#22771,#22772,#22773,#22774,#22775,#22776),
 .UNSPECIFIED.,.F.,.F.,(4,1,1,1,1,1,1,1,1,1,1,1,1,4),(21.9911485751285,
22.387690270988,22.8869453300155,23.386200389043,23.8854554480705,24.384710507098,
24.8839655661255,25.383220625153,25.8824756841805,26.381730743208,26.8809858022355,
27.380240861263,27.8794959202905,28.2743338823081),.UNSPECIFIED.);
#2246=B_SPLINE_CURVE_WITH_KNOTS('',3,(#22782,#22783,#22784,#22785,#22786,
#22787),.UNSPECIFIED.,.F.,.F.,(4,1,1,4),(14.399609326548,14.8988643855755,
15.398119444603,15.707963267949),.UNSPECIFIED.);
#2247=B_SPLINE_CURVE_WITH_KNOTS('',3,(#22790,#22791,#22792,#22793,#22794,
#22795,#22796),.UNSPECIFIED.,.F.,.F.,(4,1,1,1,4),(13.8747245557601,14.3492181595645,
14.848473218592,15.3477282776195,15.707963267949),.UNSPECIFIED.);
#2248=B_SPLINE_CURVE_WITH_KNOTS('',3,(#22802,#22803,#22804,#22805),
 .UNSPECIFIED.,.F.,.F.,(4,4),(34.5575191894877,34.818675579692),
 .UNSPECIFIED.);
#2249=B_SPLINE_CURVE_WITH_KNOTS('',3,(#22808,#22809,#22810,#22811,#22812),
 .UNSPECIFIED.,.F.,.F.,(4,1,4),(34.5575191894877,34.8690667466755,35.3435603504799),
 .UNSPECIFIED.);
#2250=B_SPLINE_CURVE_WITH_KNOTS('',3,(#22817,#22818,#22819,#22820,#22821,
#22822,#22823,#22824,#22825,#22826,#22827,#22828,#22829,#22830,#22831,#22832,
#22833),.UNSPECIFIED.,.F.,.F.,(4,1,1,1,1,1,1,1,1,1,1,1,1,1,4),(28.2743338823081,
28.3283598123345,28.827614871362,29.3268699303895,29.826124989417,30.3253800484445,
30.824635107472,31.3238901664995,31.823145225527,32.3224002845545,32.821655343582,
33.3209104026095,33.820165461637,34.3194205206645,34.5575191894877),
 .UNSPECIFIED.);
#2251=B_SPLINE_CURVE_WITH_KNOTS('',3,(#22834,#22835,#22836,#22837,#22838,
#22839,#22840,#22841,#22842,#22843,#22844,#22845,#22846,#22847,#22848,#22849,
#22850),.UNSPECIFIED.,.F.,.F.,(4,1,1,1,1,1,1,1,1,1,1,1,1,1,4),(28.2743338823081,
28.378750979318,28.8780060383455,29.377261097373,29.8765161564005,30.375771215428,
30.8750262744555,31.374281333483,31.8735363925105,32.372791451538,32.8720465105655,
33.371301569593,33.8705566286205,34.369811687648,34.5575191894877),
 .UNSPECIFIED.);
#2252=B_SPLINE_CURVE_WITH_KNOTS('',3,(#22855,#22856,#22857,#22858,#22859,
#22860,#22861,#22862,#22863,#22864,#22865,#22866,#22867,#22868,#22869,#22870),
 .UNSPECIFIED.,.F.,.F.,(4,1,1,1,1,1,1,1,1,1,1,1,1,4),(21.9911485751285,
22.3372991040045,22.836554163032,23.3358092220595,23.835064281087,24.3343193401145,
24.833574399142,25.3328294581695,25.832084517197,26.3313395762245,26.830594635252,
27.3298496942795,27.829104753307,28.2743338823081),.UNSPECIFIED.);
#2253=B_SPLINE_CURVE_WITH_KNOTS('',3,(#22871,#22872,#22873,#22874,#22875,
#22876,#22877,#22878,#22879,#22880,#22881,#22882,#22883,#22884,#22885,#22886),
 .UNSPECIFIED.,.F.,.F.,(4,1,1,1,1,1,1,1,1,1,1,1,1,4),(21.9911485751285,
22.387690270988,22.8869453300155,23.386200389043,23.8854554480705,24.384710507098,
24.8839655661255,25.383220625153,25.8824756841805,26.381730743208,26.8809858022355,
27.380240861263,27.8794959202905,28.2743338823081),.UNSPECIFIED.);
#2254=B_SPLINE_CURVE_WITH_KNOTS('',3,(#22892,#22893,#22894,#22895,#22896,
#22897),.UNSPECIFIED.,.F.,.F.,(4,1,1,4),(14.399609326548,14.8988643855755,
15.398119444603,15.707963267949),.UNSPECIFIED.);
#2255=B_SPLINE_CURVE_WITH_KNOTS('',3,(#22900,#22901,#22902,#22903,#22904,
#22905,#22906),.UNSPECIFIED.,.F.,.F.,(4,1,1,1,4),(13.8747245557601,14.3492181595645,
14.848473218592,15.3477282776195,15.707963267949),.UNSPECIFIED.);
#2256=B_SPLINE_CURVE_WITH_KNOTS('',3,(#22969,#22970,#22971,#22972,#22973,
#22974,#22975,#22976,#22977,#22978,#22979,#22980,#22981,#22982,#22983,#22984,
#22985),.UNSPECIFIED.,.F.,.F.,(4,1,1,1,1,1,1,1,1,1,1,1,1,1,4),(15.707963267949,
15.846983336647,16.3462383956745,16.845493454702,17.3447485137295,17.844003572757,
18.3432586317845,18.842513690812,19.3417687498395,19.841023808867,20.3402788678945,
20.839533926922,21.3387889859495,21.838044044977,21.9911485751285),
 .UNSPECIFIED.);
#2257=B_SPLINE_CURVE_WITH_KNOTS('',3,(#22986,#22987,#22988,#22989,#22990,
#22991,#22992,#22993,#22994,#22995,#22996,#22997,#22998,#22999,#23000,#23001,
#23002),.UNSPECIFIED.,.F.,.F.,(4,1,1,1,1,1,1,1,1,1,1,1,1,1,4),(15.707963267949,
15.8973745036305,16.396629562658,16.8958846216855,17.395139680713,17.8943947397405,
18.393649798768,18.8929048577955,19.392159916823,19.8914149758505,20.390670034878,
20.8899250939055,21.389180152933,21.8884352119605,21.9911485751285),
 .UNSPECIFIED.);
#2258=B_SPLINE_CURVE_WITH_KNOTS('',3,(#23199,#23200,#23201,#23202,#23203,
#23204,#23205,#23206,#23207,#23208,#23209,#23210,#23211,#23212,#23213,#23214,
#23215,#23216,#23217,#23218,#23219,#23220,#23221,#23222,#23223,#23224,#23225,
#23226,#23227,#23228,#23229,#23230,#23231,#23232,#23233,#23234,#23235,#23236,
#23237,#23238,#23239,#23240,#23241,#23242,#23243,#23244,#23245,#23246,#23247,
#23248,#23249,#23250,#23251,#23252,#23253,#23254,#23255,#23256,#23257,#23258,
#23259,#23260,#23261,#23262,#23263,#23264,#23265,#23266,#23267,#23268,#23269,
#23270,#23271),.UNSPECIFIED.,.F.,.F.,(4,3,3,3,3,3,3,3,3,3,3,3,3,3,3,3,3,
3,3,3,3,3,3,3,4),(-0.950777871811465,-0.888334407370769,-0.851051814776991,
-0.82737904373313,-0.764191528890905,-0.727096293545134,-0.707864357405063,
-0.701004014048681,-0.624532510230306,-0.548715306176616,-0.528886751702636,
-0.51335217329456,-0.460845815077925,-0.386468184274459,-0.349072714542667,
-0.331943455188318,-0.259671363135132,-0.230659644409349,-0.19743434794885,
-0.175120034180883,-0.157580682039417,-0.0841021758717334,-0.0150413926252008,
-0.0106236697040495,0.),.UNSPECIFIED.);
#2259=B_SPLINE_CURVE_WITH_KNOTS('',3,(#23272,#23273,#23274,#23275,#23276,
#23277,#23278,#23279,#23280,#23281,#23282,#23283,#23284,#23285,#23286,#23287,
#23288,#23289,#23290,#23291,#23292,#23293,#23294,#23295,#23296,#23297,#23298,
#23299,#23300,#23301,#23302,#23303,#23304,#23305,#23306,#23307,#23308,#23309,
#23310,#23311,#23312,#23313,#23314,#23315,#23316,#23317,#23318,#23319,#23320,
#23321,#23322,#23323,#23324,#23325,#23326,#23327,#23328,#23329,#23330,#23331,
#23332,#23333,#23334,#23335,#23336,#23337,#23338,#23339,#23340,#23341),
 .UNSPECIFIED.,.F.,.F.,(4,3,3,3,3,3,3,3,3,3,3,3,3,3,3,3,3,3,3,3,3,3,3,4),
(0.,0.0695167991119783,0.140212658431775,0.162172470483188,0.179979408684031,
0.219498223261391,0.291822018016311,0.337745303611425,0.355228583776568,
0.429645631566202,0.449180111380345,0.509263572656178,0.525649154341391,
0.601088264154331,0.677503858556246,0.688874999321038,0.709603483853625,
0.730479306054779,0.782399641108501,0.820902701806524,0.845385896033558,
0.924612288143001,0.938160646269666,0.950777871811463),.UNSPECIFIED.);
#2260=B_SPLINE_CURVE_WITH_KNOTS('',3,(#23342,#23343,#23344,#23345,#23346,
#23347,#23348,#23349,#23350,#23351,#23352,#23353,#23354,#23355,#23356,#23357,
#23358,#23359,#23360,#23361,#23362,#23363,#23364,#23365,#23366,#23367,#23368,
#23369,#23370,#23371,#23372,#23373,#23374,#23375,#23376,#23377,#23378,#23379,
#23380,#23381,#23382,#23383,#23384),.UNSPECIFIED.,.F.,.F.,(4,3,3,3,3,3,
3,3,3,3,3,3,3,3,4),(-10.1382057107016,-9.98510118055001,-9.48584612152251,
-8.98659106249501,-8.48733600346751,-7.98808094444001,-7.48882588541251,
-6.98957082638501,-6.49031576735751,-5.99106070833001,-5.49180564930251,
-4.99255059027501,-4.49329553124751,-3.99404047222001,-3.85502040352197),
 .UNSPECIFIED.);
#2261=B_SPLINE_CURVE_WITH_KNOTS('',3,(#23581,#23582,#23583,#23584,#23585,
#23586,#23587,#23588,#23589,#23590,#23591,#23592,#23593,#23594,#23595,#23596,
#23597,#23598,#23599,#23600,#23601,#23602,#23603,#23604,#23605,#23606,#23607,
#23608,#23609,#23610,#23611,#23612,#23613,#23614,#23615,#23616,#23617,#23618,
#23619,#23620,#23621,#23622,#23623,#23624,#23625,#23626,#23627,#23628,#23629,
#23630,#23631,#23632,#23633,#23634,#23635,#23636,#23637,#23638,#23639,#23640,
#23641,#23642,#23643,#23644,#23645,#23646,#23647,#23648,#23649,#23650),
 .UNSPECIFIED.,.F.,.F.,(4,3,3,3,3,3,3,3,3,3,3,3,3,3,3,3,3,3,3,3,3,3,3,4),
(-0.954382097139049,-0.899410408801335,-0.859358635307587,-0.836685957905282,
-0.785590650846737,-0.75140161257743,-0.734495343788191,-0.662158982507963,
-0.588787990221564,-0.570217280263643,-0.551422718402641,-0.504011712732237,
-0.443843717567291,-0.393584703400901,-0.372143080358795,-0.295059059270718,
-0.263339732072452,-0.224912725821683,-0.201648013648112,-0.183362315801792,
-0.105092336646239,-0.0261711118220366,-0.0126626251736613,0.),
 .UNSPECIFIED.);
#2262=B_SPLINE_CURVE_WITH_KNOTS('',3,(#23651,#23652,#23653,#23654,#23655,
#23656,#23657,#23658,#23659,#23660,#23661,#23662,#23663,#23664,#23665,#23666,
#23667,#23668,#23669,#23670,#23671,#23672,#23673,#23674,#23675,#23676,#23677,
#23678,#23679,#23680,#23681,#23682,#23683,#23684,#23685,#23686,#23687,#23688,
#23689,#23690),.UNSPECIFIED.,.F.,.F.,(4,3,3,3,3,3,3,3,3,3,3,3,3,4),(7.59153924858057,
7.98808094444002,8.48733600346752,8.98659106249502,9.48584612152252,9.98510118055002,
10.4843562395775,10.983611298605,11.4828663576325,11.98212141666,12.4813764756875,
12.980631534715,13.4798865937425,13.8747245557602),.UNSPECIFIED.);
#2263=B_SPLINE_CURVE_WITH_KNOTS('',3,(#23691,#23692,#23693,#23694,#23695,
#23696,#23697,#23698,#23699,#23700,#23701,#23702,#23703,#23704,#23705,#23706,
#23707,#23708,#23709,#23710,#23711,#23712,#23713,#23714,#23715,#23716,#23717,
#23718,#23719,#23720,#23721,#23722,#23723,#23724,#23725,#23726,#23727,#23728,
#23729,#23730,#23731,#23732,#23733,#23734,#23735,#23736,#23737,#23738,#23739,
#23740,#23741,#23742,#23743,#23744,#23745,#23746,#23747,#23748,#23749,#23750,
#23751,#23752,#23753,#23754,#23755,#23756,#23757,#23758,#23759,#23760),
 .UNSPECIFIED.,.F.,.F.,(4,3,3,3,3,3,3,3,3,3,3,3,3,3,3,3,3,3,3,3,3,3,3,4),
(0.,0.079016546580938,0.157641122394585,0.183993443720854,0.207891281656444,
0.251131687956984,0.328243571587973,0.374168384090539,0.397099877179475,
0.472026294619315,0.492301725366521,0.550056206928688,0.568103933485432,
0.584735378149958,0.65759847554391,0.72331965161519,0.743939980328521,0.763679188248337,
0.809798919188833,0.846311488438111,0.867561854219163,0.937273050771799,
0.943726018375008,0.954382097139032),.UNSPECIFIED.);
#2264=B_SPLINE_CURVE_WITH_KNOTS('',3,(#23762,#23763,#23764,#23765,#23766,
#23767,#23768,#23769,#23770,#23771,#23772,#23773,#23774,#23775,#23776,#23777,
#23778),.UNSPECIFIED.,.F.,.F.,(4,1,1,1,1,1,1,1,1,1,1,1,1,1,4),(15.707963267949,
15.846983336647,16.3462383956745,16.845493454702,17.3447485137295,17.844003572757,
18.3432586317845,18.842513690812,19.3417687498395,19.841023808867,20.3402788678945,
20.839533926922,21.3387889859495,21.838044044977,21.9911485751285),
 .UNSPECIFIED.);
#2265=B_SPLINE_CURVE_WITH_KNOTS('',3,(#23779,#23780,#23781,#23782,#23783,
#23784,#23785,#23786,#23787,#23788,#23789,#23790,#23791,#23792,#23793,#23794,
#23795),.UNSPECIFIED.,.F.,.F.,(4,1,1,1,1,1,1,1,1,1,1,1,1,1,4),(15.707963267949,
15.8973745036305,16.396629562658,16.8958846216855,17.395139680713,17.8943947397405,
18.393649798768,18.8929048577955,19.392159916823,19.8914149758505,20.390670034878,
20.8899250939055,21.389180152933,21.8884352119605,21.9911485751285),
 .UNSPECIFIED.);
#2266=B_SPLINE_CURVE_WITH_KNOTS('',3,(#23992,#23993,#23994,#23995,#23996,
#23997,#23998,#23999,#24000,#24001,#24002,#24003,#24004,#24005,#24006,#24007,
#24008,#24009,#24010,#24011,#24012,#24013,#24014,#24015,#24016,#24017,#24018,
#24019,#24020,#24021,#24022,#24023,#24024,#24025,#24026,#24027,#24028,#24029,
#24030,#24031,#24032,#24033,#24034,#24035,#24036,#24037,#24038,#24039,#24040,
#24041,#24042,#24043,#24044,#24045,#24046,#24047,#24048,#24049,#24050,#24051,
#24052,#24053,#24054,#24055,#24056,#24057,#24058,#24059,#24060,#24061,#24062,
#24063,#24064),.UNSPECIFIED.,.F.,.F.,(4,3,3,3,3,3,3,3,3,3,3,3,3,3,3,3,3,
3,3,3,3,3,3,3,4),(-0.950777871811465,-0.888334407370769,-0.851051814776991,
-0.82737904373313,-0.764191528890905,-0.727096293545134,-0.707864357405063,
-0.701004014048681,-0.624532510230306,-0.548715306176616,-0.528886751702636,
-0.51335217329456,-0.460845815077925,-0.386468184274459,-0.349072714542667,
-0.331943455188318,-0.259671363135132,-0.230659644409349,-0.19743434794885,
-0.175120034180883,-0.157580682039417,-0.0841021758717334,-0.0150413926252008,
-0.0106236697040495,0.),.UNSPECIFIED.);
#2267=B_SPLINE_CURVE_WITH_KNOTS('',3,(#24065,#24066,#24067,#24068,#24069,
#24070,#24071,#24072,#24073,#24074,#24075,#24076,#24077,#24078,#24079,#24080,
#24081,#24082,#24083,#24084,#24085,#24086,#24087,#24088,#24089,#24090,#24091,
#24092,#24093,#24094,#24095,#24096,#24097,#24098,#24099,#24100,#24101,#24102,
#24103,#24104,#24105,#24106,#24107,#24108,#24109,#24110,#24111,#24112,#24113,
#24114,#24115,#24116,#24117,#24118,#24119,#24120,#24121,#24122,#24123,#24124,
#24125,#24126,#24127,#24128,#24129,#24130,#24131,#24132,#24133,#24134),
 .UNSPECIFIED.,.F.,.F.,(4,3,3,3,3,3,3,3,3,3,3,3,3,3,3,3,3,3,3,3,3,3,3,4),
(0.,0.0695167991119783,0.140212658431775,0.162172470483188,0.179979408684031,
0.219498223261391,0.291822018016311,0.337745303611425,0.355228583776568,
0.429645631566202,0.449180111380345,0.509263572656178,0.525649154341391,
0.601088264154331,0.677503858556246,0.688874999321038,0.709603483853625,
0.730479306054779,0.782399641108501,0.820902701806524,0.845385896033558,
0.924612288143001,0.938160646269666,0.950777871811463),.UNSPECIFIED.);
#2268=B_SPLINE_CURVE_WITH_KNOTS('',3,(#24135,#24136,#24137,#24138,#24139,
#24140,#24141,#24142,#24143,#24144,#24145,#24146,#24147,#24148,#24149,#24150,
#24151,#24152,#24153,#24154,#24155,#24156,#24157,#24158,#24159,#24160,#24161,
#24162,#24163,#24164,#24165,#24166,#24167,#24168,#24169,#24170,#24171,#24172,
#24173,#24174,#24175,#24176,#24177),.UNSPECIFIED.,.F.,.F.,(4,3,3,3,3,3,
3,3,3,3,3,3,3,3,4),(-10.1382057107016,-9.98510118055001,-9.48584612152251,
-8.98659106249501,-8.48733600346751,-7.98808094444001,-7.48882588541251,
-6.98957082638501,-6.49031576735751,-5.99106070833001,-5.49180564930251,
-4.99255059027501,-4.49329553124751,-3.99404047222001,-3.85502040352197),
 .UNSPECIFIED.);
#2269=B_SPLINE_CURVE_WITH_KNOTS('',3,(#24374,#24375,#24376,#24377,#24378,
#24379,#24380,#24381,#24382,#24383,#24384,#24385,#24386,#24387,#24388,#24389,
#24390,#24391,#24392,#24393,#24394,#24395,#24396,#24397,#24398,#24399,#24400,
#24401,#24402,#24403,#24404,#24405,#24406,#24407,#24408,#24409,#24410,#24411,
#24412,#24413,#24414,#24415,#24416,#24417,#24418,#24419,#24420,#24421,#24422,
#24423,#24424,#24425,#24426,#24427,#24428,#24429,#24430,#24431,#24432,#24433,
#24434,#24435,#24436,#24437,#24438,#24439,#24440,#24441,#24442,#24443),
 .UNSPECIFIED.,.F.,.F.,(4,3,3,3,3,3,3,3,3,3,3,3,3,3,3,3,3,3,3,3,3,3,3,4),
(-0.954382097139049,-0.899410408801335,-0.859358635307587,-0.836685957905282,
-0.785590650846737,-0.75140161257743,-0.734495343788191,-0.662158982507963,
-0.588787990221564,-0.570217280263643,-0.551422718402641,-0.504011712732237,
-0.443843717567291,-0.393584703400901,-0.372143080358795,-0.295059059270718,
-0.263339732072452,-0.224912725821683,-0.201648013648112,-0.183362315801792,
-0.105092336646239,-0.0261711118220366,-0.0126626251736613,0.),
 .UNSPECIFIED.);
#2270=B_SPLINE_CURVE_WITH_KNOTS('',3,(#24444,#24445,#24446,#24447,#24448,
#24449,#24450,#24451,#24452,#24453,#24454,#24455,#24456,#24457,#24458,#24459,
#24460,#24461,#24462,#24463,#24464,#24465,#24466,#24467,#24468,#24469,#24470,
#24471,#24472,#24473,#24474,#24475,#24476,#24477,#24478,#24479,#24480,#24481,
#24482,#24483),.UNSPECIFIED.,.F.,.F.,(4,3,3,3,3,3,3,3,3,3,3,3,3,4),(7.59153924858057,
7.98808094444002,8.48733600346752,8.98659106249502,9.48584612152252,9.98510118055002,
10.4843562395775,10.983611298605,11.4828663576325,11.98212141666,12.4813764756875,
12.980631534715,13.4798865937425,13.8747245557602),.UNSPECIFIED.);
#2271=B_SPLINE_CURVE_WITH_KNOTS('',3,(#24484,#24485,#24486,#24487,#24488,
#24489,#24490,#24491,#24492,#24493,#24494,#24495,#24496,#24497,#24498,#24499,
#24500,#24501,#24502,#24503,#24504,#24505,#24506,#24507,#24508,#24509,#24510,
#24511,#24512,#24513,#24514,#24515,#24516,#24517,#24518,#24519,#24520,#24521,
#24522,#24523,#24524,#24525,#24526,#24527,#24528,#24529,#24530,#24531,#24532,
#24533,#24534,#24535,#24536,#24537,#24538,#24539,#24540,#24541,#24542,#24543,
#24544,#24545,#24546,#24547,#24548,#24549,#24550,#24551,#24552,#24553),
 .UNSPECIFIED.,.F.,.F.,(4,3,3,3,3,3,3,3,3,3,3,3,3,3,3,3,3,3,3,3,3,3,3,4),
(0.,0.079016546580938,0.157641122394585,0.183993443720854,0.207891281656444,
0.251131687956984,0.328243571587973,0.374168384090539,0.397099877179475,
0.472026294619315,0.492301725366521,0.550056206928688,0.568103933485432,
0.584735378149958,0.65759847554391,0.72331965161519,0.743939980328521,0.763679188248337,
0.809798919188833,0.846311488438111,0.867561854219163,0.937273050771799,
0.943726018375008,0.954382097139032),.UNSPECIFIED.);
#2272=B_SPLINE_CURVE_WITH_KNOTS('',3,(#24569,#24570,#24571,#24572,#24573,
#24574,#24575,#24576,#24577,#24578,#24579,#24580,#24581,#24582,#24583,#24584,
#24585,#24586),.UNSPECIFIED.,.F.,.F.,(4,2,2,2,2,2,2,2,4),(0.,0.0759876362447371,
0.151975272489474,0.227927665609885,0.303880058730296,0.379832451850707,
0.455784844971118,0.531772481215855,0.607760117460592),.UNSPECIFIED.);
#2273=B_SPLINE_CURVE_WITH_KNOTS('',3,(#24587,#24588,#24589,#24590,#24591,
#24592,#24593,#24594,#24595,#24596,#24597,#24598,#24599,#24600,#24601,#24602,
#24603,#24604),.UNSPECIFIED.,.F.,.F.,(4,2,2,2,2,2,2,2,4),(0.607760117460592,
0.68374775370533,0.759735389950067,0.835687783070478,0.911640176190889,
0.9875925693113,1.06354496243171,1.13953259867645,1.21552023492118),
 .UNSPECIFIED.);
#2274=B_SPLINE_CURVE_WITH_KNOTS('',3,(#24609,#24610,#24611,#24612,#24613,
#24614,#24615,#24616,#24617,#24618,#24619,#24620,#24621),.UNSPECIFIED.,
 .F.,.F.,(4,2,3,2,2,4),(-0.408608378270607,-0.265388212066323,0.,0.265388212066323,
0.530776424132647,0.698056008856335),.UNSPECIFIED.);
#2275=B_SPLINE_CURVE_WITH_KNOTS('',3,(#24624,#24625,#24626,#24627,#24628,
#24629,#24630,#24631,#24632,#24633,#24634,#24635),.UNSPECIFIED.,.F.,.F.,
(4,2,2,2,2,4),(1.42476853019388,1.59204811491757,1.85743632698389,2.12282453905022,
2.38821275111654,2.53143291732083),.UNSPECIFIED.);
#2276=B_SPLINE_CURVE_WITH_KNOTS('',3,(#24669,#24670,#24671,#24672,#24673,
#24674,#24675,#24676,#24677,#24678,#24679,#24680,#24681),.UNSPECIFIED.,
 .F.,.F.,(4,2,3,2,2,4),(-0.408608378270607,-0.265388212066323,0.,0.265388212066323,
0.530776424132647,0.698056008856335),.UNSPECIFIED.);
#2277=B_SPLINE_CURVE_WITH_KNOTS('',3,(#24697,#24698,#24699,#24700,#24701,
#24702,#24703,#24704,#24705,#24706),.UNSPECIFIED.,.F.,.F.,(4,2,2,2,4),(0.303880058730296,
0.379832451850707,0.455784844971118,0.531772481215855,0.607760117460592),
 .UNSPECIFIED.);
#2278=B_SPLINE_CURVE_WITH_KNOTS('',3,(#24708,#24709,#24710,#24711,#24712,
#24713,#24714,#24715,#24716,#24717),.UNSPECIFIED.,.F.,.F.,(4,2,2,2,4),(0.,
0.0759876362447371,0.151975272489474,0.227927665609885,0.303880058730296),
 .UNSPECIFIED.);
#2279=B_SPLINE_CURVE_WITH_KNOTS('',3,(#24719,#24720,#24721,#24722,#24723,
#24724,#24725,#24726,#24727,#24728),.UNSPECIFIED.,.F.,.F.,(4,2,2,2,4),(0.911640176190889,
0.9875925693113,1.06354496243171,1.13953259867645,1.21552023492118),
 .UNSPECIFIED.);
#2280=B_SPLINE_CURVE_WITH_KNOTS('',3,(#24729,#24730,#24731,#24732,#24733,
#24734,#24735,#24736,#24737,#24738),.UNSPECIFIED.,.F.,.F.,(4,2,2,2,4),(0.607760117460592,
0.68374775370533,0.759735389950067,0.835687783070478,0.911640176190889),
 .UNSPECIFIED.);
#2281=B_SPLINE_CURVE_WITH_KNOTS('',3,(#24742,#24743,#24744,#24745,#24746,
#24747,#24748,#24749,#24750,#24751,#24752,#24753),.UNSPECIFIED.,.F.,.F.,
(4,2,2,2,2,4),(1.42476853019388,1.59204811491757,1.85743632698389,2.12282453905022,
2.38821275111654,2.53143291732083),.UNSPECIFIED.);
#2282=B_SPLINE_CURVE_WITH_KNOTS('',3,(#24821,#24822,#24823,#24824,#24825,
#24826,#24827,#24828,#24829,#24830,#24831,#24832,#24833,#24834,#24835,#24836,
#24837,#24838,#24839,#24840,#24841,#24842),.UNSPECIFIED.,.F.,.F.,(4,3,3,
3,3,3,3,4),(76.7080459413271,76.8129957196859,77.8105670926688,78.8081384656518,
79.8057098386347,80.8032812116176,81.8008525846005,82.7984239575835),
 .UNSPECIFIED.);
#2283=B_SPLINE_CURVE_WITH_KNOTS('',3,(#24846,#24847,#24848,#24849,#24850,
#24851,#24852),.UNSPECIFIED.,.F.,.F.,(4,3,4),(-80.783811092309,-79.8057098386347,
-79.2446069498474),.UNSPECIFIED.);
#2284=B_SPLINE_CURVE_WITH_KNOTS('',3,(#24856,#24857,#24858,#24859,#24860,
#24861,#24862,#24863,#24864,#24865,#24866,#24867,#24868,#24869,#24870,#24871,
#24872,#24873,#24874,#24875,#24876,#24877),.UNSPECIFIED.,.F.,.F.,(4,3,3,
3,3,3,3,4),(-79.2446069498474,-78.8081384656518,-77.8105670926689,-76.8129957196859,
-75.815424346703,-74.81785297372,-73.8202816007371,-72.9614216426678),
 .UNSPECIFIED.);
#2285=B_SPLINE_CURVE_WITH_KNOTS('',3,(#24882,#24883,#24884,#24885,#24886,
#24887,#24888,#24889,#24890,#24891,#24892,#24893,#24894,#24895,#24896,#24897,
#24898,#24899,#24900,#24901,#24902,#24903),.UNSPECIFIED.,.F.,.F.,(4,3,3,
3,3,3,3,4),(70.4248606341475,70.8275674817883,71.8251388547712,72.8227102277541,
73.8202816007371,74.81785297372,75.815424346703,76.7080459413271),
 .UNSPECIFIED.);
#2286=B_SPLINE_CURVE_WITH_KNOTS('',3,(#24904,#24905,#24906,#24907,#24908,
#24909,#24910,#24911,#24912,#24913,#24914,#24915,#24916,#24917,#24918,#24919,
#24920,#24921,#24922,#24923,#24924,#24925,#24926,#24927,#24928),
 .UNSPECIFIED.,.F.,.F.,(4,3,3,3,3,3,3,3,4),(-72.9614216426678,-72.8227102277542,
-71.8251388547712,-70.8275674817883,-69.8299961088054,-68.8324247358224,
-67.8348533628395,-66.8372819898566,-66.6782363354882),.UNSPECIFIED.);
#2287=B_SPLINE_CURVE_WITH_KNOTS('',3,(#24933,#24934,#24935,#24936,#24937,
#24938,#24939,#24940,#24941,#24942,#24943,#24944,#24945,#24946,#24947,#24948,
#24949,#24950,#24951,#24952,#24953,#24954),.UNSPECIFIED.,.F.,.F.,(4,3,3,
3,3,3,3,4),(64.1416753269679,64.8421392438907,65.8397106168736,66.8372819898565,
67.8348533628395,68.8324247358224,69.8299961088054,70.4248606341475),
 .UNSPECIFIED.);
#2288=B_SPLINE_CURVE_WITH_KNOTS('',3,(#24955,#24956,#24957,#24958,#24959,
#24960,#24961,#24962,#24963,#24964,#24965,#24966,#24967,#24968,#24969,#24970,
#24971,#24972,#24973,#24974,#24975,#24976),.UNSPECIFIED.,.F.,.F.,(4,3,3,
3,3,3,3,4),(-66.6782363354882,-65.8397106168736,-64.8421392438907,-63.8445678709078,
-62.8469964979248,-61.8494251249419,-60.851853751959,-60.3950510283086),
 .UNSPECIFIED.);
#2289=B_SPLINE_CURVE_WITH_KNOTS('',3,(#24981,#24982,#24983,#24984,#24985,
#24986,#24987,#24988,#24989,#24990,#24991,#24992,#24993,#24994,#24995,#24996,
#24997,#24998,#24999,#25000,#25001,#25002),.UNSPECIFIED.,.F.,.F.,(4,3,3,
3,3,3,3,4),(57.8584900197883,58.8567110059931,59.854282378976,60.851853751959,
61.8494251249419,62.8469964979248,63.8445678709078,64.1416753269679),
 .UNSPECIFIED.);
#2290=B_SPLINE_CURVE_WITH_KNOTS('',3,(#25003,#25004,#25005,#25006,#25007,
#25008,#25009,#25010,#25011,#25012,#25013,#25014,#25015,#25016,#25017,#25018,
#25019,#25020,#25021,#25022,#25023,#25024),.UNSPECIFIED.,.F.,.F.,(4,3,3,
3,3,3,3,4),(-60.3950510283086,-59.8542823789761,-58.8567110059931,-57.8591396330102,
-56.8615682600272,-55.8639968870443,-54.8664255140614,-54.111865721129),
 .UNSPECIFIED.);
#2291=B_SPLINE_CURVE_WITH_KNOTS('',3,(#25029,#25030,#25031,#25032,#25033,
#25034,#25035,#25036,#25037,#25038,#25039,#25040,#25041,#25042,#25043,#25044,
#25045,#25046,#25047,#25048,#25049,#25050),.UNSPECIFIED.,.F.,.F.,(4,3,3,
3,3,3,3,4),(51.5753047126088,51.8737113951125,52.8712827680955,53.8688541410784,
54.8664255140613,55.8639968870443,56.8615682600272,57.8584900197883),
 .UNSPECIFIED.);
#2292=B_SPLINE_CURVE_WITH_KNOTS('',3,(#25051,#25052,#25053,#25054,#25055,
#25056,#25057,#25058,#25059,#25060,#25061,#25062,#25063,#25064,#25065,#25066,
#25067,#25068,#25069,#25070,#25071,#25072,#25073,#25074,#25075),
 .UNSPECIFIED.,.F.,.F.,(4,3,3,3,3,3,3,3,4),(-54.111865721129,-53.8688541410784,
-52.8712827680955,-51.8737113951126,-50.8761400221296,-49.8785686491467,
-48.8809972761638,-47.8834259031808,-47.8286804139494),.UNSPECIFIED.);
#2293=B_SPLINE_CURVE_WITH_KNOTS('',3,(#25080,#25081,#25082,#25083,#25084,
#25085,#25086,#25087,#25088,#25089,#25090,#25091,#25092,#25093,#25094,#25095,
#25096,#25097,#25098,#25099,#25100,#25101),.UNSPECIFIED.,.F.,.F.,(4,3,3,
3,3,3,3,4),(45.2921194054292,45.8882831572149,46.8858545301979,47.8834259031808,
48.8809972761637,49.8785686491467,50.8761400221296,51.5753047126088),
 .UNSPECIFIED.);
#2294=B_SPLINE_CURVE_WITH_KNOTS('',3,(#25102,#25103,#25104,#25105,#25106,
#25107,#25108,#25109,#25110,#25111,#25112,#25113,#25114,#25115,#25116,#25117,
#25118,#25119,#25120,#25121,#25122,#25123),.UNSPECIFIED.,.F.,.F.,(4,3,3,
3,3,3,3,4),(-47.8286804139494,-46.8858545301979,-45.888283157215,-44.890711784232,
-43.8931404112491,-42.8955690382662,-41.8979976652832,-41.5454951067698),
 .UNSPECIFIED.);
#2295=B_SPLINE_CURVE_WITH_KNOTS('',3,(#25128,#25129,#25130,#25131,#25132,
#25133,#25134,#25135,#25136,#25137,#25138,#25139,#25140,#25141,#25142,#25143,
#25144,#25145,#25146,#25147,#25148,#25149),.UNSPECIFIED.,.F.,.F.,(4,3,3,
3,3,3,3,4),(39.0089340982495,39.9028549193173,40.9004262923003,41.8979976652832,
42.8955690382661,43.8931404112491,44.890711784232,45.2921194054292),
 .UNSPECIFIED.);
#2296=B_SPLINE_CURVE_WITH_KNOTS('',3,(#25150,#25151,#25152,#25153,#25154,
#25155,#25156,#25157,#25158,#25159,#25160,#25161,#25162,#25163,#25164,#25165,
#25166,#25167,#25168,#25169,#25170,#25171),.UNSPECIFIED.,.F.,.F.,(4,3,3,
3,3,3,3,4),(-41.5454951067698,-40.9004262923003,-39.9028549193174,-38.9052835463344,
-37.9077121733515,-36.9101408003686,-35.9125694273856,-35.2623097995902),
 .UNSPECIFIED.);
#2297=B_SPLINE_CURVE_WITH_KNOTS('',3,(#25176,#25177,#25178,#25179,#25180,
#25181,#25182,#25183,#25184,#25185,#25186,#25187,#25188,#25189,#25190,#25191,
#25192,#25193,#25194,#25195,#25196,#25197,#25198,#25199,#25200),
 .UNSPECIFIED.,.F.,.F.,(4,3,3,3,3,3,3,3,4),(32.7257487910699,32.9198553084368,
33.9174266814197,34.9149980544027,35.9125694273856,36.9101408003685,37.9077121733515,
38.9052835463344,39.0089340982495),.UNSPECIFIED.);
#2298=B_SPLINE_CURVE_WITH_KNOTS('',3,(#25201,#25202,#25203,#25204,#25205,
#25206,#25207,#25208,#25209,#25210,#25211,#25212,#25213,#25214,#25215,#25216,
#25217,#25218,#25219,#25220,#25221,#25222),.UNSPECIFIED.,.F.,.F.,(4,3,3,
3,3,3,3,4),(-35.2623097995902,-34.9149980544027,-33.9174266814197,-32.9198553084368,
-31.9222839354539,-30.924712562471,-29.927141189488,-28.9791244924107),
 .UNSPECIFIED.);
#2299=B_SPLINE_CURVE_WITH_KNOTS('',3,(#25227,#25228,#25229,#25230,#25231,
#25232,#25233,#25234,#25235,#25236,#25237,#25238,#25239,#25240,#25241,#25242,
#25243,#25244,#25245,#25246,#25247,#25248),.UNSPECIFIED.,.F.,.F.,(4,3,3,
3,3,3,3,4),(26.4425634838903,26.9344270705392,27.9319984435221,28.9295698165051,
29.927141189488,30.9247125624709,31.9222839354539,32.7257487910699),
 .UNSPECIFIED.);
#2300=B_SPLINE_CURVE_WITH_KNOTS('',3,(#25249,#25250,#25251,#25252,#25253,
#25254,#25255,#25256,#25257,#25258,#25259,#25260,#25261,#25262,#25263,#25264,
#25265,#25266,#25267,#25268,#25269,#25270,#25271,#25272,#25273),
 .UNSPECIFIED.,.F.,.F.,(4,3,3,3,3,3,3,3,4),(-28.9791244924107,-28.9295698165051,
-27.9319984435222,-26.9344270705392,-25.9368556975563,-24.9392843245734,
-23.9417129515904,-22.9441415786075,-22.6959391852311),.UNSPECIFIED.);
#2301=B_SPLINE_CURVE_WITH_KNOTS('',3,(#25278,#25279,#25280,#25281,#25282,
#25283,#25284,#25285,#25286,#25287,#25288,#25289,#25290,#25291,#25292,#25293,
#25294,#25295,#25296,#25297,#25298,#25299),.UNSPECIFIED.,.F.,.F.,(4,3,3,
3,3,3,3,4),(20.1593781767107,20.9489988326416,21.9465702056245,22.9441415786075,
23.9417129515904,24.9392843245733,25.9368556975563,26.4425634838903),
 .UNSPECIFIED.);
#2302=B_SPLINE_CURVE_WITH_KNOTS('',3,(#25300,#25301,#25302,#25303,#25304,
#25305,#25306,#25307,#25308,#25309,#25310,#25311,#25312,#25313,#25314,#25315,
#25316,#25317,#25318,#25319,#25320,#25321),.UNSPECIFIED.,.F.,.F.,(4,3,3,
3,3,3,3,4),(-22.6959391852311,-21.9465702056245,-20.9489988326416,-19.9514274596587,
-18.9538560866757,-17.9562847136928,-16.9587133407099,-16.4127538780515),
 .UNSPECIFIED.);
#2303=B_SPLINE_CURVE_WITH_KNOTS('',3,(#25326,#25327,#25328,#25329,#25330,
#25331,#25332,#25333,#25334,#25335,#25336,#25337,#25338,#25339,#25340,#25341,
#25342,#25343,#25344,#25345,#25346,#25347,#25348,#25349,#25350),
 .UNSPECIFIED.,.F.,.F.,(4,3,3,3,3,3,3,3,4),(13.8761928695313,13.9659992217611,
14.963570594744,15.9611419677269,16.9587133407099,17.9562847136928,18.9538560866757,
19.9514274596587,20.1593781767107),.UNSPECIFIED.);
#2304=B_SPLINE_CURVE_WITH_KNOTS('',3,(#25351,#25352,#25353,#25354,#25355,
#25356,#25357,#25358,#25359,#25360,#25361,#25362,#25363,#25364,#25365,#25366,
#25367,#25368,#25369,#25370,#25371,#25372),.UNSPECIFIED.,.F.,.F.,(4,3,3,
3,3,3,3,4),(-16.4127538780515,-15.9611419677269,-14.963570594744,-13.9659992217611,
-12.9684278487781,-11.9708564757952,-10.9732851028123,-10.1295685708719),
 .UNSPECIFIED.);
#2305=B_SPLINE_CURVE_WITH_KNOTS('',3,(#25378,#25379,#25380,#25381,#25382,
#25383,#25384,#25385,#25386,#25387,#25388,#25389,#25390),.UNSPECIFIED.,
 .F.,.F.,(4,3,3,3,4),(-3.84638326369226,-2.9927141189488,-1.99514274596587,
-0.997571372982934,0.),.UNSPECIFIED.);
#2306=B_SPLINE_CURVE_WITH_KNOTS('',3,(#25393,#25394,#25395,#25396,#25397,
#25398,#25399,#25400,#25401,#25402,#25403,#25404,#25405,#25406,#25407,#25408,
#25409,#25410,#25411),.UNSPECIFIED.,.F.,.F.,(4,3,3,3,3,3,4),(2.01461286527449,
2.9927141189488,3.99028549193173,4.98785686491467,5.9854282378976,6.98299961088053,
7.59300756235165),.UNSPECIFIED.);
#2307=B_SPLINE_CURVE_WITH_KNOTS('',3,(#25417,#25418,#25419,#25420,#25421,
#25422,#25423),.UNSPECIFIED.,.F.,.F.,(4,1,1,1,4),(91.106186954104,91.6672898428913,
92.6648612158743,93.6624325888572,94.6600039618401),.UNSPECIFIED.);
#2308=B_SPLINE_CURVE_WITH_KNOTS('',3,(#25426,#25427,#25428,#25429,#25430,
#25431,#25432,#25433),.UNSPECIFIED.,.F.,.F.,(4,1,1,1,1,4),(91.106186954104,
91.2111367324627,92.2087081054457,93.2062794784286,94.2038508514115,95.1819521050858),
 .UNSPECIFIED.);
#2309=B_SPLINE_CURVE_WITH_KNOTS('',3,(#25438,#25439,#25440,#25441,#25442,
#25443,#25444,#25445,#25446,#25447),.UNSPECIFIED.,.F.,.F.,(4,1,1,1,1,1,
1,4),(84.8230016469244,85.6818616049937,86.6794329779766,87.6770043509596,
88.6745757239425,89.6721470969255,90.6697184699084,91.106186954104),
 .UNSPECIFIED.);
#2310=B_SPLINE_CURVE_WITH_KNOTS('',3,(#25448,#25449,#25450,#25451,#25452,
#25453,#25454,#25455,#25456,#25457),.UNSPECIFIED.,.F.,.F.,(4,1,1,1,1,1,
1,4),(84.8230016469244,85.2257084945651,86.2232798675481,87.220851240531,
88.2184226135139,89.2159939864968,90.2135653594798,91.106186954104),
 .UNSPECIFIED.);
#2311=B_SPLINE_CURVE_WITH_KNOTS('',3,(#25462,#25463,#25464,#25465,#25466,
#25467,#25468,#25469,#25470,#25471,#25472),.UNSPECIFIED.,.F.,.F.,(4,1,1,
1,1,1,1,1,4),(78.5398163397448,78.6988619941132,79.6964333670961,80.6940047400791,
81.691576113062,82.6891474860449,83.6867188590278,84.6842902320108,84.8230016469244),
 .UNSPECIFIED.);
#2312=B_SPLINE_CURVE_WITH_KNOTS('',3,(#25473,#25474,#25475,#25476,#25477,
#25478,#25479,#25480,#25481,#25482),.UNSPECIFIED.,.F.,.F.,(4,1,1,1,1,1,
1,4),(78.5398163397448,79.2402802566675,80.2378516296505,81.2354230026334,
82.2329943756163,83.2305657485992,84.2281371215822,84.8230016469244),
 .UNSPECIFIED.);
#2313=B_SPLINE_CURVE_WITH_KNOTS('',3,(#25487,#25488,#25489,#25490,#25491,
#25492,#25493,#25494,#25495,#25496),.UNSPECIFIED.,.F.,.F.,(4,1,1,1,1,1,
1,4),(72.2566310325652,72.7134337562156,73.7110051291985,74.7085765021814,
75.7061478751644,76.7037192481473,77.7012906211302,78.5398163397448),
 .UNSPECIFIED.);
#2314=B_SPLINE_CURVE_WITH_KNOTS('',3,(#25497,#25498,#25499,#25500,#25501,
#25502,#25503,#25504,#25505,#25506,#25507),.UNSPECIFIED.,.F.,.F.,(4,1,1,
1,1,1,1,1,4),(72.2566310325652,72.257280645787,73.2548520187699,74.2524233917528,
75.2499947647358,76.2475661377187,77.2451375107017,78.2427088836846,78.5398163397448),
 .UNSPECIFIED.);
#2315=B_SPLINE_CURVE_WITH_KNOTS('',3,(#25512,#25513,#25514,#25515,#25516,
#25517,#25518,#25519,#25520,#25521),.UNSPECIFIED.,.F.,.F.,(4,1,1,1,1,1,
1,4),(65.9734457253856,66.728005518318,67.7255768913009,68.7231482642838,
69.7207196372668,70.7182910102497,71.7158623832326,72.2566310325652),
 .UNSPECIFIED.);
#2316=B_SPLINE_CURVE_WITH_KNOTS('',3,(#25522,#25523,#25524,#25525,#25526,
#25527,#25528,#25529,#25530,#25531),.UNSPECIFIED.,.F.,.F.,(4,1,1,1,1,1,
1,4),(65.9734457253856,66.2718524078894,67.2694237808723,68.2669951538552,
69.2645665268382,70.2621378998211,71.2597092728041,72.2566310325652),
 .UNSPECIFIED.);
#2317=B_SPLINE_CURVE_WITH_KNOTS('',3,(#25536,#25537,#25538,#25539,#25540,
#25541,#25542,#25543,#25544,#25545,#25546),.UNSPECIFIED.,.F.,.F.,(4,1,1,
1,1,1,1,1,4),(59.690260418206,59.7450059074374,60.7425772804204,61.7401486534033,
62.7377200263862,63.7352913993692,64.7328627723521,65.730434145335,65.9734457253856),
 .UNSPECIFIED.);
#2318=B_SPLINE_CURVE_WITH_KNOTS('',3,(#25547,#25548,#25549,#25550,#25551,
#25552,#25553,#25554,#25555,#25556),.UNSPECIFIED.,.F.,.F.,(4,1,1,1,1,1,
1,4),(59.690260418206,60.2864241699918,61.2839955429747,62.2815669159576,
63.2791382889406,64.2767096619235,65.2742810349065,65.9734457253856),
 .UNSPECIFIED.);
#2319=B_SPLINE_CURVE_WITH_KNOTS('',3,(#25561,#25562,#25563,#25564,#25565,
#25566,#25567,#25568,#25569,#25570),.UNSPECIFIED.,.F.,.F.,(4,1,1,1,1,1,
1,4),(53.4070751110264,53.7595776695398,54.7571490425228,55.7547204155057,
56.7522917884886,57.7498631614716,58.7474345344545,59.690260418206),
 .UNSPECIFIED.);
#2320=B_SPLINE_CURVE_WITH_KNOTS('',3,(#25571,#25572,#25573,#25574,#25575,
#25576,#25577,#25578,#25579,#25580),.UNSPECIFIED.,.F.,.F.,(4,1,1,1,1,1,
1,4),(53.4070751110264,54.3009959320942,55.2985673050771,56.29613867806,
57.293710051043,58.2912814240259,59.2888527970089,59.690260418206),
 .UNSPECIFIED.);
#2321=B_SPLINE_CURVE_WITH_KNOTS('',3,(#25585,#25586,#25587,#25588,#25589,
#25590,#25591,#25592,#25593,#25594),.UNSPECIFIED.,.F.,.F.,(4,1,1,1,1,1,
1,4),(47.1238898038468,47.7741494316422,48.7717208046252,49.7692921776081,
50.766863550591,51.764434923574,52.7620062965569,53.4070751110264),
 .UNSPECIFIED.);
#2322=B_SPLINE_CURVE_WITH_KNOTS('',3,(#25595,#25596,#25597,#25598,#25599,
#25600,#25601,#25602,#25603,#25604,#25605),.UNSPECIFIED.,.F.,.F.,(4,1,1,
1,1,1,1,1,4),(47.1238898038468,47.3179963212136,48.3155676941966,49.3131390671795,
50.3107104401624,51.3082818131454,52.3058531861283,53.3034245591112,53.4070751110264),
 .UNSPECIFIED.);
#2323=B_SPLINE_CURVE_WITH_KNOTS('',3,(#25610,#25611,#25612,#25613,#25614,
#25615,#25616,#25617,#25618,#25619),.UNSPECIFIED.,.F.,.F.,(4,1,1,1,1,1,
1,4),(40.8407044966672,41.7887211937446,42.7862925667276,43.7838639397105,
44.7814353126934,45.7790066856764,46.7765780586593,47.1238898038468),
 .UNSPECIFIED.);
#2324=B_SPLINE_CURVE_WITH_KNOTS('',3,(#25620,#25621,#25622,#25623,#25624,
#25625,#25626,#25627,#25628,#25629),.UNSPECIFIED.,.F.,.F.,(4,1,1,1,1,1,
1,4),(40.8407044966672,41.332568083316,42.330139456299,43.3277108292819,
44.3252822022648,45.3228535752478,46.3204249482307,47.1238898038468),
 .UNSPECIFIED.);
#2325=B_SPLINE_CURVE_WITH_KNOTS('',3,(#25634,#25635,#25636,#25637,#25638,
#25639,#25640,#25641,#25642,#25643,#25644),.UNSPECIFIED.,.F.,.F.,(4,1,1,
1,1,1,1,1,4),(34.5575191894877,34.8057215828641,35.803292955847,36.80086432883,
37.7984357018129,38.7960070747958,39.7935784477788,40.7911498207617,40.8407044966672),
 .UNSPECIFIED.);
#2326=B_SPLINE_CURVE_WITH_KNOTS('',3,(#25645,#25646,#25647,#25648,#25649,
#25650,#25651,#25652,#25653,#25654),.UNSPECIFIED.,.F.,.F.,(4,1,1,1,1,1,
1,4),(34.5575191894877,35.3471398454184,36.3447112184014,37.3422825913843,
38.3398539643672,39.3374253373502,40.3349967103331,40.8407044966672),
 .UNSPECIFIED.);
#2327=B_SPLINE_CURVE_WITH_KNOTS('',3,(#25659,#25660,#25661,#25662,#25663,
#25664,#25665,#25666,#25667,#25668),.UNSPECIFIED.,.F.,.F.,(4,1,1,1,1,1,
1,4),(28.2743338823081,28.8202933449665,29.8178647179494,30.8154360909324,
31.8130074639153,32.8105788368982,33.8081502098812,34.5575191894877),
 .UNSPECIFIED.);
#2328=B_SPLINE_CURVE_WITH_KNOTS('',3,(#25669,#25670,#25671,#25672,#25673,
#25674,#25675,#25676,#25677,#25678,#25679),.UNSPECIFIED.,.F.,.F.,(4,1,1,
1,1,1,1,1,4),(28.2743338823081,28.3641402345379,29.3617116075208,30.3592829805038,
31.3568543534867,32.3544257264696,33.3519970994526,34.3495684724355,34.5575191894877),
 .UNSPECIFIED.);
#2329=B_SPLINE_CURVE_WITH_KNOTS('',3,(#25684,#25685,#25686,#25687,#25688,
#25689,#25690,#25691,#25692,#25693),.UNSPECIFIED.,.F.,.F.,(4,1,1,1,1,1,
1,4),(21.9911485751285,22.8348651070689,23.8324364800518,24.8300078530348,
25.8275792260177,26.8251505990006,27.8227219719836,28.2743338823081),
 .UNSPECIFIED.);
#2330=B_SPLINE_CURVE_WITH_KNOTS('',3,(#25694,#25695,#25696,#25697,#25698,
#25699,#25700,#25701,#25702,#25703),.UNSPECIFIED.,.F.,.F.,(4,1,1,1,1,1,
1,4),(21.9911485751285,22.3787119966403,23.3762833696232,24.3738547426062,
25.3714261155891,26.368997488572,27.366568861555,28.2743338823081),
 .UNSPECIFIED.);
#2331=B_SPLINE_CURVE_WITH_KNOTS('',3,(#25709,#25710,#25711,#25712,#25713),
 .UNSPECIFIED.,.F.,.F.,(4,1,4),(14.3981410127768,15.3957123857598,15.7079632679489),
 .UNSPECIFIED.);
#2332=B_SPLINE_CURVE_WITH_KNOTS('',3,(#25716,#25717,#25718,#25719,#25720),
 .UNSPECIFIED.,.F.,.F.,(4,1,4),(13.8761928695311,14.8542941232054,15.7079632679489),
 .UNSPECIFIED.);
#2333=B_SPLINE_CURVE_WITH_KNOTS('',3,(#25726,#25727,#25728,#25729),
 .UNSPECIFIED.,.F.,.F.,(4,4),(51.5750455984138,52.2860549491936),
 .UNSPECIFIED.);
#2334=B_SPLINE_CURVE_WITH_KNOTS('',3,(#25732,#25733,#25734,#25735,#25736,
#25737,#25738,#25739,#25740,#25741),.UNSPECIFIED.,.F.,.F.,(4,3,3,4),(-50.2654824574367,
-49.3264669332015,-48.3399375945375,-47.8348991546268),.UNSPECIFIED.);
#2335=B_SPLINE_CURVE_WITH_KNOTS('',3,(#25746,#25747,#25748,#25749,#25750,
#25751,#25752,#25753,#25754,#25755,#25756,#25757,#25758,#25759,#25760,#25761,
#25762,#25763,#25764,#25765,#25766,#25767,#25768,#25769,#25770),
 .UNSPECIFIED.,.F.,.F.,(4,3,3,3,3,3,3,3,4),(45.2918602912342,45.3803495785454,
46.3668789172094,47.3534082558735,48.3399375945375,49.3264669332015,50.3129962718656,
51.2995256105296,51.5750455984138),.UNSPECIFIED.);
#2336=B_SPLINE_CURVE_WITH_KNOTS('',3,(#25771,#25772,#25773,#25774,#25775,
#25776,#25777,#25778,#25779,#25780,#25781,#25782,#25783,#25784,#25785,#25786,
#25787,#25788,#25789,#25790,#25791,#25792),.UNSPECIFIED.,.F.,.F.,(4,3,3,
3,3,3,3,4),(-47.8348991546268,-47.3534082558735,-46.3668789172095,-45.3803495785454,
-44.3938202398814,-43.4072909012174,-42.4207615625533,-41.5517138474472),
 .UNSPECIFIED.);
#2337=B_SPLINE_CURVE_WITH_KNOTS('',3,(#25797,#25798,#25799,#25800,#25801,
#25802,#25803,#25804,#25805,#25806,#25807,#25808,#25809,#25810,#25811,#25812,
#25813,#25814,#25815,#25816,#25817,#25818),.UNSPECIFIED.,.F.,.F.,(4,3,3,
3,3,3,3,4),(39.0086749840546,39.4611735465612,40.4477028852253,41.4342322238893,
42.4207615625533,43.4072909012174,44.3938202398814,45.2918602912342),
 .UNSPECIFIED.);
#2338=B_SPLINE_CURVE_WITH_KNOTS('',3,(#25819,#25820,#25821,#25822,#25823,
#25824,#25825,#25826,#25827,#25828,#25829,#25830,#25831,#25832,#25833,#25834,
#25835,#25836,#25837,#25838,#25839,#25840,#25841,#25842,#25843),
 .UNSPECIFIED.,.F.,.F.,(4,3,3,3,3,3,3,3,4),(-41.5517138474472,-41.4342322238893,
-40.4477028852253,-39.4611735465612,-38.4746442078972,-37.4881148692332,
-36.5015855305691,-35.5150561919051,-35.2685285402676),.UNSPECIFIED.);
#2339=B_SPLINE_CURVE_WITH_KNOTS('',3,(#25848,#25849,#25850,#25851,#25852,
#25853,#25854,#25855,#25856,#25857,#25858,#25859,#25860,#25861,#25862,#25863,
#25864,#25865,#25866,#25867,#25868,#25869),.UNSPECIFIED.,.F.,.F.,(4,3,3,
3,3,3,3,4),(32.725489676875,33.541997514577,34.5285268532411,35.5150561919051,
36.5015855305691,37.4881148692332,38.4746442078972,39.0086749840546),
 .UNSPECIFIED.);
#2340=B_SPLINE_CURVE_WITH_KNOTS('',3,(#25870,#25871,#25872,#25873,#25874,
#25875,#25876,#25877,#25878,#25879,#25880,#25881,#25882,#25883,#25884,#25885,
#25886,#25887,#25888,#25889,#25890,#25891),.UNSPECIFIED.,.F.,.F.,(4,3,3,
3,3,3,3,4),(-35.2685285402676,-34.5285268532411,-33.541997514577,-32.555468175913,
-31.568938837249,-30.582409498585,-29.5958801599209,-28.985343233088),
 .UNSPECIFIED.);
#2341=B_SPLINE_CURVE_WITH_KNOTS('',3,(#25896,#25897,#25898,#25899,#25900,
#25901,#25902,#25903,#25904,#25905,#25906,#25907,#25908,#25909,#25910,#25911,
#25912,#25913,#25914,#25915,#25916,#25917,#25918,#25919,#25920),
 .UNSPECIFIED.,.F.,.F.,(4,3,3,3,3,3,3,3,4),(26.4423043696954,26.6362921439288,
27.6228214825929,28.6093508212569,29.5958801599209,30.582409498585,31.568938837249,
32.555468175913,32.725489676875),.UNSPECIFIED.);
#2342=B_SPLINE_CURVE_WITH_KNOTS('',3,(#25921,#25922,#25923,#25924,#25925,
#25926,#25927,#25928,#25929,#25930,#25931,#25932,#25933,#25934,#25935,#25936,
#25937,#25938,#25939,#25940,#25941,#25942),.UNSPECIFIED.,.F.,.F.,(4,3,3,
3,3,3,3,4),(-28.985343233088,-28.6093508212569,-27.6228214825929,-26.6362921439288,
-25.6497628052648,-24.6632334666008,-23.6767041279367,-22.7021579259084),
 .UNSPECIFIED.);
#2343=B_SPLINE_CURVE_WITH_KNOTS('',3,(#25947,#25948,#25949,#25950,#25951,
#25952,#25953,#25954,#25955,#25956,#25957,#25958,#25959,#25960,#25961,#25962,
#25963,#25964,#25965,#25966,#25967,#25968),.UNSPECIFIED.,.F.,.F.,(4,3,3,
3,3,3,3,4),(20.1591190625159,20.7171161119446,21.7036454506087,22.6901747892727,
23.6767041279367,24.6632334666008,25.6497628052648,26.4423043696954),
 .UNSPECIFIED.);
#2344=B_SPLINE_CURVE_WITH_KNOTS('',3,(#25969,#25970,#25971,#25972,#25973,
#25974,#25975,#25976,#25977,#25978,#25979,#25980,#25981,#25982,#25983,#25984,
#25985,#25986,#25987,#25988,#25989,#25990,#25991,#25992,#25993),
 .UNSPECIFIED.,.F.,.F.,(4,3,3,3,3,3,3,3,4),(-22.7021579259084,-22.6901747892727,
-21.7036454506087,-20.7171161119446,-19.7305867732806,-18.7440574346166,
-17.7575280959526,-16.7709987572885,-16.4189726187288),.UNSPECIFIED.);
#2345=B_SPLINE_CURVE_WITH_KNOTS('',3,(#25998,#25999,#26000,#26001,#26002,
#26003,#26004,#26005,#26006,#26007,#26008,#26009,#26010,#26011,#26012,#26013,
#26014,#26015,#26016,#26017,#26018,#26019),.UNSPECIFIED.,.F.,.F.,(4,3,3,
3,3,3,3,4),(13.8759337553363,14.7979400799605,15.7844694186245,16.7709987572885,
17.7575280959526,18.7440574346166,19.7305867732806,20.1591190625159),
 .UNSPECIFIED.);
#2346=B_SPLINE_CURVE_WITH_KNOTS('',3,(#26020,#26021,#26022,#26023,#26024,
#26025,#26026,#26027,#26028,#26029,#26030,#26031,#26032,#26033,#26034,#26035,
#26036,#26037,#26038,#26039,#26040,#26041),.UNSPECIFIED.,.F.,.F.,(4,3,3,
3,3,3,3,4),(-16.4189726187288,-15.7844694186245,-14.7979400799605,-13.8114107412964,
-12.8248814026324,-11.8383520639684,-10.8518227253043,-10.1357873115492),
 .UNSPECIFIED.);
#2347=B_SPLINE_CURVE_WITH_KNOTS('',3,(#26047,#26048,#26049,#26050,#26051,
#26052,#26053,#26054,#26055,#26056,#26057,#26058,#26059),.UNSPECIFIED.,
 .F.,.F.,(4,3,3,3,4),(-3.85260200436966,-2.95958801599209,-1.97305867732806,
-0.986529338664031,0.),.UNSPECIFIED.);
#2348=B_SPLINE_CURVE_WITH_KNOTS('',3,(#26062,#26063,#26064,#26065,#26066,
#26067,#26068,#26069,#26070,#26071,#26072,#26073,#26074,#26075,#26076,#26077,
#26078,#26079,#26080),.UNSPECIFIED.,.F.,.F.,(4,3,3,3,3,3,4),(2.0205724917569,
2.95958801599209,3.94611735465613,4.93264669332016,5.91917603198418,6.90570537064821,
7.5927484481567),.UNSPECIFIED.);
#2349=B_SPLINE_CURVE_WITH_KNOTS('',3,(#26086,#26087,#26088,#26089),
 .UNSPECIFIED.,.F.,.F.,(4,4),(51.5750455984138,52.2860549491936),
 .UNSPECIFIED.);
#2350=B_SPLINE_CURVE_WITH_KNOTS('',3,(#26092,#26093,#26094,#26095,#26096,
#26097,#26098,#26099,#26100,#26101),.UNSPECIFIED.,.F.,.F.,(4,3,3,4),(-50.2654824574367,
-49.3264669332015,-48.3399375945375,-47.8348991546268),.UNSPECIFIED.);
#2351=B_SPLINE_CURVE_WITH_KNOTS('',3,(#26106,#26107,#26108,#26109,#26110,
#26111,#26112,#26113,#26114,#26115,#26116,#26117,#26118,#26119,#26120,#26121,
#26122,#26123,#26124,#26125,#26126,#26127,#26128,#26129,#26130),
 .UNSPECIFIED.,.F.,.F.,(4,3,3,3,3,3,3,3,4),(45.2918602912342,45.3803495785454,
46.3668789172094,47.3534082558735,48.3399375945375,49.3264669332015,50.3129962718656,
51.2995256105296,51.5750455984138),.UNSPECIFIED.);
#2352=B_SPLINE_CURVE_WITH_KNOTS('',3,(#26131,#26132,#26133,#26134,#26135,
#26136,#26137,#26138,#26139,#26140,#26141,#26142,#26143,#26144,#26145,#26146,
#26147,#26148,#26149,#26150,#26151,#26152),.UNSPECIFIED.,.F.,.F.,(4,3,3,
3,3,3,3,4),(-47.8348991546268,-47.3534082558735,-46.3668789172095,-45.3803495785454,
-44.3938202398814,-43.4072909012174,-42.4207615625533,-41.5517138474472),
 .UNSPECIFIED.);
#2353=B_SPLINE_CURVE_WITH_KNOTS('',3,(#26157,#26158,#26159,#26160,#26161,
#26162,#26163,#26164,#26165,#26166,#26167,#26168,#26169,#26170,#26171,#26172,
#26173,#26174,#26175,#26176,#26177,#26178),.UNSPECIFIED.,.F.,.F.,(4,3,3,
3,3,3,3,4),(39.0086749840546,39.4611735465612,40.4477028852253,41.4342322238893,
42.4207615625533,43.4072909012174,44.3938202398814,45.2918602912342),
 .UNSPECIFIED.);
#2354=B_SPLINE_CURVE_WITH_KNOTS('',3,(#26179,#26180,#26181,#26182,#26183,
#26184,#26185,#26186,#26187,#26188,#26189,#26190,#26191,#26192,#26193,#26194,
#26195,#26196,#26197,#26198,#26199,#26200,#26201,#26202,#26203),
 .UNSPECIFIED.,.F.,.F.,(4,3,3,3,3,3,3,3,4),(-41.5517138474472,-41.4342322238893,
-40.4477028852253,-39.4611735465612,-38.4746442078972,-37.4881148692332,
-36.5015855305691,-35.5150561919051,-35.2685285402676),.UNSPECIFIED.);
#2355=B_SPLINE_CURVE_WITH_KNOTS('',3,(#26208,#26209,#26210,#26211,#26212,
#26213,#26214,#26215,#26216,#26217,#26218,#26219,#26220,#26221,#26222,#26223,
#26224,#26225,#26226,#26227,#26228,#26229),.UNSPECIFIED.,.F.,.F.,(4,3,3,
3,3,3,3,4),(32.725489676875,33.541997514577,34.5285268532411,35.5150561919051,
36.5015855305691,37.4881148692332,38.4746442078972,39.0086749840546),
 .UNSPECIFIED.);
#2356=B_SPLINE_CURVE_WITH_KNOTS('',3,(#26230,#26231,#26232,#26233,#26234,
#26235,#26236,#26237,#26238,#26239,#26240,#26241,#26242,#26243,#26244,#26245,
#26246,#26247,#26248,#26249,#26250,#26251),.UNSPECIFIED.,.F.,.F.,(4,3,3,
3,3,3,3,4),(-35.2685285402676,-34.5285268532411,-33.541997514577,-32.555468175913,
-31.568938837249,-30.582409498585,-29.5958801599209,-28.985343233088),
 .UNSPECIFIED.);
#2357=B_SPLINE_CURVE_WITH_KNOTS('',3,(#26256,#26257,#26258,#26259,#26260,
#26261,#26262,#26263,#26264,#26265,#26266,#26267,#26268,#26269,#26270,#26271,
#26272,#26273,#26274,#26275,#26276,#26277,#26278,#26279,#26280),
 .UNSPECIFIED.,.F.,.F.,(4,3,3,3,3,3,3,3,4),(26.4423043696954,26.6362921439288,
27.6228214825929,28.6093508212569,29.5958801599209,30.582409498585,31.568938837249,
32.555468175913,32.725489676875),.UNSPECIFIED.);
#2358=B_SPLINE_CURVE_WITH_KNOTS('',3,(#26281,#26282,#26283,#26284,#26285,
#26286,#26287,#26288,#26289,#26290,#26291,#26292,#26293,#26294,#26295,#26296,
#26297,#26298,#26299,#26300,#26301,#26302),.UNSPECIFIED.,.F.,.F.,(4,3,3,
3,3,3,3,4),(-28.985343233088,-28.6093508212569,-27.6228214825929,-26.6362921439288,
-25.6497628052648,-24.6632334666008,-23.6767041279367,-22.7021579259084),
 .UNSPECIFIED.);
#2359=B_SPLINE_CURVE_WITH_KNOTS('',3,(#26307,#26308,#26309,#26310,#26311,
#26312,#26313,#26314,#26315,#26316,#26317,#26318,#26319,#26320,#26321,#26322,
#26323,#26324,#26325,#26326,#26327,#26328),.UNSPECIFIED.,.F.,.F.,(4,3,3,
3,3,3,3,4),(20.1591190625159,20.7171161119446,21.7036454506087,22.6901747892727,
23.6767041279367,24.6632334666008,25.6497628052648,26.4423043696954),
 .UNSPECIFIED.);
#2360=B_SPLINE_CURVE_WITH_KNOTS('',3,(#26329,#26330,#26331,#26332,#26333,
#26334,#26335,#26336,#26337,#26338,#26339,#26340,#26341,#26342,#26343,#26344,
#26345,#26346,#26347,#26348,#26349,#26350,#26351,#26352,#26353),
 .UNSPECIFIED.,.F.,.F.,(4,3,3,3,3,3,3,3,4),(-22.7021579259084,-22.6901747892727,
-21.7036454506087,-20.7171161119446,-19.7305867732806,-18.7440574346166,
-17.7575280959526,-16.7709987572885,-16.4189726187288),.UNSPECIFIED.);
#2361=B_SPLINE_CURVE_WITH_KNOTS('',3,(#26358,#26359,#26360,#26361,#26362,
#26363,#26364,#26365,#26366,#26367,#26368,#26369,#26370,#26371,#26372,#26373,
#26374,#26375,#26376,#26377,#26378,#26379),.UNSPECIFIED.,.F.,.F.,(4,3,3,
3,3,3,3,4),(13.8759337553363,14.7979400799605,15.7844694186245,16.7709987572885,
17.7575280959526,18.7440574346166,19.7305867732806,20.1591190625159),
 .UNSPECIFIED.);
#2362=B_SPLINE_CURVE_WITH_KNOTS('',3,(#26380,#26381,#26382,#26383,#26384,
#26385,#26386,#26387,#26388,#26389,#26390,#26391,#26392,#26393,#26394,#26395,
#26396,#26397,#26398,#26399,#26400,#26401),.UNSPECIFIED.,.F.,.F.,(4,3,3,
3,3,3,3,4),(-16.4189726187288,-15.7844694186245,-14.7979400799605,-13.8114107412964,
-12.8248814026324,-11.8383520639684,-10.8518227253043,-10.1357873115492),
 .UNSPECIFIED.);
#2363=B_SPLINE_CURVE_WITH_KNOTS('',3,(#26407,#26408,#26409,#26410,#26411,
#26412,#26413,#26414,#26415,#26416,#26417,#26418,#26419),.UNSPECIFIED.,
 .F.,.F.,(4,3,3,3,4),(-3.85260200436966,-2.95958801599209,-1.97305867732806,
-0.986529338664031,0.),.UNSPECIFIED.);
#2364=B_SPLINE_CURVE_WITH_KNOTS('',3,(#26422,#26423,#26424,#26425,#26426,
#26427,#26428,#26429,#26430,#26431,#26432,#26433,#26434,#26435,#26436,#26437,
#26438,#26439,#26440),.UNSPECIFIED.,.F.,.F.,(4,3,3,3,3,3,4),(2.0205724917569,
2.95958801599209,3.94611735465612,4.93264669332016,5.91917603198418,6.90570537064822,
7.5927484481567),.UNSPECIFIED.);
#2365=B_SPLINE_CURVE_WITH_KNOTS('',3,(#26446,#26447,#26448,#26449,#26450,
#26451,#26452,#26453),.UNSPECIFIED.,.F.,.F.,(4,1,1,1,1,4),(59.6902604182061,
60.1952988581168,61.1818281967808,62.1683575354449,63.1548868741089,64.1414162127729),
 .UNSPECIFIED.);
#2366=B_SPLINE_CURVE_WITH_KNOTS('',3,(#26456,#26457,#26458,#26459,#26460,
#26461,#26462,#26463,#26464),.UNSPECIFIED.,.F.,.F.,(4,1,1,1,1,1,4),(59.6902604182061,
59.7787497055172,60.7652790441813,61.7518083828453,62.7383377215093,63.7248670601734,
64.6638825844086),.UNSPECIFIED.);
#2367=B_SPLINE_CURVE_WITH_KNOTS('',3,(#26469,#26470,#26471,#26472,#26473,
#26474,#26475,#26476,#26477,#26478),.UNSPECIFIED.,.F.,.F.,(4,1,1,1,1,1,
1,4),(53.4070751110265,54.2761228261326,55.2626521647967,56.2491815034607,
57.2357108421247,58.2222401807888,59.2087695194528,59.6902604182061),
 .UNSPECIFIED.);
#2368=B_SPLINE_CURVE_WITH_KNOTS('',3,(#26479,#26480,#26481,#26482,#26483,
#26484,#26485,#26486,#26487,#26488),.UNSPECIFIED.,.F.,.F.,(4,1,1,1,1,1,
1,4),(53.4070751110265,53.8595736735331,54.8461030121971,55.8326323508611,
56.8191616895251,57.8056910281892,58.7922203668532,59.6902604182061),
 .UNSPECIFIED.);
#2369=B_SPLINE_CURVE_WITH_KNOTS('',3,(#26493,#26494,#26495,#26496,#26497,
#26498,#26499,#26500,#26501,#26502,#26503),.UNSPECIFIED.,.F.,.F.,(4,1,1,
1,1,1,1,1,4),(47.1238898038469,47.3704174554844,48.3569467941484,49.3434761328125,
50.3300054714765,51.3165348101405,52.3030641488046,53.2895934874686,53.4070751110265),
 .UNSPECIFIED.);
#2370=B_SPLINE_CURVE_WITH_KNOTS('',3,(#26504,#26505,#26506,#26507,#26508,
#26509,#26510,#26511,#26512,#26513),.UNSPECIFIED.,.F.,.F.,(4,1,1,1,1,1,
1,4),(47.1238898038469,47.9403976415489,48.9269269802129,49.9134563188769,
50.899985657541,51.886514996205,52.873044334869,53.4070751110265),
 .UNSPECIFIED.);
#2371=B_SPLINE_CURVE_WITH_KNOTS('',3,(#26518,#26519,#26520,#26521,#26522,
#26523,#26524,#26525,#26526,#26527),.UNSPECIFIED.,.F.,.F.,(4,1,1,1,1,1,
1,4),(40.8407044966673,41.4512414235002,42.4377707621643,43.4243001008283,
44.4108294394923,45.3973587781563,46.3838881168204,47.1238898038469),
 .UNSPECIFIED.);
#2372=B_SPLINE_CURVE_WITH_KNOTS('',3,(#26528,#26529,#26530,#26531,#26532,
#26533,#26534,#26535,#26536,#26537,#26538),.UNSPECIFIED.,.F.,.F.,(4,1,1,
1,1,1,1,1,4),(40.8407044966673,41.0346922709007,42.0212216095647,43.0077509482287,
43.9942802868928,44.9808096255568,45.9673389642208,46.9538683028848,47.1238898038469),
 .UNSPECIFIED.);
#2373=B_SPLINE_CURVE_WITH_KNOTS('',3,(#26543,#26544,#26545,#26546,#26547,
#26548,#26549,#26550,#26551,#26552),.UNSPECIFIED.,.F.,.F.,(4,1,1,1,1,1,
1,4),(34.5575191894877,35.532065391516,36.5185947301801,37.5051240688441,
38.4916534075081,39.4781827461722,40.4647120848362,40.8407044966673),
 .UNSPECIFIED.);
#2374=B_SPLINE_CURVE_WITH_KNOTS('',3,(#26553,#26554,#26555,#26556,#26557,
#26558,#26559,#26560,#26561,#26562),.UNSPECIFIED.,.F.,.F.,(4,1,1,1,1,1,
1,4),(34.5575191894877,35.1155162389165,36.1020455775805,37.0885749162445,
38.0751042549086,39.0616335935726,40.0481629322366,40.8407044966673),
 .UNSPECIFIED.);
#2375=B_SPLINE_CURVE_WITH_KNOTS('',3,(#26567,#26568,#26569,#26570,#26571,
#26572,#26573,#26574,#26575,#26576,#26577),.UNSPECIFIED.,.F.,.F.,(4,1,1,
1,1,1,1,1,4),(28.2743338823081,28.6263600208678,29.6128893595319,30.5994186981959,
31.5859480368599,32.5724773755239,33.559006714188,34.545536052852,34.5575191894877),
 .UNSPECIFIED.);
#2376=B_SPLINE_CURVE_WITH_KNOTS('',3,(#26578,#26579,#26580,#26581,#26582,
#26583,#26584,#26585,#26586,#26587),.UNSPECIFIED.,.F.,.F.,(4,1,1,1,1,1,
1,4),(28.2743338823081,29.1963402069323,30.1828695455963,31.1693988842604,
32.1559282229244,33.1424575615884,34.1289869002524,34.5575191894877),
 .UNSPECIFIED.);
#2377=B_SPLINE_CURVE_WITH_KNOTS('',3,(#26592,#26593,#26594,#26595,#26596,
#26597,#26598,#26599,#26600,#26601),.UNSPECIFIED.,.F.,.F.,(4,1,1,1,1,1,
1,4),(21.9911485751285,22.7071839888836,23.6937133275477,24.6802426662117,
25.6667720048757,26.6533013435398,27.6398306822038,28.2743338823081),
 .UNSPECIFIED.);
#2378=B_SPLINE_CURVE_WITH_KNOTS('',3,(#26602,#26603,#26604,#26605,#26606,
#26607,#26608,#26609,#26610,#26611,#26612),.UNSPECIFIED.,.F.,.F.,(4,1,1,
1,1,1,1,1,4),(21.9911485751285,22.2906348362841,23.2771641749481,24.2636935136121,
25.2502228522762,26.2367521909402,27.2232815296042,28.2098108682683,28.2743338823081),
 .UNSPECIFIED.);
#2379=B_SPLINE_CURVE_WITH_KNOTS('',3,(#26618,#26619,#26620,#26621,#26622),
 .UNSPECIFIED.,.F.,.F.,(4,1,4),(14.3984001269718,15.3849294656359,15.707963267949),
 .UNSPECIFIED.);
#2380=B_SPLINE_CURVE_WITH_KNOTS('',3,(#26625,#26626,#26627,#26628,#26629),
 .UNSPECIFIED.,.F.,.F.,(4,1,4),(13.8759337553362,14.8149492795714,15.7079632679489),
 .UNSPECIFIED.);
#2381=B_SPLINE_CURVE_WITH_KNOTS('',3,(#26635,#26636,#26637,#26638,#26639,
#26640,#26641,#26642),.UNSPECIFIED.,.F.,.F.,(4,1,1,1,1,4),(59.6902604182061,
60.1952988581168,61.1818281967808,62.1683575354449,63.1548868741089,64.1414162127729),
 .UNSPECIFIED.);
#2382=B_SPLINE_CURVE_WITH_KNOTS('',3,(#26645,#26646,#26647,#26648,#26649,
#26650,#26651,#26652,#26653),.UNSPECIFIED.,.F.,.F.,(4,1,1,1,1,1,4),(59.6902604182061,
59.7787497055172,60.7652790441813,61.7518083828453,62.7383377215093,63.7248670601734,
64.6638825844086),.UNSPECIFIED.);
#2383=B_SPLINE_CURVE_WITH_KNOTS('',3,(#26658,#26659,#26660,#26661,#26662,
#26663,#26664,#26665,#26666,#26667),.UNSPECIFIED.,.F.,.F.,(4,1,1,1,1,1,
1,4),(53.4070751110265,54.2761228261326,55.2626521647967,56.2491815034607,
57.2357108421247,58.2222401807888,59.2087695194528,59.6902604182061),
 .UNSPECIFIED.);
#2384=B_SPLINE_CURVE_WITH_KNOTS('',3,(#26668,#26669,#26670,#26671,#26672,
#26673,#26674,#26675,#26676,#26677),.UNSPECIFIED.,.F.,.F.,(4,1,1,1,1,1,
1,4),(53.4070751110265,53.8595736735331,54.8461030121971,55.8326323508611,
56.8191616895251,57.8056910281892,58.7922203668532,59.6902604182061),
 .UNSPECIFIED.);
#2385=B_SPLINE_CURVE_WITH_KNOTS('',3,(#26682,#26683,#26684,#26685,#26686,
#26687,#26688,#26689,#26690,#26691,#26692),.UNSPECIFIED.,.F.,.F.,(4,1,1,
1,1,1,1,1,4),(47.1238898038469,47.3704174554844,48.3569467941484,49.3434761328125,
50.3300054714765,51.3165348101405,52.3030641488046,53.2895934874686,53.4070751110265),
 .UNSPECIFIED.);
#2386=B_SPLINE_CURVE_WITH_KNOTS('',3,(#26693,#26694,#26695,#26696,#26697,
#26698,#26699,#26700,#26701,#26702),.UNSPECIFIED.,.F.,.F.,(4,1,1,1,1,1,
1,4),(47.1238898038469,47.9403976415489,48.9269269802129,49.9134563188769,
50.899985657541,51.886514996205,52.873044334869,53.4070751110265),
 .UNSPECIFIED.);
#2387=B_SPLINE_CURVE_WITH_KNOTS('',3,(#26707,#26708,#26709,#26710,#26711,
#26712,#26713,#26714,#26715,#26716),.UNSPECIFIED.,.F.,.F.,(4,1,1,1,1,1,
1,4),(40.8407044966673,41.4512414235002,42.4377707621643,43.4243001008283,
44.4108294394923,45.3973587781563,46.3838881168204,47.1238898038469),
 .UNSPECIFIED.);
#2388=B_SPLINE_CURVE_WITH_KNOTS('',3,(#26717,#26718,#26719,#26720,#26721,
#26722,#26723,#26724,#26725,#26726,#26727),.UNSPECIFIED.,.F.,.F.,(4,1,1,
1,1,1,1,1,4),(40.8407044966673,41.0346922709007,42.0212216095647,43.0077509482287,
43.9942802868928,44.9808096255568,45.9673389642208,46.9538683028848,47.1238898038469),
 .UNSPECIFIED.);
#2389=B_SPLINE_CURVE_WITH_KNOTS('',3,(#26732,#26733,#26734,#26735,#26736,
#26737,#26738,#26739,#26740,#26741),.UNSPECIFIED.,.F.,.F.,(4,1,1,1,1,1,
1,4),(34.5575191894877,35.532065391516,36.5185947301801,37.5051240688441,
38.4916534075081,39.4781827461722,40.4647120848362,40.8407044966673),
 .UNSPECIFIED.);
#2390=B_SPLINE_CURVE_WITH_KNOTS('',3,(#26742,#26743,#26744,#26745,#26746,
#26747,#26748,#26749,#26750,#26751),.UNSPECIFIED.,.F.,.F.,(4,1,1,1,1,1,
1,4),(34.5575191894877,35.1155162389165,36.1020455775805,37.0885749162445,
38.0751042549086,39.0616335935726,40.0481629322366,40.8407044966673),
 .UNSPECIFIED.);
#2391=B_SPLINE_CURVE_WITH_KNOTS('',3,(#26756,#26757,#26758,#26759,#26760,
#26761,#26762,#26763,#26764,#26765,#26766),.UNSPECIFIED.,.F.,.F.,(4,1,1,
1,1,1,1,1,4),(28.2743338823081,28.6263600208678,29.6128893595319,30.5994186981959,
31.5859480368599,32.5724773755239,33.559006714188,34.545536052852,34.5575191894877),
 .UNSPECIFIED.);
#2392=B_SPLINE_CURVE_WITH_KNOTS('',3,(#26767,#26768,#26769,#26770,#26771,
#26772,#26773,#26774,#26775,#26776),.UNSPECIFIED.,.F.,.F.,(4,1,1,1,1,1,
1,4),(28.2743338823081,29.1963402069323,30.1828695455963,31.1693988842604,
32.1559282229244,33.1424575615884,34.1289869002524,34.5575191894877),
 .UNSPECIFIED.);
#2393=B_SPLINE_CURVE_WITH_KNOTS('',3,(#26781,#26782,#26783,#26784,#26785,
#26786,#26787,#26788,#26789,#26790),.UNSPECIFIED.,.F.,.F.,(4,1,1,1,1,1,
1,4),(21.9911485751285,22.7071839888836,23.6937133275477,24.6802426662117,
25.6667720048757,26.6533013435398,27.6398306822038,28.2743338823081),
 .UNSPECIFIED.);
#2394=B_SPLINE_CURVE_WITH_KNOTS('',3,(#26791,#26792,#26793,#26794,#26795,
#26796,#26797,#26798,#26799,#26800,#26801),.UNSPECIFIED.,.F.,.F.,(4,1,1,
1,1,1,1,1,4),(21.9911485751285,22.2906348362841,23.2771641749481,24.2636935136121,
25.2502228522762,26.2367521909402,27.2232815296042,28.2098108682683,28.2743338823081),
 .UNSPECIFIED.);
#2395=B_SPLINE_CURVE_WITH_KNOTS('',3,(#26807,#26808,#26809,#26810,#26811),
 .UNSPECIFIED.,.F.,.F.,(4,1,4),(14.3984001269718,15.3849294656359,15.707963267949),
 .UNSPECIFIED.);
#2396=B_SPLINE_CURVE_WITH_KNOTS('',3,(#26814,#26815,#26816,#26817,#26818),
 .UNSPECIFIED.,.F.,.F.,(4,1,4),(13.8759337553362,14.8149492795714,15.7079632679489),
 .UNSPECIFIED.);
#2397=B_SPLINE_CURVE_WITH_KNOTS('',3,(#26820,#26821,#26822,#26823,#26824,
#26825,#26826,#26827,#26828,#26829,#26830),.UNSPECIFIED.,.F.,.F.,(4,1,1,
1,1,1,1,1,4),(15.7079632679489,15.8014786182354,16.7880079568995,17.7745372955635,
18.7610666342275,19.7475959728915,20.7341253115556,21.7206546502196,21.9911485751285),
 .UNSPECIFIED.);
#2398=B_SPLINE_CURVE_WITH_KNOTS('',3,(#26831,#26832,#26833,#26834,#26835,
#26836,#26837,#26838,#26839,#26840),.UNSPECIFIED.,.F.,.F.,(4,1,1,1,1,1,
1,4),(15.707963267949,16.3714588042999,17.3579881429639,18.344517481628,
19.331046820292,20.317576158956,21.30410549762,21.9911485751285),
 .UNSPECIFIED.);
#2399=B_SPLINE_CURVE_WITH_KNOTS('',3,(#27065,#27066,#27067,#27068,#27069,
#27070,#27071,#27072,#27073,#27074,#27075,#27076,#27077,#27078,#27079,#27080,
#27081,#27082,#27083,#27084,#27085,#27086,#27087,#27088,#27089,#27090,#27091,
#27092,#27093,#27094,#27095,#27096,#27097,#27098,#27099,#27100,#27101,#27102,
#27103,#27104,#27105,#27106,#27107,#27108,#27109,#27110,#27111,#27112,#27113,
#27114,#27115,#27116),.UNSPECIFIED.,.F.,.F.,(4,3,3,3,3,3,3,3,3,3,3,3,3,
3,3,3,3,4),(0.,0.0320331684328983,0.047982254793735,0.0587463569853809,
0.068374331906695,0.0996455206564278,0.112637667143497,0.122453511831961,
0.146764141737192,0.169126652772842,0.178509832567225,0.203948034872107,
0.222826517887668,0.233934300135679,0.251364503567911,0.26339901807632,
0.280262641786753,0.286347380332264),.UNSPECIFIED.);
#2400=B_SPLINE_CURVE_WITH_KNOTS('',3,(#27117,#27118,#27119,#27120,#27121,
#27122,#27123,#27124,#27125,#27126,#27127,#27128,#27129,#27130,#27131,#27132,
#27133,#27134,#27135,#27136,#27137,#27138,#27139,#27140,#27141,#27142,#27143,
#27144,#27145,#27146,#27147,#27148,#27149,#27150,#27151,#27152,#27153,#27154,
#27155,#27156,#27157,#27158,#27159,#27160,#27161,#27162,#27163,#27164,#27165),
 .UNSPECIFIED.,.F.,.F.,(4,3,3,3,3,3,3,3,3,3,3,3,3,3,3,3,4),(0.,0.0274255978447832,
0.048809316595412,0.0580010326491972,0.0875347374149519,0.101224292480011,
0.111280556216297,0.132431451325231,0.155780476821444,0.165670961223459,
0.193708256295631,0.208717590629974,0.219760914288732,0.239138299607853,
0.257256761910142,0.277820141512149,0.28514280399518),.UNSPECIFIED.);
#2401=B_SPLINE_CURVE_WITH_KNOTS('',3,(#27166,#27167,#27168,#27169,#27170,
#27171,#27172,#27173,#27174,#27175,#27176,#27177,#27178,#27179,#27180,#27181,
#27182,#27183,#27184,#27185,#27186,#27187,#27188,#27189,#27190),
 .UNSPECIFIED.,.F.,.F.,(4,3,3,3,3,3,3,3,4),(-10.1357873115492,-9.8652933866403,
-8.87876404797627,-7.89223470931224,-6.90570537064821,-5.91917603198418,
-4.93264669332015,-3.94611735465612,-3.85260200436966),.UNSPECIFIED.);
#2402=B_SPLINE_CURVE_WITH_KNOTS('',3,(#27415,#27416,#27417,#27418,#27419,
#27420,#27421,#27422,#27423,#27424,#27425,#27426,#27427,#27428,#27429,#27430,
#27431,#27432,#27433,#27434,#27435,#27436,#27437,#27438,#27439,#27440,#27441,
#27442,#27443,#27444,#27445,#27446,#27447,#27448,#27449,#27450,#27451,#27452,
#27453,#27454,#27455,#27456,#27457,#27458,#27459,#27460,#27461,#27462,#27463),
 .UNSPECIFIED.,.F.,.F.,(4,3,3,3,3,3,3,3,3,3,3,3,3,3,3,3,4),(0.,0.0274255913653339,
0.0488093131133246,0.0580010269694127,0.0875347308595416,0.101224269152377,
0.111280553657591,0.132431451325227,0.155780477659062,0.165670961808075,
0.193708256734092,0.208717605217266,0.21976091765614,0.239138308570995,
0.257256762582239,0.277820141512144,0.28514280399514),.UNSPECIFIED.);
#2403=B_SPLINE_CURVE_WITH_KNOTS('',3,(#27464,#27465,#27466,#27467,#27468,
#27469,#27470,#27471,#27472,#27473,#27474,#27475,#27476,#27477,#27478,#27479,
#27480,#27481,#27482,#27483,#27484,#27485,#27486,#27487,#27488),
 .UNSPECIFIED.,.F.,.F.,(4,3,3,3,3,3,3,3,4),(7.5927484481567,7.89223470931224,
8.87876404797628,9.86529338664031,10.8518227253043,11.8383520639684,12.8248814026324,
13.8114107412964,13.8759337553363),.UNSPECIFIED.);
#2404=B_SPLINE_CURVE_WITH_KNOTS('',3,(#27489,#27490,#27491,#27492,#27493,
#27494,#27495,#27496,#27497,#27498,#27499,#27500,#27501,#27502,#27503,#27504,
#27505,#27506,#27507,#27508,#27509,#27510,#27511,#27512,#27513,#27514,#27515,
#27516,#27517,#27518,#27519,#27520,#27521,#27522,#27523,#27524,#27525,#27526,
#27527,#27528,#27529,#27530,#27531,#27532,#27533,#27534,#27535,#27536,#27537,
#27538,#27539,#27540),.UNSPECIFIED.,.F.,.F.,(4,3,3,3,3,3,3,3,3,3,3,3,3,
3,3,3,3,4),(0.,0.0320331645440323,0.0479822944538874,0.0587463983360561,
0.0683743388328265,0.0996455292883743,0.112637688108393,0.122453518454582,
0.146764141737195,0.169126651893336,0.178509831787203,0.20394803428708,
0.222826505940554,0.233934299906464,0.251364515046202,0.263399023832158,
0.280262641786714,0.28634738033223),.UNSPECIFIED.);
#2405=B_SPLINE_CURVE_WITH_KNOTS('',3,(#27554,#27555,#27556,#27557,#27558,
#27559,#27560,#27561,#27562,#27563,#27564,#27565,#27566,#27567,#27568,#27569,
#27570,#27571,#27572,#27573,#27574,#27575,#27576,#27577,#27578,#27579,#27580,
#27581,#27582,#27583,#27584,#27585,#27586,#27587,#27588,#27589,#27590,#27591,
#27592,#27593,#27594,#27595,#27596,#27597,#27598,#27599,#27600,#27601,#27602),
 .UNSPECIFIED.,.F.,.F.,(4,3,3,3,3,3,3,3,3,3,3,3,3,3,3,3,4),(0.,0.0274256070877454,
0.0488093215641943,0.0580010407627361,0.0875347467776894,0.101224325795315,
0.111280559869577,0.132431451325226,0.155780475624762,0.165670960389251,
0.193708255669975,0.208717569845021,0.219760909477782,0.239138286790648,
0.257256760954527,0.277820141512144,0.285142803995137),.UNSPECIFIED.);
#2406=B_SPLINE_CURVE_WITH_KNOTS('',3,(#27603,#27604,#27605,#27606,#27607,
#27608,#27609,#27610,#27611,#27612,#27613,#27614,#27615,#27616,#27617,#27618,
#27619,#27620,#27621,#27622,#27623,#27624,#27625,#27626,#27627,#27628,#27629,
#27630,#27631,#27632,#27633,#27634,#27635,#27636,#27637,#27638,#27639,#27640,
#27641,#27642,#27643,#27644,#27645,#27646,#27647,#27648,#27649,#27650,#27651,
#27652,#27653,#27654),.UNSPECIFIED.,.F.,.F.,(4,3,3,3,3,3,3,3,3,3,3,3,3,
3,3,3,3,4),(0.,0.032033144059138,0.0479825033685422,0.058746616231457,0.068374375333449,
0.0996455747709087,0.112637798572108,0.122453553351573,0.146764141737196,
0.169126647261903,0.17850982771232,0.203948031230928,0.22282644299279,0.233934298697096,
0.251364575521066,0.263399054117863,0.280262641786752,0.286347380332261),
 .UNSPECIFIED.);
#2407=B_SPLINE_CURVE_WITH_KNOTS('',3,(#27656,#27657,#27658,#27659,#27660,
#27661,#27662,#27663,#27664,#27665,#27666),.UNSPECIFIED.,.F.,.F.,(4,1,1,
1,1,1,1,1,4),(15.7079632679489,15.8014786182354,16.7880079568995,17.7745372955635,
18.7610666342275,19.7475959728915,20.7341253115556,21.7206546502196,21.9911485751285),
 .UNSPECIFIED.);
#2408=B_SPLINE_CURVE_WITH_KNOTS('',3,(#27667,#27668,#27669,#27670,#27671,
#27672,#27673,#27674,#27675,#27676),.UNSPECIFIED.,.F.,.F.,(4,1,1,1,1,1,
1,4),(15.707963267949,16.3714588042999,17.3579881429639,18.344517481628,
19.331046820292,20.317576158956,21.30410549762,21.9911485751285),
 .UNSPECIFIED.);
#2409=B_SPLINE_CURVE_WITH_KNOTS('',3,(#27901,#27902,#27903,#27904,#27905,
#27906,#27907,#27908,#27909,#27910,#27911,#27912,#27913,#27914,#27915,#27916,
#27917,#27918,#27919,#27920,#27921,#27922,#27923,#27924,#27925,#27926,#27927,
#27928,#27929,#27930,#27931,#27932,#27933,#27934,#27935,#27936,#27937,#27938,
#27939,#27940,#27941,#27942,#27943,#27944,#27945,#27946,#27947,#27948,#27949),
 .UNSPECIFIED.,.F.,.F.,(4,3,3,3,3,3,3,3,3,3,3,3,3,3,3,3,4),(0.,0.0274255572386018,
0.0488092947703195,0.0580009970300377,0.0875346963040298,0.101224146180659,
0.111280540172636,0.132431451325231,0.155780482071967,0.165670964883965,
0.19370825904101,0.208717681926172,0.219760935414438,0.239138355867989,
0.257256766122231,0.277820141512143,0.285142803995174),.UNSPECIFIED.);
#2410=B_SPLINE_CURVE_WITH_KNOTS('',3,(#27950,#27951,#27952,#27953,#27954,
#27955,#27956,#27957,#27958,#27959,#27960,#27961,#27962,#27963,#27964,#27965,
#27966,#27967,#27968,#27969,#27970,#27971,#27972,#27973,#27974),
 .UNSPECIFIED.,.F.,.F.,(4,3,3,3,3,3,3,3,4),(-10.1357873115492,-9.8652933866403,
-8.87876404797628,-7.89223470931224,-6.90570537064821,-5.91917603198418,
-4.93264669332015,-3.94611735465612,-3.85260200436966),.UNSPECIFIED.);
#2411=B_SPLINE_CURVE_WITH_KNOTS('',3,(#28199,#28200,#28201,#28202,#28203,
#28204,#28205,#28206,#28207,#28208,#28209,#28210,#28211,#28212,#28213,#28214,
#28215,#28216,#28217,#28218,#28219,#28220,#28221,#28222,#28223),
 .UNSPECIFIED.,.F.,.F.,(4,3,3,3,3,3,3,3,4),(7.5927484481567,7.89223470931225,
8.87876404797628,9.86529338664031,10.8518227253043,11.8383520639684,12.8248814026324,
13.8114107412964,13.8759337553363),.UNSPECIFIED.);
#2412=B_SPLINE_CURVE_WITH_KNOTS('',3,(#28224,#28225,#28226,#28227,#28228,
#28229,#28230,#28231,#28232,#28233,#28234,#28235,#28236,#28237,#28238,#28239,
#28240,#28241,#28242,#28243,#28244,#28245,#28246,#28247,#28248,#28249,#28250,
#28251,#28252,#28253,#28254,#28255,#28256,#28257,#28258,#28259,#28260,#28261,
#28262,#28263,#28264,#28265,#28266,#28267,#28268,#28269,#28270,#28271,#28272,
#28273,#28274,#28275),.UNSPECIFIED.,.F.,.F.,(4,3,3,3,3,3,3,3,3,3,3,3,3,
3,3,3,3,4),(0.,0.0320331739806594,0.047982198208099,0.0587462979950865,
0.0683743220264688,0.0996455083427913,0.112637637236076,0.122453502382791,
0.146764141737189,0.169126654027335,0.178509833663637,0.203948035694404,
0.222826534951851,0.233934300464251,0.251364487179106,0.263399009878289,
0.280262641786705,0.286347380332219),.UNSPECIFIED.);
#2413=B_SPLINE_CURVE_WITH_KNOTS('',3,(#28279,#28280,#28281,#28282,#28283,
#28284,#28285,#28286,#28287,#28288,#28289,#28290,#28291,#28292,#28293,#28294,
#28295,#28296,#28297,#28298,#28299,#28300,#28301,#28302,#28303,#28304,#28305,
#28306,#28307,#28308,#28309,#28310,#28311,#28312,#28313,#28314,#28315,#28316,
#28317,#28318,#28319,#28320,#28321,#28322,#28323,#28324,#28325,#28326,#28327,
#28328,#28329,#28330,#28331,#28332,#28333),.UNSPECIFIED.,.F.,.F.,(4,3,3,
3,3,3,3,3,3,3,3,3,3,3,3,3,3,3,4),(-0.378621596831506,-0.353562246876325,
-0.339726745125034,-0.324795320074381,-0.299965799454646,-0.289116647258409,
-0.252367455997566,-0.234471207960412,-0.219335677585236,-0.200829495678116,
-0.174828907630048,-0.155853084460074,-0.144932199137797,-0.109703302304573,
-0.0896821993996096,-0.0773430052299345,-0.0372184478821882,-0.00401661180490171,
0.),.UNSPECIFIED.);
#2414=B_SPLINE_CURVE_WITH_KNOTS('',3,(#28334,#28335,#28336,#28337,#28338,
#28339,#28340,#28341,#28342,#28343,#28344,#28345,#28346,#28347,#28348,#28349,
#28350,#28351,#28352,#28353,#28354,#28355,#28356,#28357,#28358,#28359,#28360,
#28361,#28362,#28363,#28364,#28365,#28366,#28367,#28368,#28369,#28370,#28371,
#28372,#28373,#28374,#28375,#28376,#28377,#28378,#28379,#28380,#28381,#28382,
#28383,#28384,#28385,#28386,#28387,#28388),.UNSPECIFIED.,.F.,.F.,(4,3,3,
3,3,3,3,3,3,3,3,3,3,3,3,3,3,3,4),(-0.376940817211645,-0.351602392887994,
-0.33251855101009,-0.318227201330527,-0.288328241243131,-0.272716591979397,
-0.234504390923632,-0.216959715082621,-0.205491684554535,-0.180854828870955,
-0.153735831424588,-0.136659504603933,-0.126241092823357,-0.0954984218751326,
-0.0666697806071311,-0.0558640204611096,-0.021970383107796,-0.00327040903045916,
0.),.UNSPECIFIED.);
#2415=B_SPLINE_CURVE_WITH_KNOTS('',3,(#28390,#28391,#28392,#28393,#28394,
#28395,#28396,#28397,#28398,#28399,#28400),.UNSPECIFIED.,.F.,.F.,(4,1,1,
1,1,1,1,1,4),(15.7079632679489,15.8518654961883,16.8494368691713,17.8470082421542,
18.8445796151371,19.8421509881201,20.839722361103,21.837293734086,21.9911485751285),
 .UNSPECIFIED.);
#2416=B_SPLINE_CURVE_WITH_KNOTS('',3,(#28401,#28402,#28403,#28404,#28405,
#28406,#28407,#28408,#28409,#28410),.UNSPECIFIED.,.F.,.F.,(4,1,1,1,1,1,
1,4),(15.7079632679489,16.3932837587427,17.3908551317256,18.3884265047086,
19.3859978776915,20.3835692506744,21.3811406236574,21.9911485751285),
 .UNSPECIFIED.);
#2417=B_SPLINE_CURVE_WITH_KNOTS('',3,(#28755,#28756,#28757,#28758,#28759,
#28760,#28761,#28762,#28763,#28764,#28765,#28766,#28767,#28768,#28769,#28770,
#28771,#28772,#28773,#28774,#28775,#28776,#28777,#28778,#28779,#28780,#28781,
#28782,#28783,#28784,#28785,#28786,#28787,#28788,#28789,#28790,#28791,#28792,
#28793,#28794,#28795,#28796,#28797,#28798,#28799,#28800,#28801,#28802,#28803,
#28804,#28805,#28806),.UNSPECIFIED.,.F.,.F.,(4,3,3,3,3,3,3,3,3,3,3,3,3,
3,3,3,3,4),(0.,0.0336928872610179,0.0587353899469406,0.0734853414895339,
0.10979289593323,0.132866050933898,0.143634155874187,0.177205256270033,
0.19591174232575,0.207613838096411,0.244893860705133,0.269595977941347,
0.282504950871715,0.310154017664246,0.327714110380406,0.342573451622329,
0.372940760482264,0.376940817211574),.UNSPECIFIED.);
#2418=B_SPLINE_CURVE_WITH_KNOTS('',3,(#28807,#28808,#28809,#28810,#28811,
#28812,#28813,#28814,#28815,#28816,#28817,#28818,#28819,#28820,#28821,#28822,
#28823,#28824,#28825,#28826,#28827,#28828,#28829,#28830,#28831),
 .UNSPECIFIED.,.F.,.F.,(4,3,3,3,3,3,3,3,4),(-10.1295685708719,-9.97571372982934,
-8.9781423568464,-7.98057098386347,-6.98299961088054,-5.9854282378976,-4.98785686491467,
-3.99028549193173,-3.84638326369226),.UNSPECIFIED.);
#2419=B_SPLINE_CURVE_WITH_KNOTS('',3,(#29176,#29177,#29178,#29179,#29180,
#29181,#29182,#29183,#29184,#29185,#29186,#29187,#29188,#29189,#29190,#29191,
#29192,#29193,#29194,#29195,#29196,#29197),.UNSPECIFIED.,.F.,.F.,(4,3,3,
3,3,3,3,4),(7.59300756235165,7.98057098386347,8.9781423568464,9.97571372982934,
10.9732851028123,11.9708564757952,12.9684278487781,13.8761928695313),
 .UNSPECIFIED.);
#2420=B_SPLINE_CURVE_WITH_KNOTS('',3,(#29198,#29199,#29200,#29201,#29202,
#29203,#29204,#29205,#29206,#29207,#29208,#29209,#29210,#29211,#29212,#29213,
#29214,#29215,#29216,#29217,#29218,#29219,#29220,#29221,#29222,#29223,#29224,
#29225,#29226,#29227,#29228,#29229,#29230,#29231,#29232,#29233,#29234,#29235,
#29236,#29237,#29238,#29239,#29240,#29241,#29242,#29243,#29244,#29245,#29246,
#29247,#29248,#29249),.UNSPECIFIED.,.F.,.F.,(4,3,3,3,3,3,3,3,3,3,3,3,3,
3,3,3,3,4),(0.,0.0396802077059044,0.0598020944317896,0.0772905411980831,
0.0898519540170797,0.128513068109953,0.153545960121946,0.165105837651985,
0.197163594226428,0.224451618228952,0.234159833899698,0.269454677349509,
0.287586460843776,0.305420009888492,0.333077118982087,0.347224172298259,
0.375339207698941,0.37862159683149),.UNSPECIFIED.);
#2421=B_SPLINE_CURVE_WITH_KNOTS('',3,(#29811,#29812,#29813,#29814,#29815,
#29816,#29817,#29818,#29819,#29820,#29821,#29822,#29823,#29824,#29825,#29826,
#29827,#29828,#29829,#29830,#29831,#29832,#29833,#29834,#29835,#29836,#29837,
#29838,#29839,#29840,#29841,#29842,#29843,#29844,#29845,#29846,#29847,#29848,
#29849,#29850,#29851),.UNSPECIFIED.,.F.,.F.,(4,1,1,1,1,1,1,1,1,1,1,1,1,
1,1,1,1,1,1,1,1,1,1,1,1,1,1,1,1,1,1,1,1,1,1,1,1,1,4),(0.,0.496040945303652,
0.992081890607303,1.48812283591095,1.98416378121461,2.48020472651826,2.97624567182191,
3.47228661712556,3.96832756242921,4.46436850773286,4.96040945303652,5.45645039834017,
5.95249134364382,6.44853228894747,6.94457323425112,7.44061417955477,7.93665512485842,
8.43269607016208,8.92873701546573,9.42477796076938,9.92081890607303,10.4168598513767,
10.9129007966803,11.408941741984,11.9049826872876,12.4010236325913,12.8970645778949,
13.3931055231986,13.8891464685022,14.3851874138059,14.8812283591095,15.3772693044132,
15.8733102497168,16.3693511950205,16.8653921403242,17.3614330856278,17.8574740309315,
18.3535149762351,18.8495559215388),.UNSPECIFIED.);
#2422=B_SPLINE_CURVE_WITH_KNOTS('',3,(#29861,#29862,#29863,#29864,#29865,
#29866,#29867,#29868,#29869,#29870,#29871,#29872,#29873,#29874,#29875,#29876,
#29877,#29878,#29879,#29880,#29881,#29882),.UNSPECIFIED.,.F.,.F.,(4,3,3,
3,3,3,3,4),(76.7080459413271,76.8129957196858,77.8105670926688,78.8081384656517,
79.8057098386346,80.8032812116176,81.8008525846005,82.7984239575834),
 .UNSPECIFIED.);
#2423=B_SPLINE_CURVE_WITH_KNOTS('',3,(#29886,#29887,#29888,#29889,#29890,
#29891,#29892),.UNSPECIFIED.,.F.,.F.,(4,3,4),(-80.783811092309,-79.8057098386346,
-79.2446069498474),.UNSPECIFIED.);
#2424=B_SPLINE_CURVE_WITH_KNOTS('',3,(#29896,#29897,#29898,#29899,#29900,
#29901,#29902,#29903,#29904,#29905,#29906,#29907,#29908,#29909,#29910,#29911,
#29912,#29913,#29914,#29915,#29916,#29917),.UNSPECIFIED.,.F.,.F.,(4,3,3,
3,3,3,3,4),(-79.2446069498474,-78.8081384656517,-77.8105670926688,-76.8129957196858,
-75.8154243467029,-74.81785297372,-73.820281600737,-72.9614216426678),
 .UNSPECIFIED.);
#2425=B_SPLINE_CURVE_WITH_KNOTS('',3,(#29922,#29923,#29924,#29925,#29926,
#29927,#29928,#29929,#29930,#29931,#29932,#29933,#29934,#29935,#29936,#29937,
#29938,#29939,#29940,#29941,#29942,#29943),.UNSPECIFIED.,.F.,.F.,(4,3,3,
3,3,3,3,4),(70.4248606341475,70.8275674817882,71.8251388547712,72.8227102277541,
73.820281600737,74.81785297372,75.8154243467029,76.7080459413271),
 .UNSPECIFIED.);
#2426=B_SPLINE_CURVE_WITH_KNOTS('',3,(#29944,#29945,#29946,#29947,#29948,
#29949,#29950,#29951,#29952,#29953,#29954,#29955,#29956,#29957,#29958,#29959,
#29960,#29961,#29962,#29963,#29964,#29965,#29966,#29967,#29968),
 .UNSPECIFIED.,.F.,.F.,(4,3,3,3,3,3,3,3,4),(-72.9614216426678,-72.8227102277541,
-71.8251388547712,-70.8275674817882,-69.8299961088053,-68.8324247358224,
-67.8348533628394,-66.8372819898565,-66.6782363354882),.UNSPECIFIED.);
#2427=B_SPLINE_CURVE_WITH_KNOTS('',3,(#29973,#29974,#29975,#29976,#29977,
#29978,#29979,#29980,#29981,#29982,#29983,#29984,#29985,#29986,#29987,#29988,
#29989,#29990,#29991,#29992,#29993,#29994),.UNSPECIFIED.,.F.,.F.,(4,3,3,
3,3,3,3,4),(64.1416753269679,64.8421392438906,65.8397106168736,66.8372819898565,
67.8348533628394,68.8324247358224,69.8299961088053,70.4248606341475),
 .UNSPECIFIED.);
#2428=B_SPLINE_CURVE_WITH_KNOTS('',3,(#29995,#29996,#29997,#29998,#29999,
#30000,#30001,#30002,#30003,#30004,#30005,#30006,#30007,#30008,#30009,#30010,
#30011,#30012,#30013,#30014,#30015,#30016),.UNSPECIFIED.,.F.,.F.,(4,3,3,
3,3,3,3,4),(-66.6782363354882,-65.8397106168736,-64.8421392438907,-63.8445678709077,
-62.8469964979248,-61.8494251249419,-60.8518537519589,-60.3950510283086),
 .UNSPECIFIED.);
#2429=B_SPLINE_CURVE_WITH_KNOTS('',3,(#30021,#30022,#30023,#30024,#30025,
#30026,#30027,#30028,#30029,#30030,#30031,#30032,#30033,#30034,#30035,#30036,
#30037,#30038,#30039,#30040,#30041,#30042),.UNSPECIFIED.,.F.,.F.,(4,3,3,
3,3,3,3,4),(57.8584900197883,58.856711005993,59.854282378976,60.8518537519589,
61.8494251249418,62.8469964979247,63.8445678709077,64.1416753269679),
 .UNSPECIFIED.);
#2430=B_SPLINE_CURVE_WITH_KNOTS('',3,(#30043,#30044,#30045,#30046,#30047,
#30048,#30049,#30050,#30051,#30052,#30053,#30054,#30055,#30056,#30057,#30058,
#30059,#30060,#30061,#30062,#30063,#30064),.UNSPECIFIED.,.F.,.F.,(4,3,3,
3,3,3,3,4),(-60.3950510283086,-59.854282378976,-58.856711005993,-57.8591396330101,
-56.8615682600272,-55.8639968870442,-54.8664255140613,-54.111865721129),
 .UNSPECIFIED.);
#2431=B_SPLINE_CURVE_WITH_KNOTS('',3,(#30069,#30070,#30071,#30072,#30073,
#30074,#30075,#30076,#30077,#30078,#30079,#30080,#30081,#30082,#30083,#30084,
#30085,#30086,#30087,#30088,#30089,#30090),.UNSPECIFIED.,.F.,.F.,(4,3,3,
3,3,3,3,4),(51.5753047126087,51.8737113951125,52.8712827680954,53.8688541410784,
54.8664255140613,55.8639968870442,56.8615682600272,57.8584900197883),
 .UNSPECIFIED.);
#2432=B_SPLINE_CURVE_WITH_KNOTS('',3,(#30091,#30092,#30093,#30094,#30095,
#30096,#30097,#30098,#30099,#30100,#30101,#30102,#30103,#30104,#30105,#30106,
#30107,#30108,#30109,#30110,#30111,#30112,#30113,#30114,#30115),
 .UNSPECIFIED.,.F.,.F.,(4,3,3,3,3,3,3,3,4),(-54.111865721129,-53.8688541410784,
-52.8712827680954,-51.8737113951125,-50.8761400221296,-49.8785686491466,
-48.8809972761637,-47.8834259031808,-47.8286804139494),.UNSPECIFIED.);
#2433=B_SPLINE_CURVE_WITH_KNOTS('',3,(#30120,#30121,#30122,#30123,#30124,
#30125,#30126,#30127,#30128,#30129,#30130,#30131,#30132,#30133,#30134,#30135,
#30136,#30137,#30138,#30139,#30140,#30141),.UNSPECIFIED.,.F.,.F.,(4,3,3,
3,3,3,3,4),(45.2921194054291,45.8882831572149,46.8858545301978,47.8834259031808,
48.8809972761637,49.8785686491466,50.8761400221296,51.5753047126087),
 .UNSPECIFIED.);
#2434=B_SPLINE_CURVE_WITH_KNOTS('',3,(#30142,#30143,#30144,#30145,#30146,
#30147,#30148,#30149,#30150,#30151,#30152,#30153,#30154,#30155,#30156,#30157,
#30158,#30159,#30160,#30161,#30162,#30163),.UNSPECIFIED.,.F.,.F.,(4,3,3,
3,3,3,3,4),(-47.8286804139494,-46.8858545301979,-45.8882831572149,-44.890711784232,
-43.893140411249,-42.8955690382661,-41.8979976652832,-41.5454951067698),
 .UNSPECIFIED.);
#2435=B_SPLINE_CURVE_WITH_KNOTS('',3,(#30168,#30169,#30170,#30171,#30172,
#30173,#30174,#30175,#30176,#30177,#30178,#30179,#30180,#30181,#30182,#30183,
#30184,#30185,#30186,#30187,#30188,#30189),.UNSPECIFIED.,.F.,.F.,(4,3,3,
3,3,3,3,4),(39.0089340982495,39.9028549193173,40.9004262923002,41.8979976652832,
42.8955690382661,43.893140411249,44.890711784232,45.2921194054291),
 .UNSPECIFIED.);
#2436=B_SPLINE_CURVE_WITH_KNOTS('',3,(#30190,#30191,#30192,#30193,#30194,
#30195,#30196,#30197,#30198,#30199,#30200,#30201,#30202,#30203,#30204,#30205,
#30206,#30207,#30208,#30209,#30210,#30211),.UNSPECIFIED.,.F.,.F.,(4,3,3,
3,3,3,3,4),(-41.5454951067698,-40.9004262923003,-39.9028549193173,-38.9052835463344,
-37.9077121733515,-36.9101408003685,-35.9125694273856,-35.2623097995902),
 .UNSPECIFIED.);
#2437=B_SPLINE_CURVE_WITH_KNOTS('',3,(#30216,#30217,#30218,#30219,#30220,
#30221,#30222,#30223,#30224,#30225,#30226,#30227,#30228,#30229,#30230,#30231,
#30232,#30233,#30234,#30235,#30236,#30237,#30238,#30239,#30240),
 .UNSPECIFIED.,.F.,.F.,(4,3,3,3,3,3,3,3,4),(32.7257487910699,32.9198553084368,
33.9174266814197,34.9149980544027,35.9125694273856,36.9101408003685,37.9077121733514,
38.9052835463344,39.0089340982495),.UNSPECIFIED.);
#2438=B_SPLINE_CURVE_WITH_KNOTS('',3,(#30241,#30242,#30243,#30244,#30245,
#30246,#30247,#30248,#30249,#30250,#30251,#30252,#30253,#30254,#30255,#30256,
#30257,#30258,#30259,#30260,#30261,#30262),.UNSPECIFIED.,.F.,.F.,(4,3,3,
3,3,3,3,4),(-35.2623097995902,-34.9149980544027,-33.9174266814197,-32.9198553084368,
-31.9222839354538,-30.9247125624709,-29.927141189488,-28.9791244924106),
 .UNSPECIFIED.);
#2439=B_SPLINE_CURVE_WITH_KNOTS('',3,(#30267,#30268,#30269,#30270,#30271,
#30272,#30273,#30274,#30275,#30276,#30277,#30278,#30279,#30280,#30281,#30282,
#30283,#30284,#30285,#30286,#30287,#30288),.UNSPECIFIED.,.F.,.F.,(4,3,3,
3,3,3,3,4),(26.4425634838903,26.9344270705392,27.9319984435221,28.929569816505,
29.927141189488,30.9247125624709,31.9222839354538,32.7257487910699),
 .UNSPECIFIED.);
#2440=B_SPLINE_CURVE_WITH_KNOTS('',3,(#30289,#30290,#30291,#30292,#30293,
#30294,#30295,#30296,#30297,#30298,#30299,#30300,#30301,#30302,#30303,#30304,
#30305,#30306,#30307,#30308,#30309,#30310,#30311,#30312,#30313),
 .UNSPECIFIED.,.F.,.F.,(4,3,3,3,3,3,3,3,4),(-28.9791244924106,-28.929569816505,
-27.9319984435221,-26.9344270705392,-25.9368556975562,-24.9392843245733,
-23.9417129515904,-22.9441415786075,-22.695939185231),.UNSPECIFIED.);
#2441=B_SPLINE_CURVE_WITH_KNOTS('',3,(#30318,#30319,#30320,#30321,#30322,
#30323,#30324,#30325,#30326,#30327,#30328,#30329,#30330,#30331,#30332,#30333,
#30334,#30335,#30336,#30337,#30338,#30339),.UNSPECIFIED.,.F.,.F.,(4,3,3,
3,3,3,3,4),(20.1593781767107,20.9489988326416,21.9465702056245,22.9441415786074,
23.9417129515904,24.9392843245733,25.9368556975562,26.4425634838903),
 .UNSPECIFIED.);
#2442=B_SPLINE_CURVE_WITH_KNOTS('',3,(#30340,#30341,#30342,#30343,#30344,
#30345,#30346,#30347,#30348,#30349,#30350,#30351,#30352,#30353,#30354,#30355,
#30356,#30357,#30358,#30359,#30360,#30361),.UNSPECIFIED.,.F.,.F.,(4,3,3,
3,3,3,3,4),(-22.695939185231,-21.9465702056245,-20.9489988326416,-19.9514274596586,
-18.9538560866757,-17.9562847136928,-16.9587133407099,-16.4127538780514),
 .UNSPECIFIED.);
#2443=B_SPLINE_CURVE_WITH_KNOTS('',3,(#30366,#30367,#30368,#30369,#30370,
#30371,#30372,#30373,#30374,#30375,#30376,#30377,#30378,#30379,#30380,#30381,
#30382,#30383,#30384,#30385,#30386,#30387,#30388,#30389,#30390),
 .UNSPECIFIED.,.F.,.F.,(4,3,3,3,3,3,3,3,4),(13.8761928695311,13.9659992217611,
14.963570594744,15.9611419677269,16.9587133407099,17.9562847136928,18.9538560866757,
19.9514274596586,20.1593781767107),.UNSPECIFIED.);
#2444=B_SPLINE_CURVE_WITH_KNOTS('',3,(#30391,#30392,#30393,#30394,#30395,
#30396,#30397,#30398,#30399,#30400,#30401,#30402,#30403,#30404,#30405,#30406,
#30407,#30408,#30409,#30410,#30411,#30412),.UNSPECIFIED.,.F.,.F.,(4,3,3,
3,3,3,3,4),(-16.4127538780514,-15.9611419677269,-14.963570594744,-13.9659992217611,
-12.9684278487781,-11.9708564757952,-10.9732851028123,-10.1295685708718),
 .UNSPECIFIED.);
#2445=B_SPLINE_CURVE_WITH_KNOTS('',3,(#30418,#30419,#30420,#30421,#30422,
#30423,#30424,#30425,#30426,#30427,#30428,#30429,#30430),.UNSPECIFIED.,
 .F.,.F.,(4,3,3,3,4),(-3.84638326369226,-2.9927141189488,-1.99514274596587,
-0.997571372982931,0.),.UNSPECIFIED.);
#2446=B_SPLINE_CURVE_WITH_KNOTS('',3,(#30433,#30434,#30435,#30436,#30437,
#30438,#30439,#30440,#30441,#30442,#30443,#30444,#30445,#30446,#30447,#30448,
#30449,#30450,#30451),.UNSPECIFIED.,.F.,.F.,(4,3,3,3,3,3,4),(2.01461286527445,
2.9927141189488,3.99028549193173,4.98785686491467,5.9854282378976,6.98299961088053,
7.59300756235155),.UNSPECIFIED.);
#2447=B_SPLINE_CURVE_WITH_KNOTS('',3,(#30457,#30458,#30459,#30460,#30461,
#30462,#30463),.UNSPECIFIED.,.F.,.F.,(4,1,1,1,4),(91.106186954104,91.6672898428913,
92.6648612158742,93.6624325888571,94.6600039618401),.UNSPECIFIED.);
#2448=B_SPLINE_CURVE_WITH_KNOTS('',3,(#30466,#30467,#30468,#30469,#30470,
#30471,#30472,#30473),.UNSPECIFIED.,.F.,.F.,(4,1,1,1,1,4),(91.106186954104,
91.2111367324627,92.2087081054457,93.2062794784286,94.2038508514115,95.1819521050859),
 .UNSPECIFIED.);
#2449=B_SPLINE_CURVE_WITH_KNOTS('',3,(#30478,#30479,#30480,#30481,#30482,
#30483,#30484,#30485,#30486,#30487),.UNSPECIFIED.,.F.,.F.,(4,1,1,1,1,1,
1,4),(84.8230016469244,85.6818616049937,86.6794329779766,87.6770043509595,
88.6745757239425,89.6721470969254,90.6697184699083,91.106186954104),
 .UNSPECIFIED.);
#2450=B_SPLINE_CURVE_WITH_KNOTS('',3,(#30488,#30489,#30490,#30491,#30492,
#30493,#30494,#30495,#30496,#30497),.UNSPECIFIED.,.F.,.F.,(4,1,1,1,1,1,
1,4),(84.8230016469244,85.2257084945651,86.2232798675481,87.220851240531,
88.2184226135139,89.2159939864969,90.2135653594798,91.106186954104),
 .UNSPECIFIED.);
#2451=B_SPLINE_CURVE_WITH_KNOTS('',3,(#30502,#30503,#30504,#30505,#30506,
#30507,#30508,#30509,#30510,#30511,#30512),.UNSPECIFIED.,.F.,.F.,(4,1,1,
1,1,1,1,1,4),(78.5398163397448,78.6988619941132,79.6964333670961,80.694004740079,
81.691576113062,82.6891474860449,83.6867188590278,84.6842902320108,84.8230016469244),
 .UNSPECIFIED.);
#2452=B_SPLINE_CURVE_WITH_KNOTS('',3,(#30513,#30514,#30515,#30516,#30517,
#30518,#30519,#30520,#30521,#30522),.UNSPECIFIED.,.F.,.F.,(4,1,1,1,1,1,
1,4),(78.5398163397448,79.2402802566675,80.2378516296505,81.2354230026334,
82.2329943756163,83.2305657485993,84.2281371215822,84.8230016469244),
 .UNSPECIFIED.);
#2453=B_SPLINE_CURVE_WITH_KNOTS('',3,(#30527,#30528,#30529,#30530,#30531,
#30532,#30533,#30534,#30535,#30536),.UNSPECIFIED.,.F.,.F.,(4,1,1,1,1,1,
1,4),(72.2566310325652,72.7134337562156,73.7110051291985,74.7085765021814,
75.7061478751643,76.7037192481473,77.7012906211302,78.5398163397448),
 .UNSPECIFIED.);
#2454=B_SPLINE_CURVE_WITH_KNOTS('',3,(#30537,#30538,#30539,#30540,#30541,
#30542,#30543,#30544,#30545,#30546,#30547),.UNSPECIFIED.,.F.,.F.,(4,1,1,
1,1,1,1,1,4),(72.2566310325652,72.257280645787,73.2548520187699,74.2524233917529,
75.2499947647358,76.2475661377187,77.2451375107017,78.2427088836846,78.5398163397448),
 .UNSPECIFIED.);
#2455=B_SPLINE_CURVE_WITH_KNOTS('',3,(#30552,#30553,#30554,#30555,#30556,
#30557,#30558,#30559,#30560,#30561),.UNSPECIFIED.,.F.,.F.,(4,1,1,1,1,1,
1,4),(65.9734457253856,66.728005518318,67.7255768913009,68.7231482642838,
69.7207196372668,70.7182910102497,71.7158623832326,72.2566310325652),
 .UNSPECIFIED.);
#2456=B_SPLINE_CURVE_WITH_KNOTS('',3,(#30562,#30563,#30564,#30565,#30566,
#30567,#30568,#30569,#30570,#30571),.UNSPECIFIED.,.F.,.F.,(4,1,1,1,1,1,
1,4),(65.9734457253856,66.2718524078894,67.2694237808723,68.2669951538553,
69.2645665268382,70.2621378998211,71.2597092728041,72.2566310325652),
 .UNSPECIFIED.);
#2457=B_SPLINE_CURVE_WITH_KNOTS('',3,(#30576,#30577,#30578,#30579,#30580,
#30581,#30582,#30583,#30584,#30585,#30586),.UNSPECIFIED.,.F.,.F.,(4,1,1,
1,1,1,1,1,4),(59.690260418206,59.7450059074374,60.7425772804204,61.7401486534033,
62.7377200263862,63.7352913993692,64.7328627723521,65.730434145335,65.9734457253856),
 .UNSPECIFIED.);
#2458=B_SPLINE_CURVE_WITH_KNOTS('',3,(#30587,#30588,#30589,#30590,#30591,
#30592,#30593,#30594,#30595,#30596),.UNSPECIFIED.,.F.,.F.,(4,1,1,1,1,1,
1,4),(59.690260418206,60.2864241699918,61.2839955429747,62.2815669159577,
63.2791382889406,64.2767096619235,65.2742810349065,65.9734457253856),
 .UNSPECIFIED.);
#2459=B_SPLINE_CURVE_WITH_KNOTS('',3,(#30601,#30602,#30603,#30604,#30605,
#30606,#30607,#30608,#30609,#30610),.UNSPECIFIED.,.F.,.F.,(4,1,1,1,1,1,
1,4),(53.4070751110264,53.7595776695398,54.7571490425228,55.7547204155057,
56.7522917884886,57.7498631614716,58.7474345344545,59.690260418206),
 .UNSPECIFIED.);
#2460=B_SPLINE_CURVE_WITH_KNOTS('',3,(#30611,#30612,#30613,#30614,#30615,
#30616,#30617,#30618,#30619,#30620),.UNSPECIFIED.,.F.,.F.,(4,1,1,1,1,1,
1,4),(53.4070751110264,54.3009959320942,55.2985673050771,56.2961386780601,
57.293710051043,58.2912814240259,59.2888527970089,59.690260418206),
 .UNSPECIFIED.);
#2461=B_SPLINE_CURVE_WITH_KNOTS('',3,(#30625,#30626,#30627,#30628,#30629,
#30630,#30631,#30632,#30633,#30634),.UNSPECIFIED.,.F.,.F.,(4,1,1,1,1,1,
1,4),(47.1238898038468,47.7741494316422,48.7717208046252,49.7692921776081,
50.766863550591,51.764434923574,52.7620062965569,53.4070751110264),
 .UNSPECIFIED.);
#2462=B_SPLINE_CURVE_WITH_KNOTS('',3,(#30635,#30636,#30637,#30638,#30639,
#30640,#30641,#30642,#30643,#30644,#30645),.UNSPECIFIED.,.F.,.F.,(4,1,1,
1,1,1,1,1,4),(47.1238898038468,47.3179963212137,48.3155676941966,49.3131390671795,
50.3107104401625,51.3082818131454,52.3058531861283,53.3034245591113,53.4070751110264),
 .UNSPECIFIED.);
#2463=B_SPLINE_CURVE_WITH_KNOTS('',3,(#30650,#30651,#30652,#30653,#30654,
#30655,#30656,#30657,#30658,#30659),.UNSPECIFIED.,.F.,.F.,(4,1,1,1,1,1,
1,4),(40.8407044966673,41.7887211937446,42.7862925667276,43.7838639397105,
44.7814353126934,45.7790066856764,46.7765780586593,47.1238898038468),
 .UNSPECIFIED.);
#2464=B_SPLINE_CURVE_WITH_KNOTS('',3,(#30660,#30661,#30662,#30663,#30664,
#30665,#30666,#30667,#30668,#30669),.UNSPECIFIED.,.F.,.F.,(4,1,1,1,1,1,
1,4),(40.8407044966673,41.3325680833161,42.330139456299,43.3277108292819,
44.3252822022649,45.3228535752478,46.3204249482307,47.1238898038468),
 .UNSPECIFIED.);
#2465=B_SPLINE_CURVE_WITH_KNOTS('',3,(#30674,#30675,#30676,#30677,#30678,
#30679,#30680,#30681,#30682,#30683,#30684),.UNSPECIFIED.,.F.,.F.,(4,1,1,
1,1,1,1,1,4),(34.5575191894876,34.8057215828641,35.803292955847,36.80086432883,
37.7984357018129,38.7960070747958,39.7935784477788,40.7911498207617,40.8407044966673),
 .UNSPECIFIED.);
#2466=B_SPLINE_CURVE_WITH_KNOTS('',3,(#30685,#30686,#30687,#30688,#30689,
#30690,#30691,#30692,#30693,#30694),.UNSPECIFIED.,.F.,.F.,(4,1,1,1,1,1,
1,4),(34.5575191894876,35.3471398454185,36.3447112184014,37.3422825913843,
38.3398539643673,39.3374253373502,40.3349967103331,40.8407044966673),
 .UNSPECIFIED.);
#2467=B_SPLINE_CURVE_WITH_KNOTS('',3,(#30699,#30700,#30701,#30702,#30703,
#30704,#30705,#30706,#30707,#30708),.UNSPECIFIED.,.F.,.F.,(4,1,1,1,1,1,
1,4),(28.2743338823081,28.8202933449665,29.8178647179494,30.8154360909324,
31.8130074639153,32.8105788368982,33.8081502098812,34.5575191894876),
 .UNSPECIFIED.);
#2468=B_SPLINE_CURVE_WITH_KNOTS('',3,(#30709,#30710,#30711,#30712,#30713,
#30714,#30715,#30716,#30717,#30718,#30719),.UNSPECIFIED.,.F.,.F.,(4,1,1,
1,1,1,1,1,4),(28.2743338823081,28.364140234538,29.3617116075209,30.3592829805038,
31.3568543534868,32.3544257264697,33.3519970994526,34.3495684724355,34.5575191894876),
 .UNSPECIFIED.);
#2469=B_SPLINE_CURVE_WITH_KNOTS('',3,(#30724,#30725,#30726,#30727,#30728,
#30729,#30730,#30731,#30732,#30733),.UNSPECIFIED.,.F.,.F.,(4,1,1,1,1,1,
1,4),(21.9911485751285,22.8348651070689,23.8324364800518,24.8300078530348,
25.8275792260177,26.8251505990006,27.8227219719836,28.2743338823081),
 .UNSPECIFIED.);
#2470=B_SPLINE_CURVE_WITH_KNOTS('',3,(#30734,#30735,#30736,#30737,#30738,
#30739,#30740,#30741,#30742,#30743),.UNSPECIFIED.,.F.,.F.,(4,1,1,1,1,1,
1,4),(21.9911485751285,22.3787119966404,23.3762833696233,24.3738547426062,
25.3714261155892,26.3689974885721,27.366568861555,28.2743338823081),
 .UNSPECIFIED.);
#2471=B_SPLINE_CURVE_WITH_KNOTS('',3,(#30749,#30750,#30751,#30752,#30753),
 .UNSPECIFIED.,.F.,.F.,(4,1,4),(14.3981410127769,15.3957123857598,15.7079632679489),
 .UNSPECIFIED.);
#2472=B_SPLINE_CURVE_WITH_KNOTS('',3,(#30756,#30757,#30758,#30759,#30760),
 .UNSPECIFIED.,.F.,.F.,(4,1,4),(13.8761928695311,14.8542941232054,15.7079632679489),
 .UNSPECIFIED.);
#2473=B_SPLINE_CURVE_WITH_KNOTS('',3,(#30766,#30767,#30768,#30769),
 .UNSPECIFIED.,.F.,.F.,(4,4),(114.40689867021,115.117908020989),
 .UNSPECIFIED.);
#2474=B_SPLINE_CURVE_WITH_KNOTS('',3,(#30777,#30778,#30779,#30780,#30781,
#30782,#30783,#30784,#30785,#30786),.UNSPECIFIED.,.F.,.F.,(4,3,3,4),(-113.097335529232,
-112.140720744584,-111.148324985783,-110.666752226423),.UNSPECIFIED.);
#2475=B_SPLINE_CURVE_WITH_KNOTS('',3,(#30791,#30792,#30793,#30794,#30795,
#30796,#30797,#30798,#30799,#30800,#30801,#30802,#30803,#30804,#30805,#30806,
#30807,#30808,#30809,#30810,#30811,#30812,#30813,#30814,#30815),
 .UNSPECIFIED.,.F.,.F.,(4,3,3,3,3,3,3,3,4),(108.12371336303,108.171137709378,
109.16353346818,110.155929226981,111.148324985783,112.140720744584,113.133116503386,
114.125512262188,114.40689867021),.UNSPECIFIED.);
#2476=B_SPLINE_CURVE_WITH_KNOTS('',3,(#30816,#30817,#30818,#30819,#30820,
#30821,#30822,#30823,#30824,#30825,#30826,#30827,#30828,#30829,#30830,#30831,
#30832,#30833,#30834,#30835,#30836,#30837),.UNSPECIFIED.,.F.,.F.,(4,3,3,
3,3,3,3,4),(-110.666752226423,-110.155929226981,-109.16353346818,-108.171137709378,
-107.178741950576,-106.186346191775,-105.193950432973,-104.383566919243),
 .UNSPECIFIED.);
#2477=B_SPLINE_CURVE_WITH_KNOTS('',3,(#30842,#30843,#30844,#30845,#30846,
#30847,#30848,#30849,#30850,#30851,#30852,#30853,#30854,#30855,#30856,#30857,
#30858,#30859,#30860,#30861,#30862,#30863),.UNSPECIFIED.,.F.,.F.,(4,3,3,
3,3,3,3,4),(101.84052805585,102.216763156568,103.20915891537,104.201554674171,
105.193950432973,106.186346191775,107.178741950576,108.12371336303),
 .UNSPECIFIED.);
#2478=B_SPLINE_CURVE_WITH_KNOTS('',3,(#30864,#30865,#30866,#30867,#30868,
#30869,#30870,#30871,#30872,#30873,#30874,#30875,#30876,#30877,#30878,#30879,
#30880,#30881,#30882,#30883,#30884,#30885,#30886,#30887,#30888),
 .UNSPECIFIED.,.F.,.F.,(4,3,3,3,3,3,3,3,4),(-104.383566919243,-104.201554674171,
-103.20915891537,-102.216763156568,-101.224367397767,-100.231971638965,
-99.2395758801633,-98.2471801213616,-98.1003816120635),.UNSPECIFIED.);
#2479=B_SPLINE_CURVE_WITH_KNOTS('',3,(#30893,#30894,#30895,#30896,#30897,
#30898,#30899,#30900,#30901,#30902,#30903,#30904,#30905,#30906,#30907,#30908,
#30909,#30910,#30911,#30912,#30913,#30914),.UNSPECIFIED.,.F.,.F.,(4,3,3,
3,3,3,3,4),(95.5573427486709,96.2623886037584,97.25478436256,98.2471801213616,
99.2395758801633,100.231971638965,101.224367397767,101.84052805585),
 .UNSPECIFIED.);
#2480=B_SPLINE_CURVE_WITH_KNOTS('',3,(#30915,#30916,#30917,#30918,#30919,
#30920,#30921,#30922,#30923,#30924,#30925,#30926,#30927,#30928,#30929,#30930,
#30931,#30932,#30933,#30934,#30935,#30936),.UNSPECIFIED.,.F.,.F.,(4,3,3,
3,3,3,3,4),(-98.1003816120635,-97.25478436256,-96.2623886037584,-95.2699928449567,
-94.2775970861551,-93.2852013273535,-92.2928055685519,-91.8171963048839),
 .UNSPECIFIED.);
#2481=B_SPLINE_CURVE_WITH_KNOTS('',3,(#30941,#30942,#30943,#30944,#30945,
#30946,#30947,#30948,#30949,#30950,#30951,#30952,#30953,#30954,#30955,#30956,
#30957,#30958,#30959,#30960,#30961,#30962,#30963,#30964,#30965),
 .UNSPECIFIED.,.F.,.F.,(4,3,3,3,3,3,3,3,4),(89.2741574414912,89.3156182921469,
90.3080140509486,91.3004098097502,92.2928055685518,93.2852013273535,94.2775970861551,
95.2699928449567,95.5573427486709),.UNSPECIFIED.);
#2482=B_SPLINE_CURVE_WITH_KNOTS('',3,(#30966,#30967,#30968,#30969,#30970,
#30971,#30972,#30973,#30974,#30975,#30976,#30977,#30978,#30979,#30980,#30981,
#30982,#30983,#30984,#30985,#30986,#30987),.UNSPECIFIED.,.F.,.F.,(4,3,3,
3,3,3,3,4),(-91.8171963048839,-91.3004098097502,-90.3080140509486,-89.315618292147,
-88.3232225333453,-87.3308267745437,-86.338431015742,-85.5340109977043),
 .UNSPECIFIED.);
#2483=B_SPLINE_CURVE_WITH_KNOTS('',3,(#30992,#30993,#30994,#30995,#30996,
#30997,#30998,#30999,#31000,#31001,#31002,#31003,#31004,#31005,#31006,#31007,
#31008,#31009,#31010,#31011,#31012,#31013),.UNSPECIFIED.,.F.,.F.,(4,3,3,
3,3,3,3,4),(82.9909721343117,83.3612437393372,84.3536394981388,85.3460352569404,
86.338431015742,87.3308267745437,88.3232225333453,89.2741574414912),
 .UNSPECIFIED.);
#2484=B_SPLINE_CURVE_WITH_KNOTS('',3,(#31014,#31015,#31016,#31017,#31018,
#31019,#31020,#31021,#31022,#31023,#31024,#31025,#31026,#31027,#31028,#31029,
#31030,#31031,#31032,#31033,#31034,#31035,#31036,#31037,#31038),
 .UNSPECIFIED.,.F.,.F.,(4,3,3,3,3,3,3,3,4),(-85.5340109977043,-85.3460352569404,
-84.3536394981388,-83.3612437393372,-82.3688479805355,-81.3764522217339,
-80.3840564629323,-79.3916607041306,-79.2508256905247),.UNSPECIFIED.);
#2485=B_SPLINE_CURVE_WITH_KNOTS('',3,(#31043,#31044,#31045,#31046,#31047,
#31048,#31049,#31050,#31051,#31052,#31053,#31054,#31055,#31056,#31057,#31058,
#31059,#31060,#31061,#31062,#31063,#31064),.UNSPECIFIED.,.F.,.F.,(4,3,3,
3,3,3,3,4),(76.7077868271321,77.4068691865273,78.399264945329,79.3916607041306,
80.3840564629322,81.3764522217339,82.3688479805355,82.9909721343117),
 .UNSPECIFIED.);
#2486=B_SPLINE_CURVE_WITH_KNOTS('',3,(#31065,#31066,#31067,#31068,#31069,
#31070,#31071,#31072,#31073,#31074,#31075,#31076,#31077,#31078,#31079,#31080,
#31081,#31082,#31083,#31084,#31085,#31086),.UNSPECIFIED.,.F.,.F.,(4,3,3,
3,3,3,3,4),(-79.2508256905247,-78.399264945329,-77.4068691865274,-76.4144734277257,
-75.4220776689241,-74.4296819101224,-73.4372861513208,-72.9676403833451),
 .UNSPECIFIED.);
#2487=B_SPLINE_CURVE_WITH_KNOTS('',3,(#31091,#31092,#31093,#31094,#31095,
#31096,#31097,#31098,#31099,#31100,#31101,#31102,#31103,#31104,#31105,#31106,
#31107,#31108,#31109,#31110,#31111,#31112,#31113,#31114,#31115),
 .UNSPECIFIED.,.F.,.F.,(4,3,3,3,3,3,3,3,4),(70.4246015199525,70.4600988749159,
71.4524946337175,72.4448903925192,73.4372861513208,74.4296819101224,75.4220776689241,
76.4144734277257,76.7077868271321),.UNSPECIFIED.);
#2488=B_SPLINE_CURVE_WITH_KNOTS('',3,(#31116,#31117,#31118,#31119,#31120,
#31121,#31122,#31123,#31124,#31125,#31126,#31127,#31128,#31129,#31130,#31131,
#31132,#31133,#31134,#31135,#31136,#31137),.UNSPECIFIED.,.F.,.F.,(4,3,3,
3,3,3,3,4),(-72.9676403833451,-72.4448903925192,-71.4524946337175,-70.4600988749159,
-69.4677031161143,-68.4753073573127,-67.482911598511,-66.6844550761655),
 .UNSPECIFIED.);
#2489=B_SPLINE_CURVE_WITH_KNOTS('',3,(#31142,#31143,#31144,#31145,#31146,
#31147,#31148,#31149,#31150,#31151,#31152,#31153,#31154,#31155,#31156,#31157,
#31158,#31159,#31160,#31161,#31162,#31163),.UNSPECIFIED.,.F.,.F.,(4,3,3,
3,3,3,3,4),(64.1414162127729,64.5057243221061,65.4981200809078,66.4905158397094,
67.482911598511,68.4753073573126,69.4677031161143,70.4246015199525),
 .UNSPECIFIED.);
#2490=B_SPLINE_CURVE_WITH_KNOTS('',3,(#31164,#31165,#31166,#31167,#31168,
#31169,#31170,#31171,#31172,#31173,#31174,#31175,#31176,#31177,#31178,#31179,
#31180,#31181,#31182,#31183,#31184,#31185,#31186,#31187,#31188),
 .UNSPECIFIED.,.F.,.F.,(4,3,3,3,3,3,3,3,4),(-66.6844550761655,-66.4905158397094,
-65.4981200809078,-64.5057243221061,-63.5133285633045,-62.5209328045029,
-61.5285370457012,-60.5361412868996,-60.4012697689859),.UNSPECIFIED.);
#2491=B_SPLINE_CURVE_WITH_KNOTS('',3,(#31193,#31194,#31195,#31196,#31197,
#31198,#31199,#31200,#31201,#31202,#31203,#31204,#31205,#31206,#31207,#31208,
#31209,#31210,#31211,#31212,#31213,#31214),.UNSPECIFIED.,.F.,.F.,(4,3,3,
3,3,3,3,4),(57.8582309055933,58.5513497692963,59.543745528098,60.5361412868996,
61.5285370457012,62.5209328045029,63.5133285633045,64.1414162127729),
 .UNSPECIFIED.);
#2492=B_SPLINE_CURVE_WITH_KNOTS('',3,(#31215,#31216,#31217,#31218,#31219,
#31220,#31221,#31222,#31223,#31224,#31225,#31226,#31227,#31228,#31229,#31230,
#31231,#31232,#31233,#31234,#31235,#31236),.UNSPECIFIED.,.F.,.F.,(4,3,3,
3,3,3,3,4),(-60.4012697689859,-59.543745528098,-58.5513497692964,-57.5589540104947,
-56.5665582516931,-55.5741624928914,-54.5817667340898,-54.1180844618063),
 .UNSPECIFIED.);
#2493=B_SPLINE_CURVE_WITH_KNOTS('',3,(#31241,#31242,#31243,#31244,#31245,
#31246,#31247,#31248,#31249,#31250,#31251,#31252,#31253,#31254,#31255,#31256,
#31257,#31258,#31259,#31260,#31261,#31262,#31263,#31264,#31265),
 .UNSPECIFIED.,.F.,.F.,(4,3,3,3,3,3,3,3,4),(51.5750455984137,51.6045794576849,
52.5969752164865,53.5893709752882,54.5817667340898,55.5741624928914,56.5665582516931,
57.5589540104947,57.8582309055933),.UNSPECIFIED.);
#2494=B_SPLINE_CURVE_WITH_KNOTS('',3,(#31266,#31267,#31268,#31269,#31270,
#31271,#31272,#31273,#31274,#31275,#31276,#31277,#31278,#31279,#31280,#31281,
#31282,#31283,#31284,#31285,#31286,#31287),.UNSPECIFIED.,.F.,.F.,(4,3,3,
3,3,3,3,4),(-54.1180844618063,-53.5893709752882,-52.5969752164865,-51.6045794576849,
-50.6121836988833,-49.6197879400816,-48.62739218128,-47.8348991546267),
 .UNSPECIFIED.);
#2495=B_SPLINE_CURVE_WITH_KNOTS('',3,(#31292,#31293,#31294,#31295,#31296,
#31297,#31298,#31299,#31300,#31301,#31302,#31303,#31304,#31305,#31306,#31307,
#31308,#31309,#31310,#31311,#31312,#31313),.UNSPECIFIED.,.F.,.F.,(4,3,3,
3,3,3,3,4),(45.2918602912341,45.6502049048751,46.6426006636767,47.6349964224784,
48.62739218128,49.6197879400816,50.6121836988833,51.5750455984137),
 .UNSPECIFIED.);
#2496=B_SPLINE_CURVE_WITH_KNOTS('',3,(#31314,#31315,#31316,#31317,#31318,
#31319,#31320,#31321,#31322,#31323,#31324,#31325,#31326,#31327,#31328,#31329,
#31330,#31331,#31332,#31333,#31334,#31335,#31336,#31337,#31338),
 .UNSPECIFIED.,.F.,.F.,(4,3,3,3,3,3,3,3,4),(-47.8348991546267,-47.6349964224784,
-46.6426006636767,-45.6502049048751,-44.6578091460735,-43.6654133872718,
-42.6730176284702,-41.6806218696686,-41.5517138474472),.UNSPECIFIED.);
#2497=B_SPLINE_CURVE_WITH_KNOTS('',3,(#31343,#31344,#31345,#31346,#31347,
#31348,#31349,#31350,#31351,#31352,#31353,#31354,#31355,#31356,#31357,#31358,
#31359,#31360,#31361,#31362,#31363,#31364),.UNSPECIFIED.,.F.,.F.,(4,3,3,
3,3,3,3,4),(39.0086749840545,39.6958303520653,40.6882261108669,41.6806218696686,
42.6730176284702,43.6654133872718,44.6578091460735,45.2918602912341),
 .UNSPECIFIED.);
#2498=B_SPLINE_CURVE_WITH_KNOTS('',3,(#31365,#31366,#31367,#31368,#31369,
#31370,#31371,#31372,#31373,#31374,#31375,#31376,#31377,#31378,#31379,#31380,
#31381,#31382,#31383,#31384,#31385,#31386),.UNSPECIFIED.,.F.,.F.,(4,3,3,
3,3,3,3,4),(-41.5517138474472,-40.6882261108669,-39.6958303520653,-38.7034345932637,
-37.711038834462,-36.7186430756604,-35.7262473168588,-35.2685285402675),
 .UNSPECIFIED.);
#2499=B_SPLINE_CURVE_WITH_KNOTS('',3,(#31391,#31392,#31393,#31394,#31395,
#31396,#31397,#31398,#31399,#31400,#31401,#31402,#31403,#31404,#31405,#31406,
#31407,#31408,#31409,#31410,#31411,#31412,#31413,#31414,#31415),
 .UNSPECIFIED.,.F.,.F.,(4,3,3,3,3,3,3,3,4),(32.725489676875,32.7490600404539,
33.7414557992555,34.7338515580571,35.7262473168588,36.7186430756604,37.711038834462,
38.7034345932637,39.0086749840545),.UNSPECIFIED.);
#2500=B_SPLINE_CURVE_WITH_KNOTS('',3,(#31416,#31417,#31418,#31419,#31420,
#31421,#31422,#31423,#31424,#31425,#31426,#31427,#31428,#31429,#31430,#31431,
#31432,#31433,#31434,#31435,#31436,#31437),.UNSPECIFIED.,.F.,.F.,(4,3,3,
3,3,3,3,4),(-35.2685285402675,-34.7338515580572,-33.7414557992555,-32.7490600404539,
-31.7566642816523,-30.7642685228506,-29.771872764049,-28.985343233088),
 .UNSPECIFIED.);
#2501=B_SPLINE_CURVE_WITH_KNOTS('',3,(#31442,#31443,#31444,#31445,#31446,
#31447,#31448,#31449,#31450,#31451,#31452,#31453,#31454,#31455,#31456,#31457,
#31458,#31459,#31460,#31461,#31462,#31463),.UNSPECIFIED.,.F.,.F.,(4,3,3,
3,3,3,3,4),(26.4423043696953,26.7946854876441,27.7870812464457,28.7794770052473,
29.771872764049,30.7642685228506,31.7566642816522,32.725489676875),
 .UNSPECIFIED.);
#2502=B_SPLINE_CURVE_WITH_KNOTS('',3,(#31464,#31465,#31466,#31467,#31468,
#31469,#31470,#31471,#31472,#31473,#31474,#31475,#31476,#31477,#31478,#31479,
#31480,#31481,#31482,#31483,#31484,#31485,#31486,#31487,#31488),
 .UNSPECIFIED.,.F.,.F.,(4,3,3,3,3,3,3,3,4),(-28.985343233088,-28.7794770052474,
-27.7870812464457,-26.7946854876441,-25.8022897288425,-24.8098939700408,
-23.8174982112392,-22.8251024524376,-22.7021579259084),.UNSPECIFIED.);
#2503=B_SPLINE_CURVE_WITH_KNOTS('',3,(#31493,#31494,#31495,#31496,#31497,
#31498,#31499,#31500,#31501,#31502,#31503,#31504,#31505,#31506,#31507,#31508,
#31509,#31510,#31511,#31512,#31513,#31514),.UNSPECIFIED.,.F.,.F.,(4,3,3,
3,3,3,3,4),(20.1591190625158,20.8403109348343,21.8327066936359,22.8251024524376,
23.8174982112392,24.8098939700408,25.8022897288424,26.4423043696953),
 .UNSPECIFIED.);
#2504=B_SPLINE_CURVE_WITH_KNOTS('',3,(#31515,#31516,#31517,#31518,#31519,
#31520,#31521,#31522,#31523,#31524,#31525,#31526,#31527,#31528,#31529,#31530,
#31531,#31532,#31533,#31534,#31535,#31536),.UNSPECIFIED.,.F.,.F.,(4,3,3,
3,3,3,3,4),(-22.7021579259084,-21.8327066936359,-20.8403109348343,-19.8479151760327,
-18.855519417231,-17.8631236584294,-16.8707278996278,-16.4189726187288),
 .UNSPECIFIED.);
#2505=B_SPLINE_CURVE_WITH_KNOTS('',3,(#31541,#31542,#31543,#31544,#31545,
#31546,#31547,#31548,#31549,#31550,#31551,#31552,#31553,#31554,#31555,#31556,
#31557,#31558,#31559,#31560,#31561,#31562,#31563,#31564,#31565),
 .UNSPECIFIED.,.F.,.F.,(4,3,3,3,3,3,3,3,4),(13.8759337553361,13.8935406232229,
14.8859363820245,15.8783321408261,16.8707278996278,17.8631236584294,18.855519417231,
19.8479151760327,20.1591190625158),.UNSPECIFIED.);
#2506=B_SPLINE_CURVE_WITH_KNOTS('',3,(#31566,#31567,#31568,#31569,#31570,
#31571,#31572,#31573,#31574,#31575,#31576,#31577,#31578,#31579,#31580,#31581,
#31582,#31583,#31584,#31585,#31586,#31587),.UNSPECIFIED.,.F.,.F.,(4,3,3,
3,3,3,3,4),(-16.4189726187288,-15.8783321408261,-14.8859363820245,-13.8935406232229,
-12.9011448644212,-11.9087491056196,-10.916353346818,-10.1357873115492),
 .UNSPECIFIED.);
#2507=B_SPLINE_CURVE_WITH_KNOTS('',3,(#31593,#31594,#31595,#31596,#31597,
#31598,#31599,#31600,#31601,#31602,#31603,#31604,#31605),.UNSPECIFIED.,
 .F.,.F.,(4,3,3,3,4),(-3.85260200436961,-2.9771872764049,-1.98479151760327,
-0.992395758801633,0.),.UNSPECIFIED.);
#2508=B_SPLINE_CURVE_WITH_KNOTS('',3,(#31608,#31609,#31610,#31611,#31612,
#31613,#31614,#31615,#31616,#31617,#31618,#31619,#31620,#31621,#31622,#31623,
#31624,#31625,#31626),.UNSPECIFIED.,.F.,.F.,(4,3,3,3,3,3,4),(2.0205724917569,
2.9771872764049,3.96958303520653,4.96197879400816,5.9543745528098,6.94677031161143,
7.59274844815659),.UNSPECIFIED.);
#2509=B_SPLINE_CURVE_WITH_KNOTS('',3,(#31632,#31633,#31634,#31635,#31636,
#31637,#31638,#31639),.UNSPECIFIED.,.F.,.F.,(4,1,1,1,1,4),(122.522113490002,
123.003686249362,123.996082008164,124.988477766965,125.980873525767,126.973269284569),
 .UNSPECIFIED.);
#2510=B_SPLINE_CURVE_WITH_KNOTS('',3,(#31642,#31643,#31644,#31645,#31646,
#31647,#31648,#31649,#31650),.UNSPECIFIED.,.F.,.F.,(4,1,1,1,1,1,4),(122.522113490002,
122.56953783635,123.561933595151,124.554329353953,125.546725112755,126.539120871556,
127.495735656204),.UNSPECIFIED.);
#2511=B_SPLINE_CURVE_WITH_KNOTS('',3,(#31655,#31656,#31657,#31658,#31659,
#31660,#31661,#31662,#31663,#31664),.UNSPECIFIED.,.F.,.F.,(4,1,1,1,1,1,
1,4),(116.238928182822,117.049311696552,118.041707455354,119.034103214156,
120.026498972957,121.018894731759,122.01129049056,122.522113490002),
 .UNSPECIFIED.);
#2512=B_SPLINE_CURVE_WITH_KNOTS('',3,(#31665,#31666,#31667,#31668,#31669,
#31670,#31671,#31672,#31673,#31674),.UNSPECIFIED.,.F.,.F.,(4,1,1,1,1,1,
1,4),(116.238928182822,116.61516328354,117.607559042342,118.599954801143,
119.592350559945,120.584746318746,121.577142077548,122.522113490002),
 .UNSPECIFIED.);
#2513=B_SPLINE_CURVE_WITH_KNOTS('',3,(#31679,#31680,#31681,#31682,#31683,
#31684,#31685,#31686,#31687,#31688,#31689),.UNSPECIFIED.,.F.,.F.,(4,1,1,
1,1,1,1,1,4),(109.955742875643,110.102541384941,111.094937143743,112.087332902544,
113.079728661346,114.072124420147,115.064520178949,116.056915937751,116.238928182822),
 .UNSPECIFIED.);
#2514=B_SPLINE_CURVE_WITH_KNOTS('',3,(#31690,#31691,#31692,#31693,#31694,
#31695,#31696,#31697,#31698,#31699),.UNSPECIFIED.,.F.,.F.,(4,1,1,1,1,1,
1,4),(109.955742875643,110.66078873073,111.653184489532,112.645580248333,
113.637976007135,114.630371765937,115.622767524738,116.238928182822),
 .UNSPECIFIED.);
#2515=B_SPLINE_CURVE_WITH_KNOTS('',3,(#31704,#31705,#31706,#31707,#31708,
#31709,#31710,#31711,#31712,#31713),.UNSPECIFIED.,.F.,.F.,(4,1,1,1,1,1,
1,4),(103.672557568463,104.148166832131,105.140562590933,106.132958349734,
107.125354108536,108.117749867338,109.110145626139,109.955742875643),
 .UNSPECIFIED.);
#2516=B_SPLINE_CURVE_WITH_KNOTS('',3,(#31714,#31715,#31716,#31717,#31718,
#31719,#31720,#31721,#31722,#31723,#31724),.UNSPECIFIED.,.F.,.F.,(4,1,1,
1,1,1,1,1,4),(103.672557568463,103.714018419119,104.70641417792,105.698809936722,
106.691205695524,107.683601454325,108.675997213127,109.668392971929,109.955742875643),
 .UNSPECIFIED.);
#2517=B_SPLINE_CURVE_WITH_KNOTS('',3,(#31729,#31730,#31731,#31732,#31733,
#31734,#31735,#31736,#31737,#31738),.UNSPECIFIED.,.F.,.F.,(4,1,1,1,1,1,
1,4),(97.3893722612835,98.1937922793213,99.1861880381229,100.178583796925,
101.170979555726,102.163375314528,103.155771073329,103.672557568463),
 .UNSPECIFIED.);
#2518=B_SPLINE_CURVE_WITH_KNOTS('',3,(#31739,#31740,#31741,#31742,#31743,
#31744,#31745,#31746,#31747,#31748),.UNSPECIFIED.,.F.,.F.,(4,1,1,1,1,1,
1,4),(97.3893722612835,97.7596438663089,98.7520396251105,99.7444353839122,
100.736831142714,101.729226901515,102.721622660317,103.672557568463),
 .UNSPECIFIED.);
#2519=B_SPLINE_CURVE_WITH_KNOTS('',3,(#31753,#31754,#31755,#31756,#31757,
#31758,#31759,#31760,#31761,#31762,#31763),.UNSPECIFIED.,.F.,.F.,(4,1,1,
1,1,1,1,1,4),(91.106186954104,91.2470219677099,92.2394177265115,93.2318134853131,
94.2242092441148,95.2166050029164,96.209000761718,97.2013965205197,97.3893722612835),
 .UNSPECIFIED.);
#2520=B_SPLINE_CURVE_WITH_KNOTS('',3,(#31764,#31765,#31766,#31767,#31768,
#31769,#31770,#31771,#31772,#31773),.UNSPECIFIED.,.F.,.F.,(4,1,1,1,1,1,
1,4),(91.106186954104,91.8052693134991,92.7976650723007,93.7900608311024,
94.782456589904,95.7748523487057,96.7672481075073,97.3893722612835),
 .UNSPECIFIED.);
#2521=B_SPLINE_CURVE_WITH_KNOTS('',3,(#31778,#31779,#31780,#31781,#31782,
#31783,#31784,#31785,#31786,#31787),.UNSPECIFIED.,.F.,.F.,(4,1,1,1,1,1,
1,4),(84.8230016469243,85.2926474149001,86.2850431737017,87.2774389325033,
88.269834691305,89.2622304501066,90.2546262089082,91.106186954104),
 .UNSPECIFIED.);
#2522=B_SPLINE_CURVE_WITH_KNOTS('',3,(#31788,#31789,#31790,#31791,#31792,
#31793,#31794,#31795,#31796,#31797,#31798),.UNSPECIFIED.,.F.,.F.,(4,1,1,
1,1,1,1,1,4),(84.8230016469243,84.8584990018877,85.8508947606893,86.8432905194909,
87.8356862782926,88.8280820370942,89.8204777958959,90.8128735546975,91.106186954104),
 .UNSPECIFIED.);
#2523=B_SPLINE_CURVE_WITH_KNOTS('',3,(#31803,#31804,#31805,#31806,#31807,
#31808,#31809,#31810,#31811,#31812),.UNSPECIFIED.,.F.,.F.,(4,1,1,1,1,1,
1,4),(78.5398163397448,79.3382728620903,80.3306686208919,81.3230643796935,
82.3154601384952,83.3078558972968,84.3002516560985,84.8230016469243),
 .UNSPECIFIED.);
#2524=B_SPLINE_CURVE_WITH_KNOTS('',3,(#31813,#31814,#31815,#31816,#31817,
#31818,#31819,#31820,#31821,#31822),.UNSPECIFIED.,.F.,.F.,(4,1,1,1,1,1,
1,4),(78.5398163397448,78.9041244490779,79.8965202078795,80.8889159666812,
81.8813117254828,82.8737074842844,83.8661032430861,84.8230016469243),
 .UNSPECIFIED.);
#2525=B_SPLINE_CURVE_WITH_KNOTS('',3,(#31827,#31828,#31829,#31830,#31831,
#31832,#31833,#31834,#31835,#31836,#31837),.UNSPECIFIED.,.F.,.F.,(4,1,1,
1,1,1,1,1,4),(72.2566310325651,72.3915025504788,73.3838983092805,74.3762940680821,
75.3686898268838,76.3610855856854,77.353481344487,78.3458771032886,78.5398163397448),
 .UNSPECIFIED.);
#2526=B_SPLINE_CURVE_WITH_KNOTS('',3,(#31838,#31839,#31840,#31841,#31842,
#31843,#31844,#31845,#31846,#31847),.UNSPECIFIED.,.F.,.F.,(4,1,1,1,1,1,
1,4),(72.2566310325651,72.9497498962681,73.9421456550697,74.9345414138714,
75.926937172673,76.9193329314746,77.9117286902763,78.5398163397448),
 .UNSPECIFIED.);
#2527=B_SPLINE_CURVE_WITH_KNOTS('',3,(#31852,#31853,#31854,#31855,#31856,
#31857,#31858,#31859,#31860,#31861),.UNSPECIFIED.,.F.,.F.,(4,1,1,1,1,1,
1,4),(65.9734457253856,66.4371279976691,67.4295237564707,68.4219195152723,
69.4143152740739,70.4067110328756,71.3991067916772,72.2566310325651),
 .UNSPECIFIED.);
#2528=B_SPLINE_CURVE_WITH_KNOTS('',3,(#31862,#31863,#31864,#31865,#31866,
#31867,#31868,#31869,#31870,#31871,#31872),.UNSPECIFIED.,.F.,.F.,(4,1,1,
1,1,1,1,1,4),(65.9734457253856,66.0029795846567,66.9953753434583,67.9877711022599,
68.9801668610616,69.9725626198632,70.9649583786648,71.9573541374665,72.2566310325651),
 .UNSPECIFIED.);
#2529=B_SPLINE_CURVE_WITH_KNOTS('',3,(#31877,#31878,#31879,#31880,#31881,
#31882,#31883,#31884,#31885,#31886),.UNSPECIFIED.,.F.,.F.,(4,1,1,1,1,1,
1,4),(59.690260418206,60.4827534448593,61.4751492036609,62.4675449624625,
63.4599407212642,64.4523364800658,65.4447322388674,65.9734457253856),
 .UNSPECIFIED.);
#2530=B_SPLINE_CURVE_WITH_KNOTS('',3,(#31887,#31888,#31889,#31890,#31891,
#31892,#31893,#31894,#31895,#31896),.UNSPECIFIED.,.F.,.F.,(4,1,1,1,1,1,
1,4),(59.690260418206,60.0486050318469,61.0410007906485,62.0333965494501,
63.0257923082518,64.0181880670534,65.010583825855,65.9734457253856),
 .UNSPECIFIED.);
#2531=B_SPLINE_CURVE_WITH_KNOTS('',3,(#31901,#31902,#31903,#31904,#31905,
#31906,#31907,#31908,#31909,#31910,#31911),.UNSPECIFIED.,.F.,.F.,(4,1,1,
1,1,1,1,1,4),(53.4070751110264,53.5359831332478,54.5283788920495,55.5207746508511,
56.5131704096527,57.5055661684544,58.497961927256,59.4903576860576,59.690260418206),
 .UNSPECIFIED.);
#2532=B_SPLINE_CURVE_WITH_KNOTS('',3,(#31912,#31913,#31914,#31915,#31916,
#31917,#31918,#31919,#31920,#31921),.UNSPECIFIED.,.F.,.F.,(4,1,1,1,1,1,
1,4),(53.4070751110264,54.0942304790371,55.0866262378387,56.0790219966403,
57.071417755442,58.0638135142436,59.0562092730452,59.690260418206),
 .UNSPECIFIED.);
#2533=B_SPLINE_CURVE_WITH_KNOTS('',3,(#31926,#31927,#31928,#31929,#31930,
#31931,#31932,#31933,#31934,#31935),.UNSPECIFIED.,.F.,.F.,(4,1,1,1,1,1,
1,4),(47.1238898038468,47.581608580438,48.5740043392397,49.5664000980413,
50.5587958568429,51.5511916156446,52.5435873744462,53.4070751110264),
 .UNSPECIFIED.);
#2534=B_SPLINE_CURVE_WITH_KNOTS('',3,(#31936,#31937,#31938,#31939,#31940,
#31941,#31942,#31943,#31944,#31945,#31946),.UNSPECIFIED.,.F.,.F.,(4,1,1,
1,1,1,1,1,4),(47.1238898038468,47.1474601674257,48.1398559262273,49.1322516850289,
50.1246474438306,51.1170432026322,52.1094389614338,53.1018347202355,53.4070751110264),
 .UNSPECIFIED.);
#2535=B_SPLINE_CURVE_WITH_KNOTS('',3,(#31951,#31952,#31953,#31954,#31955,
#31956,#31957,#31958,#31959,#31960),.UNSPECIFIED.,.F.,.F.,(4,1,1,1,1,1,
1,4),(40.8407044966672,41.6272340276282,42.6196297864299,43.6120255452315,
44.6044213040331,45.5968170628348,46.5892128216364,47.1238898038468),
 .UNSPECIFIED.);
#2536=B_SPLINE_CURVE_WITH_KNOTS('',3,(#31961,#31962,#31963,#31964,#31965,
#31966,#31967,#31968,#31969,#31970),.UNSPECIFIED.,.F.,.F.,(4,1,1,1,1,1,
1,4),(40.8407044966672,41.1930856146159,42.1854813734175,43.1778771322191,
44.1702728910208,45.1626686498224,46.155064408624,47.1238898038468),
 .UNSPECIFIED.);
#2537=B_SPLINE_CURVE_WITH_KNOTS('',3,(#31975,#31976,#31977,#31978,#31979,
#31980,#31981,#31982,#31983,#31984,#31985),.UNSPECIFIED.,.F.,.F.,(4,1,1,
1,1,1,1,1,4),(34.5575191894876,34.6804637160168,35.6728594748184,36.6652552336201,
37.6576509924217,38.6500467512233,39.642442510025,40.6348382688266,40.8407044966672),
 .UNSPECIFIED.);
#2538=B_SPLINE_CURVE_WITH_KNOTS('',3,(#31986,#31987,#31988,#31989,#31990,
#31991,#31992,#31993,#31994,#31995),.UNSPECIFIED.,.F.,.F.,(4,1,1,1,1,1,
1,4),(34.5575191894876,35.2387110618061,36.2311068206077,37.2235025794093,
38.215898338211,39.2082940970126,40.2006898558142,40.8407044966672),
 .UNSPECIFIED.);
#2539=B_SPLINE_CURVE_WITH_KNOTS('',3,(#32000,#32001,#32002,#32003,#32004,
#32005,#32006,#32007,#32008,#32009),.UNSPECIFIED.,.F.,.F.,(4,1,1,1,1,1,
1,4),(28.274333882308,28.726089163207,29.7184849220086,30.7108806808103,
31.7032764396119,32.6956721984135,33.6880679572152,34.5575191894876),
 .UNSPECIFIED.);
#2540=B_SPLINE_CURVE_WITH_KNOTS('',3,(#32010,#32011,#32012,#32013,#32014,
#32015,#32016,#32017,#32018,#32019,#32020),.UNSPECIFIED.,.F.,.F.,(4,1,1,
1,1,1,1,1,4),(28.274333882308,28.2919407501946,29.2843365089963,30.2767322677979,
31.2691280265995,32.2615237854012,33.2539195442028,34.2463153030044,34.5575191894876),
 .UNSPECIFIED.);
#2541=B_SPLINE_CURVE_WITH_KNOTS('',3,(#32025,#32026,#32027,#32028,#32029,
#32030,#32031,#32032,#32033,#32034),.UNSPECIFIED.,.F.,.F.,(4,1,1,1,1,1,
1,4),(21.9911485751284,22.7717146103972,23.7641103691988,24.7565061280005,
25.7489018868021,26.7412976456037,27.7336934044054,28.274333882308),
 .UNSPECIFIED.);
#2542=B_SPLINE_CURVE_WITH_KNOTS('',3,(#32035,#32036,#32037,#32038,#32039,
#32040,#32041,#32042,#32043,#32044),.UNSPECIFIED.,.F.,.F.,(4,1,1,1,1,1,
1,4),(21.9911485751284,22.3375661973848,23.3299619561865,24.3223577149881,
25.3147534737897,26.3071492325914,27.299544991393,28.274333882308),
 .UNSPECIFIED.);
#2543=B_SPLINE_CURVE_WITH_KNOTS('',3,(#32050,#32051,#32052,#32053,#32054),
 .UNSPECIFIED.,.F.,.F.,(4,1,4),(14.3984001269718,15.3907958857734,15.7079632679489),
 .UNSPECIFIED.);
#2544=B_SPLINE_CURVE_WITH_KNOTS('',3,(#32057,#32058,#32059,#32060,#32061),
 .UNSPECIFIED.,.F.,.F.,(4,1,4),(13.8759337553361,14.8325485399841,15.7079632679489),
 .UNSPECIFIED.);
#2545=B_SPLINE_CURVE_WITH_KNOTS('',3,(#32063,#32064,#32065,#32066,#32067,
#32068,#32069,#32070,#32071,#32072,#32073,#32074,#32075,#32076,#32077,#32078,
#32079,#32080,#32081,#32082,#32083,#32084,#32085,#32086,#32087,#32088,#32089,
#32090,#32091,#32092,#32093,#32094,#32095,#32096,#32097,#32098,#32099,#32100,
#32101,#32102,#32103,#32104,#32105,#32106,#32107,#32108,#32109,#32110,#32111,
#32112,#32113,#32114),.UNSPECIFIED.,.F.,.F.,(4,3,3,3,3,3,3,3,3,3,3,3,3,
3,3,3,3,4),(-0.286347380332279,-0.266347789416864,-0.254098115456061,-0.230501751705225,
-0.216536610693349,-0.18668269284242,-0.173443188538191,-0.164130900566406,
-0.152678732927651,-0.129952909210668,-0.116365164485228,-0.106745630798174,
-0.0814440134366876,-0.0640046809373957,-0.0520446962100768,-0.0197039455308333,
-0.00553916135222766,0.),.UNSPECIFIED.);
#2546=B_SPLINE_CURVE_WITH_KNOTS('',3,(#32115,#32116,#32117,#32118,#32119,
#32120,#32121,#32122,#32123,#32124,#32125,#32126,#32127,#32128,#32129,#32130,
#32131,#32132,#32133,#32134,#32135,#32136,#32137,#32138,#32139,#32140,#32141,
#32142,#32143,#32144,#32145,#32146,#32147,#32148,#32149,#32150,#32151,#32152,
#32153,#32154,#32155,#32156,#32157,#32158,#32159,#32160,#32161,#32162,#32163,
#32164,#32165,#32166,#32167,#32168,#32169),.UNSPECIFIED.,.F.,.F.,(4,3,3,
3,3,3,3,3,3,3,3,3,3,3,3,3,3,3,4),(-0.2851428039951,-0.264876660632172,-0.2498967274825,
-0.236025660645345,-0.214587312757531,-0.204671023974553,-0.173775777047669,
-0.160111619860766,-0.150128525406277,-0.138317788758425,-0.118237251615849,
-0.10321155298755,-0.092840846421164,-0.0707715126256338,-0.0558839316601653,
-0.043797399607841,-0.0161434201156718,-0.00456351123904309,0.),
 .UNSPECIFIED.);
#2547=B_SPLINE_CURVE_WITH_KNOTS('',3,(#32171,#32172,#32173,#32174,#32175,
#32176,#32177,#32178,#32179,#32180,#32181),.UNSPECIFIED.,.F.,.F.,(4,1,1,
1,1,1,1,1,4),(15.7079632679489,15.8249442987858,16.8173400575874,17.809735816389,
18.8021315751907,19.7945273339923,20.7869230927939,21.7793188515956,21.9911485751284),
 .UNSPECIFIED.);
#2548=B_SPLINE_CURVE_WITH_KNOTS('',3,(#32182,#32183,#32184,#32185,#32186,
#32187,#32188,#32189,#32190,#32191),.UNSPECIFIED.,.F.,.F.,(4,1,1,1,1,1,
1,4),(15.7079632679489,16.383191644575,17.3755874033767,18.3679831621783,
19.3603789209799,20.3527746797816,21.3451704385832,21.9911485751284),
 .UNSPECIFIED.);
#2549=B_SPLINE_CURVE_WITH_KNOTS('',3,(#32668,#32669,#32670,#32671,#32672,
#32673,#32674,#32675,#32676,#32677,#32678,#32679,#32680,#32681,#32682,#32683,
#32684,#32685,#32686,#32687,#32688,#32689,#32690,#32691,#32692,#32693,#32694,
#32695,#32696,#32697,#32698,#32699,#32700,#32701,#32702,#32703,#32704,#32705,
#32706,#32707,#32708,#32709,#32710,#32711,#32712,#32713,#32714,#32715,#32716),
 .UNSPECIFIED.,.F.,.F.,(4,3,3,3,3,3,3,3,3,3,3,3,3,3,3,3,4),(0.,0.027427935344833,
0.0485975213880563,0.057338544085104,0.0868715743464506,0.0993492225585254,
0.10874754786483,0.133259321258805,0.148225404936155,0.157073224224447,
0.187711488807199,0.203788900709552,0.214227532674886,0.239511221647469,
0.25730153039039,0.279626282555456,0.285142803995123),.UNSPECIFIED.);
#2550=B_SPLINE_CURVE_WITH_KNOTS('',3,(#32717,#32718,#32719,#32720,#32721,
#32722,#32723,#32724,#32725,#32726,#32727,#32728,#32729,#32730,#32731,#32732,
#32733,#32734,#32735,#32736,#32737,#32738,#32739,#32740,#32741),
 .UNSPECIFIED.,.F.,.F.,(4,3,3,3,3,3,3,3,4),(-10.1357873115492,-9.92395758801633,
-8.9315618292147,-7.93916607041306,-6.94677031161143,-5.9543745528098,-4.96197879400816,
-3.96958303520653,-3.85260200436961),.UNSPECIFIED.);
#2551=B_SPLINE_CURVE_WITH_KNOTS('',3,(#33218,#33219,#33220,#33221,#33222,
#33223,#33224,#33225,#33226,#33227,#33228,#33229,#33230,#33231,#33232,#33233,
#33234,#33235,#33236,#33237,#33238,#33239),.UNSPECIFIED.,.F.,.F.,(4,3,3,
3,3,3,3,4),(7.59274844815659,7.93916607041306,8.9315618292147,9.92395758801632,
10.916353346818,11.9087491056196,12.9011448644212,13.8759337553361),
 .UNSPECIFIED.);
#2552=B_SPLINE_CURVE_WITH_KNOTS('',3,(#33240,#33241,#33242,#33243,#33244,
#33245,#33246,#33247,#33248,#33249,#33250,#33251,#33252,#33253,#33254,#33255,
#33256,#33257,#33258,#33259,#33260,#33261,#33262,#33263,#33264,#33265,#33266,
#33267,#33268,#33269,#33270,#33271,#33272,#33273,#33274,#33275,#33276,#33277,
#33278,#33279,#33280,#33281,#33282,#33283,#33284,#33285,#33286,#33287,#33288),
 .UNSPECIFIED.,.F.,.F.,(4,3,3,3,3,3,3,3,3,3,3,3,3,3,3,3,4),(0.,0.0320359961493654,
0.0578351282991586,0.0686833515155324,0.0999463544758613,0.113502099149543,
0.123023834848469,0.14759884188358,0.169881710030997,0.180117784856696,
0.205530503004595,0.220530951880297,0.231030371326071,0.247789211594336,
0.263619336128737,0.281768657448294,0.286347380332258),.UNSPECIFIED.);
#2553=B_SPLINE_CURVE_WITH_KNOTS('',3,(#33292,#33293,#33294,#33295,#33296,
#33297,#33298,#33299,#33300,#33301,#33302,#33303,#33304,#33305,#33306,#33307,
#33308,#33309,#33310,#33311,#33312,#33313,#33314,#33315,#33316,#33317,#33318,
#33319,#33320,#33321,#33322,#33323,#33324,#33325,#33326,#33327,#33328,#33329,
#33330,#33331,#33332,#33333,#33334,#33335,#33336,#33337,#33338,#33339,#33340,
#33341,#33342,#33343,#33344,#33345,#33346),.UNSPECIFIED.,.F.,.F.,(4,3,3,
3,3,3,3,3,3,3,3,3,3,3,3,3,3,3,4),(-0.378621596831434,-0.353562249903933,
-0.339726595154467,-0.324795073175994,-0.299958563910779,-0.289109739323556,
-0.25235894447449,-0.234461207277299,-0.219335840287605,-0.20082949567809,
-0.174834335133969,-0.155874235881852,-0.144961055903939,-0.109724944879178,
-0.089723852283725,-0.0773553386782937,-0.0372306048514265,-0.00401661180489575,
0.),.UNSPECIFIED.);
#2554=B_SPLINE_CURVE_WITH_KNOTS('',3,(#33347,#33348,#33349,#33350,#33351,
#33352,#33353,#33354,#33355,#33356,#33357,#33358,#33359,#33360,#33361,#33362,
#33363,#33364,#33365,#33366,#33367,#33368,#33369,#33370,#33371,#33372,#33373,
#33374,#33375,#33376,#33377,#33378,#33379,#33380,#33381,#33382,#33383,#33384,
#33385,#33386,#33387,#33388,#33389,#33390,#33391,#33392,#33393,#33394,#33395,
#33396,#33397,#33398,#33399,#33400,#33401),.UNSPECIFIED.,.F.,.F.,(4,3,3,
3,3,3,3,3,3,3,3,3,3,3,3,3,3,3,4),(-0.376940817211603,-0.35160224691684,
-0.332515709335319,-0.31822436103578,-0.288310916204436,-0.272711478712379,
-0.234501138719602,-0.216951876329547,-0.20548608487052,-0.180854828870935,
-0.153741722238776,-0.136717958714649,-0.126362699189128,-0.0955896266494597,
-0.0668165609022854,-0.0558907541314208,-0.0219997397314357,-0.00327040903045418,
0.),.UNSPECIFIED.);
#2555=B_SPLINE_CURVE_WITH_KNOTS('',3,(#33403,#33404,#33405,#33406,#33407,
#33408,#33409,#33410,#33411,#33412,#33413),.UNSPECIFIED.,.F.,.F.,(4,1,1,
1,1,1,1,1,4),(15.7079632679489,15.8518654961884,16.8494368691713,17.8470082421542,
18.8445796151372,19.8421509881201,20.839722361103,21.837293734086,21.9911485751285),
 .UNSPECIFIED.);
#2556=B_SPLINE_CURVE_WITH_KNOTS('',3,(#33414,#33415,#33416,#33417,#33418,
#33419,#33420,#33421,#33422,#33423),.UNSPECIFIED.,.F.,.F.,(4,1,1,1,1,1,
1,4),(15.7079632679489,16.3932837587428,17.3908551317257,18.3884265047086,
19.3859978776916,20.3835692506745,21.3811406236574,21.9911485751285),
 .UNSPECIFIED.);
#2557=B_SPLINE_CURVE_WITH_KNOTS('',3,(#33768,#33769,#33770,#33771,#33772,
#33773,#33774,#33775,#33776,#33777,#33778,#33779,#33780,#33781,#33782,#33783,
#33784,#33785,#33786,#33787,#33788,#33789,#33790,#33791,#33792,#33793,#33794,
#33795,#33796,#33797,#33798,#33799,#33800,#33801,#33802,#33803,#33804,#33805,
#33806,#33807,#33808,#33809,#33810,#33811,#33812,#33813,#33814,#33815,#33816,
#33817,#33818,#33819),.UNSPECIFIED.,.F.,.F.,(4,3,3,3,3,3,3,3,3,3,3,3,3,
3,3,3,3,4),(0.,0.0336989330766502,0.058737806914676,0.0734856897216009,
0.109795026944167,0.13287001176372,0.143641059388719,0.177205256270034,
0.195910789941764,0.207613330853891,0.24488927972035,0.269584354829063,
0.282495236861346,0.310139624218381,0.327566593080831,0.34255192583909,
0.372940760482297,0.376940817211641),.UNSPECIFIED.);
#2558=B_SPLINE_CURVE_WITH_KNOTS('',3,(#33820,#33821,#33822,#33823,#33824,
#33825,#33826,#33827,#33828,#33829,#33830,#33831,#33832,#33833,#33834,#33835,
#33836,#33837,#33838,#33839,#33840,#33841,#33842,#33843,#33844),
 .UNSPECIFIED.,.F.,.F.,(4,3,3,3,3,3,3,3,4),(-10.1295685708718,-9.97571372982933,
-8.9781423568464,-7.98057098386346,-6.98299961088053,-5.9854282378976,-4.98785686491466,
-3.99028549193173,-3.84638326369226),.UNSPECIFIED.);
#2559=B_SPLINE_CURVE_WITH_KNOTS('',3,(#34189,#34190,#34191,#34192,#34193,
#34194,#34195,#34196,#34197,#34198,#34199,#34200,#34201,#34202,#34203,#34204,
#34205,#34206,#34207,#34208,#34209,#34210),.UNSPECIFIED.,.F.,.F.,(4,3,3,
3,3,3,3,4),(7.59300756235155,7.98057098386346,8.9781423568464,9.97571372982933,
10.9732851028123,11.9708564757952,12.9684278487781,13.8761928695311),
 .UNSPECIFIED.);
#2560=B_SPLINE_CURVE_WITH_KNOTS('',3,(#34211,#34212,#34213,#34214,#34215,
#34216,#34217,#34218,#34219,#34220,#34221,#34222,#34223,#34224,#34225,#34226,
#34227,#34228,#34229,#34230,#34231,#34232,#34233,#34234,#34235,#34236,#34237,
#34238,#34239,#34240,#34241,#34242,#34243,#34244,#34245,#34246,#34247,#34248,
#34249,#34250,#34251,#34252,#34253,#34254,#34255,#34256,#34257,#34258,#34259,
#34260,#34261,#34262),.UNSPECIFIED.,.F.,.F.,(4,3,3,3,3,3,3,3,3,3,3,3,3,
3,3,3,3,4),(0.,0.0396836996751474,0.0598295377036724,0.0776045542344442,
0.089287041955902,0.127960856426141,0.1530367876033,0.165008599097631,0.197163594226426,
0.224449840232547,0.234157399588655,0.269452851616206,0.2876129966593,0.30541494242687,
0.333061769489462,0.34722178230466,0.375339207698859,0.378621596831421),
 .UNSPECIFIED.);
#2561=B_SPLINE_CURVE_WITH_KNOTS('',3,(#34297,#34298,#34299,#34300),
 .UNSPECIFIED.,.F.,.F.,(4,4),(64.1414162127729,64.8524255635527),
 .UNSPECIFIED.);
#2562=B_SPLINE_CURVE_WITH_KNOTS('',3,(#34308,#34309,#34310,#34311,#34312,
#34313,#34314,#34315,#34316,#34317),.UNSPECIFIED.,.F.,.F.,(4,3,3,4),(-62.8318530717959,
-61.8592366913888,-60.8615070673342,-60.401269768986),.UNSPECIFIED.);
#2563=B_SPLINE_CURVE_WITH_KNOTS('',3,(#34322,#34323,#34324,#34325,#34326,
#34327,#34328,#34329,#34330,#34331,#34332,#34333,#34334,#34335,#34336,#34337,
#34338,#34339,#34340,#34341,#34342,#34343,#34344,#34345,#34346),
 .UNSPECIFIED.,.F.,.F.,(4,3,3,3,3,3,3,3,4),(57.8582309055934,57.8683181951701,
58.8660478192247,59.8637774432794,60.861507067334,61.8592366913887,62.8569663154434,
63.854695939498,64.1414162127729),.UNSPECIFIED.);
#2564=B_SPLINE_CURVE_WITH_KNOTS('',3,(#34347,#34348,#34349,#34350,#34351,
#34352,#34353,#34354,#34355,#34356,#34357,#34358,#34359,#34360,#34361,#34362,
#34363,#34364,#34365,#34366,#34367,#34368),.UNSPECIFIED.,.F.,.F.,(4,3,3,
3,3,3,3,4),(-60.401269768986,-59.8637774432795,-58.8660478192248,-57.8683181951702,
-56.8705885711155,-55.8728589470609,-54.8751293230062,-54.1180844618064),
 .UNSPECIFIED.);
#2565=B_SPLINE_CURVE_WITH_KNOTS('',3,(#34373,#34374,#34375,#34376,#34377,
#34378,#34379,#34380,#34381,#34382,#34383,#34384,#34385,#34386,#34387,#34388,
#34389,#34390,#34391,#34392,#34393,#34394),.UNSPECIFIED.,.F.,.F.,(4,3,3,
3,3,3,3,4),(51.5750455984138,51.8819404508421,52.8796700748968,53.8773996989514,
54.8751293230061,55.8728589470608,56.8705885711154,57.8582309055934),
 .UNSPECIFIED.);
#2566=B_SPLINE_CURVE_WITH_KNOTS('',3,(#34395,#34396,#34397,#34398,#34399,
#34400,#34401,#34402,#34403,#34404,#34405,#34406,#34407,#34408,#34409,#34410,
#34411,#34412,#34413,#34414,#34415,#34416,#34417,#34418,#34419),
 .UNSPECIFIED.,.F.,.F.,(4,3,3,3,3,3,3,3,4),(-54.1180844618064,-53.8773996989516,
-52.8796700748969,-51.8819404508422,-50.8842108267876,-49.8864812027329,
-48.8887515786783,-47.8910219546236,-47.8348991546268),.UNSPECIFIED.);
#2567=B_SPLINE_CURVE_WITH_KNOTS('',3,(#34424,#34425,#34426,#34427,#34428,
#34429,#34430,#34431,#34432,#34433,#34434,#34435,#34436,#34437,#34438,#34439,
#34440,#34441,#34442,#34443,#34444,#34445),.UNSPECIFIED.,.F.,.F.,(4,3,3,
3,3,3,3,4),(45.2918602912342,45.8955627065142,46.8932923305688,47.8910219546235,
48.8887515786782,49.8864812027328,50.8842108267875,51.5750455984138),
 .UNSPECIFIED.);
#2568=B_SPLINE_CURVE_WITH_KNOTS('',3,(#34446,#34447,#34448,#34449,#34450,
#34451,#34452,#34453,#34454,#34455,#34456,#34457,#34458,#34459,#34460,#34461,
#34462,#34463,#34464,#34465,#34466,#34467),.UNSPECIFIED.,.F.,.F.,(4,3,3,
3,3,3,3,4),(-47.8348991546268,-46.8932923305689,-45.8955627065143,-44.8978330824596,
-43.900103458405,-42.9023738343503,-41.9046442102957,-41.5517138474472),
 .UNSPECIFIED.);
#2569=B_SPLINE_CURVE_WITH_KNOTS('',3,(#34472,#34473,#34474,#34475,#34476,
#34477,#34478,#34479,#34480,#34481,#34482,#34483,#34484,#34485,#34486,#34487,
#34488,#34489,#34490,#34491,#34492,#34493),.UNSPECIFIED.,.F.,.F.,(4,3,3,
3,3,3,3,4),(39.0086749840546,39.9091849621863,40.9069145862409,41.9046442102956,
42.9023738343502,43.9001034584049,44.8978330824595,45.2918602912342),
 .UNSPECIFIED.);
#2570=B_SPLINE_CURVE_WITH_KNOTS('',3,(#34494,#34495,#34496,#34497,#34498,
#34499,#34500,#34501,#34502,#34503,#34504,#34505,#34506,#34507,#34508,#34509,
#34510,#34511,#34512,#34513,#34514,#34515),.UNSPECIFIED.,.F.,.F.,(4,3,3,
3,3,3,3,4),(-41.5517138474472,-40.906914586241,-39.9091849621863,-38.9114553381317,
-37.913725714077,-36.9159960900224,-35.9182664659677,-35.2685285402676),
 .UNSPECIFIED.);
#2571=B_SPLINE_CURVE_WITH_KNOTS('',3,(#34520,#34521,#34522,#34523,#34524,
#34525,#34526,#34527,#34528,#34529,#34530,#34531,#34532,#34533,#34534,#34535,
#34536,#34537,#34538,#34539,#34540,#34541,#34542,#34543,#34544),
 .UNSPECIFIED.,.F.,.F.,(4,3,3,3,3,3,3,3,4),(32.725489676875,32.9250775938037,
33.9228072178583,34.920536841913,35.9182664659676,36.9159960900223,37.9137257140769,
38.9114553381316,39.0086749840546),.UNSPECIFIED.);
#2572=B_SPLINE_CURVE_WITH_KNOTS('',3,(#34545,#34546,#34547,#34548,#34549,
#34550,#34551,#34552,#34553,#34554,#34555,#34556,#34557,#34558,#34559,#34560,
#34561,#34562,#34563,#34564,#34565,#34566),.UNSPECIFIED.,.F.,.F.,(4,3,3,
3,3,3,3,4),(-35.2685285402676,-34.920536841913,-33.9228072178584,-32.9250775938037,
-31.9273479697491,-30.9296183456944,-29.9318887216397,-28.985343233088),
 .UNSPECIFIED.);
#2573=B_SPLINE_CURVE_WITH_KNOTS('',3,(#34571,#34572,#34573,#34574,#34575,
#34576,#34577,#34578,#34579,#34580,#34581,#34582,#34583,#34584,#34585,#34586,
#34587,#34588,#34589,#34590,#34591,#34592),.UNSPECIFIED.,.F.,.F.,(4,3,3,
3,3,3,3,4),(26.4423043696954,26.9386998494757,27.9364294735304,28.934159097585,
29.9318887216397,30.9296183456943,31.927347969749,32.725489676875),
 .UNSPECIFIED.);
#2574=B_SPLINE_CURVE_WITH_KNOTS('',3,(#34593,#34594,#34595,#34596,#34597,
#34598,#34599,#34600,#34601,#34602,#34603,#34604,#34605,#34606,#34607,#34608,
#34609,#34610,#34611,#34612,#34613,#34614,#34615,#34616,#34617),
 .UNSPECIFIED.,.F.,.F.,(4,3,3,3,3,3,3,3,4),(-28.985343233088,-28.9341590975851,
-27.9364294735304,-26.9386998494758,-25.9409702254211,-24.9432406013665,
-23.9455109773118,-22.9477813532571,-22.7021579259084),.UNSPECIFIED.);
#2575=B_SPLINE_CURVE_WITH_KNOTS('',3,(#34622,#34623,#34624,#34625,#34626,
#34627,#34628,#34629,#34630,#34631,#34632,#34633,#34634,#34635,#34636,#34637,
#34638,#34639,#34640,#34641,#34642,#34643),.UNSPECIFIED.,.F.,.F.,(4,3,3,
3,3,3,3,4),(20.1591190625158,20.9523221051478,21.9500517292024,22.9477813532571,
23.9455109773117,24.9432406013664,25.9409702254211,26.4423043696954),
 .UNSPECIFIED.);
#2576=B_SPLINE_CURVE_WITH_KNOTS('',3,(#34644,#34645,#34646,#34647,#34648,
#34649,#34650,#34651,#34652,#34653,#34654,#34655,#34656,#34657,#34658,#34659,
#34660,#34661,#34662,#34663,#34664,#34665),.UNSPECIFIED.,.F.,.F.,(4,3,3,
3,3,3,3,4),(-22.7021579259084,-21.9500517292025,-20.9523221051478,-19.9545924810932,
-18.9568628570385,-17.9591332329838,-16.9614036089292,-16.4189726187288),
 .UNSPECIFIED.);
#2577=B_SPLINE_CURVE_WITH_KNOTS('',3,(#34670,#34671,#34672,#34673,#34674,
#34675,#34676,#34677,#34678,#34679,#34680,#34681,#34682,#34683,#34684,#34685,
#34686,#34687,#34688,#34689,#34690,#34691,#34692,#34693,#34694),
 .UNSPECIFIED.,.F.,.F.,(4,3,3,3,3,3,3,3,4),(13.8759337553362,13.9682147367652,
14.9659443608198,15.9636739848745,16.9614036089292,17.9591332329838,18.9568628570385,
19.9545924810931,20.1591190625158),.UNSPECIFIED.);
#2578=B_SPLINE_CURVE_WITH_KNOTS('',3,(#34695,#34696,#34697,#34698,#34699,
#34700,#34701,#34702,#34703,#34704,#34705,#34706,#34707,#34708,#34709,#34710,
#34711,#34712,#34713,#34714,#34715,#34716),.UNSPECIFIED.,.F.,.F.,(4,3,3,
3,3,3,3,4),(-16.4189726187288,-15.9636739848745,-14.9659443608199,-13.9682147367652,
-12.9704851127106,-11.9727554886559,-10.9750258646012,-10.1357873115493),
 .UNSPECIFIED.);
#2579=B_SPLINE_CURVE_WITH_KNOTS('',3,(#34722,#34723,#34724,#34725,#34726,
#34727,#34728,#34729,#34730,#34731,#34732,#34733,#34734),.UNSPECIFIED.,
 .F.,.F.,(4,3,3,3,4),(-3.85260200436966,-2.99318887216398,-1.99545924810932,
-0.997729624054659,0.),.UNSPECIFIED.);
#2580=B_SPLINE_CURVE_WITH_KNOTS('',3,(#34737,#34738,#34739,#34740,#34741,
#34742,#34743,#34744,#34745,#34746,#34747,#34748,#34749,#34750,#34751,#34752,
#34753,#34754,#34755),.UNSPECIFIED.,.F.,.F.,(4,3,3,3,3,3,4),(2.02057249175679,
2.99318887216397,3.99091849621862,4.98864812027328,5.98637774432793,6.98410736838259,
7.59274844815664),.UNSPECIFIED.);
#2581=B_SPLINE_CURVE_WITH_KNOTS('',3,(#34761,#34762,#34763,#34764,#34765,
#34766,#34767,#34768),.UNSPECIFIED.,.F.,.F.,(4,1,1,1,1,4),(72.2566310325653,
72.7168683309134,73.7145979549681,74.7123275790227,75.7100572030774,76.707786827132),
 .UNSPECIFIED.);
#2582=B_SPLINE_CURVE_WITH_KNOTS('',3,(#34771,#34772,#34773,#34774,#34775,
#34776,#34777,#34778,#34779),.UNSPECIFIED.,.F.,.F.,(4,1,1,1,1,1,4),(72.2566310325653,
72.2667183221419,73.2644479461966,74.2621775702512,75.2599071943059,76.2576368183605,
77.2302531987677),.UNSPECIFIED.);
#2583=B_SPLINE_CURVE_WITH_KNOTS('',3,(#34784,#34785,#34786,#34787,#34788,
#34789,#34790,#34791,#34792,#34793),.UNSPECIFIED.,.F.,.F.,(4,1,1,1,1,1,
1,4),(65.9734457253856,66.7304905865854,67.7282202106401,68.7259498346948,
69.7236794587494,70.7214090828041,71.7191387068587,72.2566310325653),
 .UNSPECIFIED.);
#2584=B_SPLINE_CURVE_WITH_KNOTS('',3,(#34794,#34795,#34796,#34797,#34798,
#34799,#34800,#34801,#34802,#34803),.UNSPECIFIED.,.F.,.F.,(4,1,1,1,1,1,
1,4),(65.9734457253856,66.280340577814,67.2780702018686,68.2757998259233,
69.2735294499779,70.2712590740326,71.2689886980872,72.2566310325653),
 .UNSPECIFIED.);
#2585=B_SPLINE_CURVE_WITH_KNOTS('',3,(#34808,#34809,#34810,#34811,#34812,
#34813,#34814,#34815,#34816,#34817,#34818),.UNSPECIFIED.,.F.,.F.,(4,1,1,
1,1,1,1,1,4),(59.690260418206,59.7463832182028,60.7441128422575,61.7418424663121,
62.7395720903668,63.7373017144215,64.7350313384761,65.7327609625308,65.9734457253856),
 .UNSPECIFIED.);
#2586=B_SPLINE_CURVE_WITH_KNOTS('',3,(#34819,#34820,#34821,#34822,#34823,
#34824,#34825,#34826,#34827,#34828),.UNSPECIFIED.,.F.,.F.,(4,1,1,1,1,1,
1,4),(59.690260418206,60.293962833486,61.2916924575407,62.2894220815953,
63.28715170565,64.2848813297046,65.2826109537593,65.9734457253856),
 .UNSPECIFIED.);
#2587=B_SPLINE_CURVE_WITH_KNOTS('',3,(#34833,#34834,#34835,#34836,#34837,
#34838,#34839,#34840,#34841,#34842),.UNSPECIFIED.,.F.,.F.,(4,1,1,1,1,1,
1,4),(53.4070751110265,53.7600054738749,54.7577350979295,55.7554647219842,
56.7531943460389,57.7509239700935,58.7486535941482,59.690260418206),
 .UNSPECIFIED.);
#2588=B_SPLINE_CURVE_WITH_KNOTS('',3,(#34843,#34844,#34845,#34846,#34847,
#34848,#34849,#34850,#34851,#34852),.UNSPECIFIED.,.F.,.F.,(4,1,1,1,1,1,
1,4),(53.4070751110265,54.3075850891581,55.3053147132127,56.3030443372674,
57.3007739613221,58.2985035853767,59.2962332094314,59.690260418206),
 .UNSPECIFIED.);
#2589=B_SPLINE_CURVE_WITH_KNOTS('',3,(#34857,#34858,#34859,#34860,#34861,
#34862,#34863,#34864,#34865,#34866),.UNSPECIFIED.,.F.,.F.,(4,1,1,1,1,1,
1,4),(47.1238898038468,47.7736277295469,48.7713573536016,49.7690869776563,
50.7668166017109,51.7645462257656,52.7622758498202,53.4070751110265),
 .UNSPECIFIED.);
#2590=B_SPLINE_CURVE_WITH_KNOTS('',3,(#34867,#34868,#34869,#34870,#34871,
#34872,#34873,#34874,#34875,#34876,#34877),.UNSPECIFIED.,.F.,.F.,(4,1,1,
1,1,1,1,1,4),(47.1238898038468,47.3234777207755,48.3212073448301,49.3189369688848,
50.3166665929395,51.3143962169941,52.3121258410488,53.3098554651034,53.4070751110265),
 .UNSPECIFIED.);
#2591=B_SPLINE_CURVE_WITH_KNOTS('',3,(#34882,#34883,#34884,#34885,#34886,
#34887,#34888,#34889,#34890,#34891),.UNSPECIFIED.,.F.,.F.,(4,1,1,1,1,1,
1,4),(40.8407044966673,41.787249985219,42.7849796092736,43.7827092333283,
44.780438857383,45.7781684814376,46.7758981054923,47.1238898038468),
 .UNSPECIFIED.);
#2592=B_SPLINE_CURVE_WITH_KNOTS('',3,(#34892,#34893,#34894,#34895,#34896,
#34897,#34898,#34899,#34900,#34901),.UNSPECIFIED.,.F.,.F.,(4,1,1,1,1,1,
1,4),(40.8407044966673,41.3370999764475,42.3348296005022,43.3325592245569,
44.3302888486115,45.3280184726662,46.3257480967208,47.1238898038468),
 .UNSPECIFIED.);
#2593=B_SPLINE_CURVE_WITH_KNOTS('',3,(#34906,#34907,#34908,#34909,#34910,
#34911,#34912,#34913,#34914,#34915,#34916),.UNSPECIFIED.,.F.,.F.,(4,1,1,
1,1,1,1,1,4),(34.5575191894877,34.8031426168364,35.800872240891,36.7986018649457,
37.7963314890004,38.794061113055,39.7917907371097,40.7895203611643,40.8407044966673),
 .UNSPECIFIED.);
#2594=B_SPLINE_CURVE_WITH_KNOTS('',3,(#34917,#34918,#34919,#34920,#34921,
#34922,#34923,#34924,#34925,#34926),.UNSPECIFIED.,.F.,.F.,(4,1,1,1,1,1,
1,4),(34.5575191894877,35.3507222321196,36.3484518561743,37.3461814802289,
38.3439111042836,39.3416407283382,40.3393703523929,40.8407044966673),
 .UNSPECIFIED.);
#2595=B_SPLINE_CURVE_WITH_KNOTS('',3,(#34931,#34932,#34933,#34934,#34935,
#34936,#34937,#34938,#34939,#34940),.UNSPECIFIED.,.F.,.F.,(4,1,1,1,1,1,
1,4),(28.2743338823081,28.8167648725084,29.8144944965631,30.8122241206177,
31.8099537446724,32.8076833687271,33.8054129927817,34.5575191894877),
 .UNSPECIFIED.);
#2596=B_SPLINE_CURVE_WITH_KNOTS('',3,(#34941,#34942,#34943,#34944,#34945,
#34946,#34947,#34948,#34949,#34950,#34951),.UNSPECIFIED.,.F.,.F.,(4,1,1,
1,1,1,1,1,4),(28.2743338823081,28.366614863737,29.3643444877917,30.3620741118463,
31.359803735901,32.3575333599556,33.3552629840103,34.352992608065,34.5575191894877),
 .UNSPECIFIED.);
#2597=B_SPLINE_CURVE_WITH_KNOTS('',3,(#34956,#34957,#34958,#34959,#34960,
#34961,#34962,#34963,#34964,#34965),.UNSPECIFIED.,.F.,.F.,(4,1,1,1,1,1,
1,4),(21.9911485751285,22.8303871281805,23.8281167522351,24.8258463762898,
25.8235760003445,26.8213056243991,27.8190352484538,28.2743338823081),
 .UNSPECIFIED.);
#2598=B_SPLINE_CURVE_WITH_KNOTS('',3,(#34966,#34967,#34968,#34969,#34970,
#34971,#34972,#34973,#34974,#34975),.UNSPECIFIED.,.F.,.F.,(4,1,1,1,1,1,
1,4),(21.9911485751285,22.3802371194091,23.3779667434637,24.3756963675184,
25.3734259915731,26.3711556156277,27.3688852396824,28.2743338823081),
 .UNSPECIFIED.);
#2599=B_SPLINE_CURVE_WITH_KNOTS('',3,(#34981,#34982,#34983,#34984,#34985),
 .UNSPECIFIED.,.F.,.F.,(4,1,4),(14.3984001269718,15.3961297510265,15.7079632679489),
 .UNSPECIFIED.);
#2600=B_SPLINE_CURVE_WITH_KNOTS('',3,(#34988,#34989,#34990,#34991,#34992),
 .UNSPECIFIED.,.F.,.F.,(4,1,4),(13.8759337553361,14.8485501357432,15.7079632679489),
 .UNSPECIFIED.);
#2601=B_SPLINE_CURVE_WITH_KNOTS('',3,(#34994,#34995,#34996,#34997,#34998,
#34999,#35000,#35001,#35002,#35003,#35004,#35005,#35006,#35007,#35008,#35009,
#35010,#35011,#35012,#35013,#35014,#35015,#35016,#35017,#35018,#35019,#35020,
#35021,#35022,#35023,#35024,#35025,#35026,#35027,#35028,#35029,#35030,#35031,
#35032,#35033,#35034,#35035,#35036,#35037,#35038,#35039,#35040,#35041,#35042,
#35043,#35044,#35045),.UNSPECIFIED.,.F.,.F.,(4,3,3,3,3,3,3,3,3,3,3,3,3,
3,3,3,3,4),(-0.286347380332243,-0.266225517657927,-0.253989633145399,-0.224118418951897,
-0.213637228539926,-0.18277997814213,-0.1712802294816,-0.161583702204544,
-0.151922727744335,-0.129977880386141,-0.117970426661857,-0.109303558462843,
-0.0829498108000933,-0.0663205445941391,-0.0521986510922473,-0.0198616494821571,
-0.00388856781184301,0.),.UNSPECIFIED.);
#2602=B_SPLINE_CURVE_WITH_KNOTS('',3,(#35046,#35047,#35048,#35049,#35050,
#35051,#35052,#35053,#35054,#35055,#35056,#35057,#35058,#35059,#35060,#35061,
#35062,#35063,#35064,#35065,#35066,#35067,#35068,#35069,#35070,#35071,#35072,
#35073,#35074,#35075,#35076,#35077,#35078,#35079,#35080,#35081,#35082,#35083,
#35084,#35085,#35086,#35087,#35088,#35089,#35090,#35091,#35092,#35093,#35094,
#35095,#35096,#35097,#35098,#35099,#35100),.UNSPECIFIED.,.F.,.F.,(4,3,3,
3,3,3,3,3,3,3,3,3,3,3,3,3,3,3,4),(-0.285142803995136,-0.264771978453909,
-0.248971203111392,-0.236527824899921,-0.214293390992849,-0.2038268270722,
-0.17295400685889,-0.159192875564253,-0.149652609754856,-0.137562774558619,
-0.11631964633286,-0.104925727456541,-0.0956925453293139,-0.0725695145406395,
-0.0586514835868502,-0.0490375298028169,-0.0212486353032901,-0.00320042217461625,
0.),.UNSPECIFIED.);
#2603=B_SPLINE_CURVE_WITH_KNOTS('',3,(#35102,#35103,#35104,#35105,#35106,
#35107,#35108,#35109,#35110,#35111,#35112),.UNSPECIFIED.,.F.,.F.,(4,1,1,
1,1,1,1,1,4),(15.7079632679489,15.8462797597979,16.8440093838525,17.8417390079072,
18.8394686319618,19.8371982560165,20.8349278800712,21.8326575041258,21.9911485751285),
 .UNSPECIFIED.);
#2604=B_SPLINE_CURVE_WITH_KNOTS('',3,(#35113,#35114,#35115,#35116,#35117,
#35118,#35119,#35120,#35121,#35122),.UNSPECIFIED.,.F.,.F.,(4,1,1,1,1,1,
1,4),(15.7079632679489,16.3938593750811,17.3915889991358,18.3893186231905,
19.3870482472451,20.3847778712998,21.3825074953544,21.9911485751285),
 .UNSPECIFIED.);
#2605=B_SPLINE_CURVE_WITH_KNOTS('',3,(#35395,#35396,#35397,#35398,#35399,
#35400,#35401,#35402,#35403,#35404,#35405,#35406,#35407,#35408,#35409,#35410,
#35411,#35412,#35413,#35414,#35415,#35416,#35417,#35418,#35419,#35420,#35421,
#35422,#35423,#35424,#35425,#35426,#35427,#35428,#35429,#35430,#35431,#35432,
#35433,#35434,#35435,#35436,#35437,#35438,#35439,#35440,#35441,#35442,#35443),
 .UNSPECIFIED.,.F.,.F.,(4,3,3,3,3,3,3,3,3,3,3,3,3,3,3,3,4),(0.,0.0274255371814078,
0.0484189866654049,0.0576777559231281,0.0872193790463039,0.100313119697051,
0.108749799500732,0.134012411342703,0.149997937188314,0.163168454336766,
0.192693763100972,0.210037636696566,0.220559059471184,0.247872294074534,
0.26049857837061,0.281269689393589,0.285142803995142),.UNSPECIFIED.);
#2606=B_SPLINE_CURVE_WITH_KNOTS('',3,(#35444,#35445,#35446,#35447,#35448,
#35449,#35450,#35451,#35452,#35453,#35454,#35455,#35456,#35457,#35458,#35459,
#35460,#35461,#35462,#35463,#35464,#35465,#35466,#35467,#35468),
 .UNSPECIFIED.,.F.,.F.,(4,3,3,3,3,3,3,3,4),(-10.1357873115493,-9.97729624054658,
-8.97956661649192,-7.98183699243727,-6.98410736838261,-5.98637774432795,
-4.98864812027329,-3.99091849621863,-3.85260200436966),.UNSPECIFIED.);
#2607=B_SPLINE_CURVE_WITH_KNOTS('',3,(#35741,#35742,#35743,#35744,#35745,
#35746,#35747,#35748,#35749,#35750,#35751,#35752,#35753,#35754,#35755,#35756,
#35757,#35758,#35759,#35760,#35761,#35762),.UNSPECIFIED.,.F.,.F.,(4,3,3,
3,3,3,3,4),(7.59274844815664,7.98183699243725,8.9795666164919,9.97729624054656,
10.9750258646012,11.9727554886559,12.9704851127105,13.8759337553362),
 .UNSPECIFIED.);
#2608=B_SPLINE_CURVE_WITH_KNOTS('',3,(#35763,#35764,#35765,#35766,#35767,
#35768,#35769,#35770,#35771,#35772,#35773,#35774,#35775,#35776,#35777,#35778,
#35779,#35780,#35781,#35782,#35783,#35784,#35785,#35786,#35787,#35788,#35789,
#35790,#35791,#35792,#35793,#35794,#35795,#35796,#35797,#35798,#35799,#35800,
#35801,#35802,#35803,#35804,#35805,#35806,#35807,#35808,#35809,#35810,#35811),
 .UNSPECIFIED.,.F.,.F.,(4,3,3,3,3,3,3,3,3,3,3,3,3,3,3,3,4),(0.,0.0320358644790656,
0.0566025392350713,0.0661929095230273,0.097524509655756,0.113218578765797,
0.122777613428698,0.148357330195644,0.170686258066526,0.180239221440332,
0.205963417559621,0.220473935588774,0.231002296372473,0.247562418687567,
0.263621625608468,0.283136005917488,0.286347380332233),.UNSPECIFIED.);
#2609=B_SPLINE_CURVE_WITH_KNOTS('',3,(#36326,#36327,#36328,#36329,#36330,
#36331,#36332,#36333,#36334,#36335,#36336,#36337,#36338,#36339,#36340,#36341,
#36342,#36343,#36344,#36345,#36346,#36347,#36348,#36349,#36350,#36351,#36352,
#36353,#36354,#36355,#36356,#36357,#36358,#36359,#36360,#36361,#36362,#36363,
#36364,#36365,#36366),.UNSPECIFIED.,.F.,.F.,(4,1,1,1,1,1,1,1,1,1,1,1,1,
1,1,1,1,1,1,1,1,1,1,1,1,1,1,1,1,1,1,1,1,1,1,1,1,1,4),(0.,0.496040945303652,
0.992081890607303,1.48812283591095,1.98416378121461,2.48020472651826,2.97624567182191,
3.47228661712556,3.96832756242921,4.46436850773286,4.96040945303652,5.45645039834017,
5.95249134364382,6.44853228894747,6.94457323425112,7.44061417955477,7.93665512485842,
8.43269607016208,8.92873701546573,9.42477796076938,9.92081890607303,10.4168598513767,
10.9129007966803,11.408941741984,11.9049826872876,12.4010236325913,12.8970645778949,
13.3931055231986,13.8891464685022,14.3851874138059,14.8812283591095,15.3772693044132,
15.8733102497168,16.3693511950205,16.8653921403242,17.3614330856278,17.8574740309315,
18.3535149762351,18.8495559215388),.UNSPECIFIED.);
#2610=B_SPLINE_CURVE_WITH_KNOTS('',3,(#36376,#36377,#36378,#36379,#36380,
#36381,#36382,#36383,#36384,#36385),.UNSPECIFIED.,.F.,.F.,(4,3,3,4),(-4.09254174883833,
-3.98934337020898,-2.99200752765673,-2.06514013327813),.UNSPECIFIED.);
#2611=B_SPLINE_CURVE_WITH_KNOTS('',3,(#36388,#36389,#36390,#36391,#36392,
#36393,#36394),.UNSPECIFIED.,.F.,.F.,(4,3,4),(0.,0.998006970630082,1.11419103802948),
 .UNSPECIFIED.);
#2612=B_SPLINE_CURVE_WITH_KNOTS('',3,(#36399,#36400,#36401,#36402,#36403,
#36404,#36405,#36406,#36407,#36408,#36409,#36410,#36411,#36412,#36413,#36414,
#36415,#36416,#36417,#36418,#36419,#36420),.UNSPECIFIED.,.F.,.F.,(4,3,3,
3,3,3,3,4),(-10.3757270560179,-9.97335842552244,-8.9760225829702,-7.97868674041795,
-6.9813508978657,-5.98401505531347,-4.98667921276122,-4.09254174883833),
 .UNSPECIFIED.);
#2613=B_SPLINE_CURVE_WITH_KNOTS('',3,(#36421,#36422,#36423,#36424,#36425,
#36426,#36427,#36428,#36429,#36430,#36431,#36432,#36433,#36434,#36435,#36436,
#36437,#36438,#36439,#36440,#36441,#36442),.UNSPECIFIED.,.F.,.F.,(4,3,3,
3,3,3,3,4),(1.11419103802948,1.99601394126018,2.99402091189026,3.99202788252035,
4.99003485315045,5.98804182378054,6.98604879441062,7.39737634520907),
 .UNSPECIFIED.);
#2614=B_SPLINE_CURVE_WITH_KNOTS('',3,(#36447,#36448,#36449,#36450,#36451,
#36452,#36453,#36454,#36455,#36456,#36457,#36458,#36459,#36460,#36461,#36462,
#36463,#36464,#36465,#36466,#36467,#36468),.UNSPECIFIED.,.F.,.F.,(4,3,3,
3,3,3,3,4),(-16.6589123631975,-15.9573734808359,-14.9600376382837,-13.9627017957314,
-12.9653659531792,-11.9680301106269,-10.9706942680747,-10.3757270560179),
 .UNSPECIFIED.);
#2615=B_SPLINE_CURVE_WITH_KNOTS('',3,(#36469,#36470,#36471,#36472,#36473,
#36474,#36475,#36476,#36477,#36478,#36479,#36480,#36481,#36482,#36483,#36484,
#36485,#36486,#36487,#36488,#36489,#36490),.UNSPECIFIED.,.F.,.F.,(4,3,3,
3,3,3,3,4),(7.39737634520907,7.98405576504071,8.9820627356708,9.98006970630089,
10.978076676931,11.9760836475611,12.9740906181912,13.6805616523887),
 .UNSPECIFIED.);
#2616=B_SPLINE_CURVE_WITH_KNOTS('',3,(#36495,#36496,#36497,#36498,#36499,
#36500,#36501,#36502,#36503,#36504,#36505,#36506,#36507,#36508,#36509,#36510,
#36511,#36512,#36513,#36514,#36515,#36516),.UNSPECIFIED.,.F.,.F.,(4,3,3,
3,3,3,3,4),(-22.9420976703771,-21.9413885361494,-20.9440526935971,-19.9467168510449,
-18.9493810084926,-17.9520451659404,-16.9547093233881,-16.6589123631975),
 .UNSPECIFIED.);
#2617=B_SPLINE_CURVE_WITH_KNOTS('',3,(#36517,#36518,#36519,#36520,#36521,
#36522,#36523,#36524,#36525,#36526,#36527,#36528,#36529,#36530,#36531,#36532,
#36533,#36534,#36535,#36536,#36537,#36538),.UNSPECIFIED.,.F.,.F.,(4,3,3,
3,3,3,3,4),(13.6805616523887,13.9720975888212,14.9701045594513,15.9681115300814,
16.9661185007115,17.9641254713416,18.9621324419717,19.9637469595682),
 .UNSPECIFIED.);
#2618=B_SPLINE_CURVE_WITH_KNOTS('',3,(#36543,#36544,#36545,#36546,#36547,
#36548,#36549,#36550,#36551,#36552,#36553,#36554,#36555,#36556,#36557,#36558,
#36559,#36560,#36561,#36562,#36563,#36564),.UNSPECIFIED.,.F.,.F.,(4,3,3,
3,3,3,3,4),(-29.2252829775567,-28.9227394340151,-27.9254035914628,-26.9280677489106,
-25.9307319063583,-24.9333960638061,-23.9360602212539,-22.9420976703771),
 .UNSPECIFIED.);
#2619=B_SPLINE_CURVE_WITH_KNOTS('',3,(#36565,#36566,#36567,#36568,#36569,
#36570,#36571,#36572,#36573,#36574,#36575,#36576,#36577,#36578,#36579,#36580,
#36581,#36582,#36583,#36584,#36585,#36586),.UNSPECIFIED.,.F.,.F.,(4,3,3,
3,3,3,3,4),(19.9637469595682,20.9581463832319,21.956153353862,22.954160324492,
23.9521672951221,24.9501742657522,25.9481812363823,26.2469322667478),
 .UNSPECIFIED.);
#2620=B_SPLINE_CURVE_WITH_KNOTS('',3,(#36591,#36592,#36593,#36594,#36595,
#36596,#36597,#36598,#36599,#36600,#36601,#36602,#36603,#36604,#36605,#36606,
#36607,#36608,#36609,#36610,#36611,#36612),.UNSPECIFIED.,.F.,.F.,(4,3,3,
3,3,3,3,4),(-35.5084682847363,-34.9067544893285,-33.9094186467763,-32.9120828042241,
-31.9147469616718,-30.9174111191196,-29.9200752765673,-29.2252829775567),
 .UNSPECIFIED.);
#2621=B_SPLINE_CURVE_WITH_KNOTS('',3,(#36613,#36614,#36615,#36616,#36617,
#36618,#36619,#36620,#36621,#36622,#36623,#36624,#36625,#36626,#36627,#36628,
#36629,#36630,#36631,#36632,#36633,#36634),.UNSPECIFIED.,.F.,.F.,(4,3,3,
3,3,3,3,4),(26.2469322667478,26.9461882070124,27.9441951776425,28.9422021482726,
29.9402091189027,30.9382160895327,31.9362230601628,32.5301175739274),
 .UNSPECIFIED.);
#2622=B_SPLINE_CURVE_WITH_KNOTS('',3,(#36639,#36640,#36641,#36642,#36643,
#36644,#36645,#36646,#36647,#36648,#36649,#36650,#36651,#36652,#36653,#36654,
#36655,#36656,#36657,#36658,#36659,#36660),.UNSPECIFIED.,.F.,.F.,(4,3,3,
3,3,3,3,4),(-41.7916535919159,-40.890769544642,-39.8934337020898,-38.8960978595375,
-37.8987620169853,-36.901426174433,-35.9040903318808,-35.5084682847363),
 .UNSPECIFIED.);
#2623=B_SPLINE_CURVE_WITH_KNOTS('',3,(#36661,#36662,#36663,#36664,#36665,
#36666,#36667,#36668,#36669,#36670,#36671,#36672,#36673,#36674,#36675,#36676,
#36677,#36678,#36679,#36680,#36681,#36682),.UNSPECIFIED.,.F.,.F.,(4,3,3,
3,3,3,3,4),(32.5301175739274,32.9342300307929,33.932237001423,34.9302439720531,
35.9282509426832,36.9262579133133,37.9242648839434,38.813302881107),
 .UNSPECIFIED.);
#2624=B_SPLINE_CURVE_WITH_KNOTS('',3,(#36687,#36688,#36689,#36690,#36691,
#36692,#36693,#36694,#36695,#36696,#36697,#36698,#36699,#36700,#36701,#36702,
#36703,#36704,#36705,#36706,#36707,#36708,#36709,#36710,#36711),
 .UNSPECIFIED.,.F.,.F.,(4,3,3,3,3,3,3,3,4),(-48.0748388990955,-47.8721204425077,
-46.8747845999555,-45.8774487574032,-44.880112914851,-43.8827770722987,
-42.8854412297465,-41.8881053871943,-41.7916535919159),.UNSPECIFIED.);
#2625=B_SPLINE_CURVE_WITH_KNOTS('',3,(#36712,#36713,#36714,#36715,#36716,
#36717,#36718,#36719,#36720,#36721,#36722,#36723,#36724,#36725,#36726,#36727,
#36728,#36729,#36730,#36731,#36732,#36733,#36734,#36735,#36736),
 .UNSPECIFIED.,.F.,.F.,(4,3,3,3,3,3,3,3,4),(38.813302881107,38.9222718545735,
39.9202788252036,40.9182857958337,41.9162927664637,42.9142997370938,43.9123067077239,
44.910313678354,45.0964881882866),.UNSPECIFIED.);
#2626=B_SPLINE_CURVE_WITH_KNOTS('',3,(#36741,#36742,#36743,#36744,#36745,
#36746,#36747,#36748,#36749,#36750,#36751,#36752,#36753,#36754,#36755,#36756,
#36757,#36758,#36759,#36760,#36761,#36762),.UNSPECIFIED.,.F.,.F.,(4,3,3,
3,3,3,3,4),(-54.3580242062751,-53.8561354978212,-52.8587996552689,-51.8614638127167,
-50.8641279701645,-49.8667921276122,-48.86945628506,-48.0748388990955),
 .UNSPECIFIED.);
#2627=B_SPLINE_CURVE_WITH_KNOTS('',3,(#36763,#36764,#36765,#36766,#36767,
#36768,#36769,#36770,#36771,#36772,#36773,#36774,#36775,#36776,#36777,#36778,
#36779,#36780,#36781,#36782,#36783,#36784),.UNSPECIFIED.,.F.,.F.,(4,3,3,
3,3,3,3,4),(45.0964881882866,45.9083206489841,46.9063276196142,47.9043345902443,
48.9023415608744,49.9003485315045,50.8983555021345,51.3796734954662),
 .UNSPECIFIED.);
#2628=B_SPLINE_CURVE_WITH_KNOTS('',3,(#36789,#36790,#36791,#36792,#36793,
#36794,#36795,#36796,#36797,#36798,#36799,#36800,#36801,#36802,#36803,#36804,
#36805,#36806,#36807,#36808,#36809,#36810),.UNSPECIFIED.,.F.,.F.,(4,3,3,
3,3,3,3,4),(-60.6412095134546,-59.8401505531347,-58.8428147105824,-57.8454788680302,
-56.8481430254779,-55.8508071829257,-54.8534713403734,-54.3580242062751),
 .UNSPECIFIED.);
#2629=B_SPLINE_CURVE_WITH_KNOTS('',3,(#36811,#36812,#36813,#36814,#36815,
#36816,#36817,#36818,#36819,#36820,#36821,#36822,#36823,#36824,#36825,#36826,
#36827,#36828,#36829,#36830,#36831,#36832),.UNSPECIFIED.,.F.,.F.,(4,3,3,
3,3,3,3,4),(51.3796734954662,51.8963624727646,52.8943694433947,53.8923764140248,
54.8903833846549,55.888390355285,56.8863973259151,57.6628588026458),
 .UNSPECIFIED.);
#2630=B_SPLINE_CURVE_WITH_KNOTS('',3,(#36837,#36838,#36839,#36840,#36841,
#36842,#36843,#36844,#36845,#36846,#36847,#36848,#36849,#36850,#36851,#36852,
#36853,#36854,#36855,#36856,#36857,#36858,#36859,#36860,#36861),
 .UNSPECIFIED.,.F.,.F.,(4,3,3,3,3,3,3,3,4),(-66.9243948206342,-66.8215014510004,
-65.8241656084481,-64.8268297658959,-63.8294939233436,-62.8321580807914,
-61.8348222382391,-60.8374863956869,-60.6412095134546),.UNSPECIFIED.);
#2631=B_SPLINE_CURVE_WITH_KNOTS('',3,(#36862,#36863,#36864,#36865,#36866,
#36867,#36868,#36869,#36870,#36871,#36872,#36873,#36874,#36875,#36876,#36877,
#36878,#36879,#36880,#36881,#36882,#36883,#36884,#36885,#36886),
 .UNSPECIFIED.,.F.,.F.,(4,3,3,3,3,3,3,3,4),(57.6628588026458,57.8844042965452,
58.8824112671752,59.8804182378054,60.8784252084354,61.8764321790655,62.8744391496956,
63.8724461203257,63.9460441098254),.UNSPECIFIED.);
#2632=B_SPLINE_CURVE_WITH_KNOTS('',3,(#36891,#36892,#36893,#36894,#36895,
#36896,#36897,#36898,#36899,#36900,#36901,#36902,#36903,#36904,#36905,#36906,
#36907,#36908,#36909,#36910,#36911,#36912),.UNSPECIFIED.,.F.,.F.,(4,3,3,
3,3,3,3,4),(-73.2075801278138,-72.8055165063138,-71.8081806637616,-70.8108448212093,
-69.8135089786571,-68.8161731361048,-67.8188372935526,-66.9243948206342),
 .UNSPECIFIED.);
#2633=B_SPLINE_CURVE_WITH_KNOTS('',3,(#36913,#36914,#36915,#36916,#36917,
#36918,#36919,#36920,#36921,#36922,#36923,#36924,#36925,#36926,#36927,#36928,
#36929,#36930,#36931,#36932,#36933,#36934),.UNSPECIFIED.,.F.,.F.,(4,3,3,
3,3,3,3,4),(63.9460441098254,64.8704530909558,65.8684600615859,66.866467032216,
67.8644740028461,68.8624809734761,69.8604879441062,70.229229417005),
 .UNSPECIFIED.);
#2634=B_SPLINE_CURVE_WITH_KNOTS('',3,(#36939,#36940,#36941,#36942,#36943,
#36944,#36945,#36946,#36947,#36948,#36949,#36950,#36951,#36952,#36953,#36954,
#36955,#36956,#36957,#36958,#36959,#36960),.UNSPECIFIED.,.F.,.F.,(4,3,3,
3,3,3,3,4),(-79.4907654349934,-78.7895315616273,-77.792195719075,-76.7948598765228,
-75.7975240339705,-74.8001881914183,-73.802852348866,-73.2075801278138),
 .UNSPECIFIED.);
#2635=B_SPLINE_CURVE_WITH_KNOTS('',3,(#36961,#36962,#36963,#36964,#36965,
#36966,#36967,#36968,#36969,#36970,#36971,#36972,#36973,#36974,#36975,#36976,
#36977,#36978,#36979,#36980,#36981,#36982),.UNSPECIFIED.,.F.,.F.,(4,3,3,
3,3,3,3,4),(70.229229417005,70.8584949147363,71.8565018853664,72.8545088559965,
73.8525158266266,74.8505227972567,75.8485297678868,76.5124147241846),
 .UNSPECIFIED.);
#2636=B_SPLINE_CURVE_WITH_KNOTS('',3,(#36987,#36988,#36989,#36990,#36991,
#36992,#36993,#36994,#36995,#36996,#36997,#36998,#36999,#37000,#37001,#37002,
#37003,#37004,#37005,#37006,#37007,#37008),.UNSPECIFIED.,.F.,.F.,(4,3,3,
3,3,3,3,4),(-85.773950742173,-84.7735466169407,-83.7762107743885,-82.7788749318363,
-81.781539089284,-80.7842032467318,-79.7868674041795,-79.4907654349934),
 .UNSPECIFIED.);
#2637=B_SPLINE_CURVE_WITH_KNOTS('',3,(#37009,#37010,#37011,#37012,#37013,
#37014,#37015,#37016,#37017,#37018,#37019,#37020,#37021,#37022,#37023,#37024,
#37025,#37026,#37027,#37028,#37029,#37030),.UNSPECIFIED.,.F.,.F.,(4,3,3,
3,3,3,3,4),(76.5124147241846,76.8465367385169,77.8445437091469,78.842550679777,
79.8405576504071,80.8385646210372,81.8365715916673,82.7956000313642),
 .UNSPECIFIED.);
#2638=B_SPLINE_CURVE_WITH_KNOTS('',3,(#37035,#37036,#37037,#37038,#37039,
#37040,#37041,#37042,#37043,#37044,#37045,#37046,#37047,#37048,#37049,#37050,
#37051,#37052,#37053,#37054,#37055,#37056),.UNSPECIFIED.,.F.,.F.,(4,3,3,
3,3,3,3,4),(-92.0571360493526,-91.7548975148065,-90.7575616722542,-89.760225829702,
-88.7628899871497,-87.7655541445975,-86.7682183020452,-85.773950742173),
 .UNSPECIFIED.);
#2639=B_SPLINE_CURVE_WITH_KNOTS('',3,(#37057,#37058,#37059,#37060,#37061,
#37062,#37063,#37064,#37065,#37066,#37067,#37068,#37069,#37070,#37071,#37072,
#37073,#37074,#37075,#37076,#37077,#37078,#37079,#37080,#37081),
 .UNSPECIFIED.,.F.,.F.,(4,3,3,3,3,3,3,3,4),(82.7956000313642,82.8345785622974,
83.8325855329275,84.8305925035576,85.8285994741877,86.8266064448178,87.8246134154479,
88.822620386078,89.0787853385438),.UNSPECIFIED.);
#2640=B_SPLINE_CURVE_WITH_KNOTS('',3,(#37086,#37087,#37088,#37089,#37090,
#37091,#37092,#37093,#37094,#37095,#37096,#37097,#37098,#37099,#37100,#37101,
#37102,#37103,#37104,#37105,#37106,#37107),.UNSPECIFIED.,.F.,.F.,(4,3,3,
3,3,3,3,4),(-98.3403213565322,-97.7389125701199,-96.7415767275677,-95.7442408850154,
-94.7469050424632,-93.7495691999109,-92.7522333573587,-92.0571360493526),
 .UNSPECIFIED.);
#2641=B_SPLINE_CURVE_WITH_KNOTS('',3,(#37108,#37109,#37110,#37111,#37112,
#37113,#37114,#37115,#37116,#37117,#37118,#37119,#37120,#37121,#37122,#37123,
#37124,#37125,#37126,#37127,#37128,#37129),.UNSPECIFIED.,.F.,.F.,(4,3,3,
3,3,3,3,4),(89.0787853385438,89.820627356708,90.8186343273381,91.8166412979682,
92.8146482685983,93.8126552392284,94.8106622098585,95.3619706457233),
 .UNSPECIFIED.);
#2642=B_SPLINE_CURVE_WITH_KNOTS('',3,(#37135,#37136,#37137,#37138,#37139,
#37140,#37141,#37142),.UNSPECIFIED.,.F.,.F.,(4,1,1,1,1,4),(109.955742875643,
110.351669931783,111.349005774335,112.346341616887,113.343677459439,114.341013301992),
 .UNSPECIFIED.);
#2643=B_SPLINE_CURVE_WITH_KNOTS('',3,(#37145,#37146,#37147,#37148,#37149,
#37150,#37151),.UNSPECIFIED.,.F.,.F.,(4,1,1,1,4),(109.955742875643,110.107297927009,
111.105304897639,112.103311868269,113.101318838899),.UNSPECIFIED.);
#2644=B_SPLINE_CURVE_WITH_KNOTS('',3,(#37156,#37157,#37158,#37159,#37160,
#37161,#37162,#37163,#37164,#37165),.UNSPECIFIED.,.F.,.F.,(4,1,1,1,1,1,
1,4),(103.672557568463,104.367654876469,105.364990719021,106.362326561574,
107.359662404126,108.356998246678,109.35433408923,109.955742875643),
 .UNSPECIFIED.);
#2645=B_SPLINE_CURVE_WITH_KNOTS('',3,(#37166,#37167,#37168,#37169,#37170,
#37171,#37172,#37173,#37174,#37175),.UNSPECIFIED.,.F.,.F.,(4,1,1,1,1,1,
1,4),(103.672557568463,104.119256103228,105.117263073858,106.115270044488,
107.113277015118,108.111283985749,109.109290956379,109.955742875643),
 .UNSPECIFIED.);
#2646=B_SPLINE_CURVE_WITH_KNOTS('',3,(#37180,#37181,#37182,#37183,#37184,
#37185,#37186,#37187,#37188,#37189),.UNSPECIFIED.,.F.,.F.,(4,1,1,1,1,1,
1,4),(97.3893722612836,98.3836398211558,99.380975663708,100.37831150626,
101.375647348812,102.372983191365,103.370319033917,103.672557568463),
 .UNSPECIFIED.);
#2647=B_SPLINE_CURVE_WITH_KNOTS('',3,(#37190,#37191,#37192,#37193,#37194,
#37195,#37196,#37197,#37198,#37199),.UNSPECIFIED.,.F.,.F.,(4,1,1,1,1,1,
1,4),(97.3893722612836,98.1312142794477,99.1292212500778,100.127228220708,
101.125235191338,102.123242161968,103.121249132598,103.672557568463),
 .UNSPECIFIED.);
#2648=B_SPLINE_CURVE_WITH_KNOTS('',3,(#37204,#37205,#37206,#37207,#37208,
#37209,#37210,#37211,#37212,#37213,#37214),.UNSPECIFIED.,.F.,.F.,(4,1,1,
1,1,1,1,1,4),(91.106186954104,91.4022889232901,92.3996247658423,93.3969606083945,
94.3942964509468,95.391632293499,96.3889681360513,97.3863039786035,97.3893722612836),
 .UNSPECIFIED.);
#2649=B_SPLINE_CURVE_WITH_KNOTS('',3,(#37215,#37216,#37217,#37218,#37219,
#37220,#37221,#37222,#37223,#37224,#37225),.UNSPECIFIED.,.F.,.F.,(4,1,1,
1,1,1,1,1,4),(91.106186954104,91.1451654850371,92.1431724556672,93.1411794262973,
94.1391863969273,95.1371933675574,96.1352003381875,97.1332073088176,97.3893722612836),
 .UNSPECIFIED.);
#2650=B_SPLINE_CURVE_WITH_KNOTS('',3,(#37230,#37231,#37232,#37233,#37234,
#37235,#37236,#37237,#37238,#37239),.UNSPECIFIED.,.F.,.F.,(4,1,1,1,1,1,
1,4),(84.8230016469244,85.4182738679766,86.4156097105288,87.4129455530811,
88.4102813956333,89.4076172381856,90.4049530807378,91.106186954104),
 .UNSPECIFIED.);
#2651=B_SPLINE_CURVE_WITH_KNOTS('',3,(#37240,#37241,#37242,#37243,#37244,
#37245,#37246,#37247,#37248,#37249),.UNSPECIFIED.,.F.,.F.,(4,1,1,1,1,1,
1,4),(84.8230016469244,85.1571236612565,86.1551306318866,87.1531376025167,
88.1511445731468,89.1491515437769,90.147158514407,91.106186954104),
 .UNSPECIFIED.);
#2652=B_SPLINE_CURVE_WITH_KNOTS('',3,(#37254,#37255,#37256,#37257,#37258,
#37259,#37260,#37261,#37262,#37263),.UNSPECIFIED.,.F.,.F.,(4,1,1,1,1,1,
1,4),(78.5398163397448,79.4342588126631,80.4315946552154,81.4289304977676,
82.4262663403199,83.4236021828721,84.4209380254243,84.8230016469244),
 .UNSPECIFIED.);
#2653=B_SPLINE_CURVE_WITH_KNOTS('',3,(#37264,#37265,#37266,#37267,#37268,
#37269,#37270,#37271,#37272,#37273),.UNSPECIFIED.,.F.,.F.,(4,1,1,1,1,1,
1,4),(78.5398163397448,79.169081837476,80.1670888081061,81.1650957787362,
82.1631027493663,83.1611097199964,84.1591166906264,84.8230016469244),
 .UNSPECIFIED.);
#2654=B_SPLINE_CURVE_WITH_KNOTS('',3,(#37278,#37279,#37280,#37281,#37282,
#37283,#37284,#37285,#37286,#37287,#37288),.UNSPECIFIED.,.F.,.F.,(4,1,1,
1,1,1,1,1,4),(72.2566310325652,72.4529079147974,73.4502437573497,74.4475795999019,
75.4449154424541,76.4422512850064,77.4395871275586,78.4369229701109,78.5398163397448),
 .UNSPECIFIED.);
#2655=B_SPLINE_CURVE_WITH_KNOTS('',3,(#37289,#37290,#37291,#37292,#37293,
#37294,#37295,#37296,#37297,#37298),.UNSPECIFIED.,.F.,.F.,(4,1,1,1,1,1,
1,4),(72.2566310325652,73.1810400136955,74.1790469843256,75.1770539549557,
76.1750609255857,77.1730678962158,78.1710748668459,78.5398163397448),
 .UNSPECIFIED.);
#2656=B_SPLINE_CURVE_WITH_KNOTS('',3,(#37303,#37304,#37305,#37306,#37307,
#37308,#37309,#37310,#37311,#37312),.UNSPECIFIED.,.F.,.F.,(4,1,1,1,1,1,
1,4),(65.9734457253856,66.468892859484,67.4662287020362,68.4635645445884,
69.4609003871407,70.4582362296929,71.4555720722452,72.2566310325652),
 .UNSPECIFIED.);
#2657=B_SPLINE_CURVE_WITH_KNOTS('',3,(#37313,#37314,#37315,#37316,#37317,
#37318,#37319,#37320,#37321,#37322,#37323),.UNSPECIFIED.,.F.,.F.,(4,1,1,
1,1,1,1,1,4),(65.9734457253856,66.1949912192848,67.1929981899149,68.191005160545,
69.1890121311751,70.1870191018052,71.1850260724353,72.1830330430654,72.2566310325652),
 .UNSPECIFIED.);
#2658=B_SPLINE_CURVE_WITH_KNOTS('',3,(#37328,#37329,#37330,#37331,#37332,
#37333,#37334,#37335,#37336,#37337),.UNSPECIFIED.,.F.,.F.,(4,1,1,1,1,1,
1,4),(59.690260418206,60.4848778041705,61.4822136467227,62.479549489275,
63.4768853318272,64.4742211743795,65.4715570169317,65.9734457253856),
 .UNSPECIFIED.);
#2659=B_SPLINE_CURVE_WITH_KNOTS('',3,(#37338,#37339,#37340,#37341,#37342,
#37343,#37344,#37345,#37346,#37347),.UNSPECIFIED.,.F.,.F.,(4,1,1,1,1,1,
1,4),(59.690260418206,60.2069493955043,61.2049563661344,62.2029633367645,
63.2009703073946,64.1989772780247,65.1969842486548,65.9734457253856),
 .UNSPECIFIED.);
#2660=B_SPLINE_CURVE_WITH_KNOTS('',3,(#37352,#37353,#37354,#37355,#37356,
#37357,#37358,#37359,#37360,#37361,#37362),.UNSPECIFIED.,.F.,.F.,(4,1,1,
1,1,1,1,1,4),(53.4070751110265,53.5035269063048,54.500862748857,55.4981985914093,
56.4955344339615,57.4928702765138,58.490206119066,59.4875419616182,59.690260418206),
 .UNSPECIFIED.);
#2661=B_SPLINE_CURVE_WITH_KNOTS('',3,(#37363,#37364,#37365,#37366,#37367,
#37368,#37369,#37370,#37371,#37372),.UNSPECIFIED.,.F.,.F.,(4,1,1,1,1,1,
1,4),(53.4070751110264,54.2189075717238,55.2169145423539,56.214921512984,
57.212928483614,58.2109354542441,59.2089424248742,59.690260418206),
 .UNSPECIFIED.);
#2662=B_SPLINE_CURVE_WITH_KNOTS('',3,(#37377,#37378,#37379,#37380,#37381,
#37382,#37383,#37384,#37385,#37386),.UNSPECIFIED.,.F.,.F.,(4,1,1,1,1,1,
1,4),(47.1238898038469,47.5195118509913,48.5168476935436,49.5141835360958,
50.5115193786481,51.5088552212003,52.5061910637525,53.4070751110265),
 .UNSPECIFIED.);
#2663=B_SPLINE_CURVE_WITH_KNOTS('',3,(#37387,#37388,#37389,#37390,#37391,
#37392,#37393,#37394,#37395,#37396,#37397),.UNSPECIFIED.,.F.,.F.,(4,1,1,
1,1,1,1,1,4),(47.1238898038468,47.2328587773132,48.2308657479432,49.2288727185733,
50.2268796892034,51.2248866598335,52.2228936304636,53.2209006010937,53.4070751110264),
 .UNSPECIFIED.);
#2664=B_SPLINE_CURVE_WITH_KNOTS('',3,(#37402,#37403,#37404,#37405,#37406,
#37407,#37408,#37409,#37410,#37411),.UNSPECIFIED.,.F.,.F.,(4,1,1,1,1,1,
1,4),(40.8407044966673,41.5354967956779,42.5328326382301,43.5301684807823,
44.5275043233346,45.5248401658868,46.5221760084391,47.1238898038469),
 .UNSPECIFIED.);
#2665=B_SPLINE_CURVE_WITH_KNOTS('',3,(#37412,#37413,#37414,#37415,#37416,
#37417,#37418,#37419,#37420,#37421),.UNSPECIFIED.,.F.,.F.,(4,1,1,1,1,1,
1,4),(40.8407044966672,41.2448169535326,42.2428239241627,43.2408308947928,
44.2388378654229,45.236844836053,46.2348518066831,47.1238898038468),
 .UNSPECIFIED.);
#2666=B_SPLINE_CURVE_WITH_KNOTS('',3,(#37426,#37427,#37428,#37429,#37430,
#37431,#37432,#37433,#37434,#37435),.UNSPECIFIED.,.F.,.F.,(4,1,1,1,1,1,
1,4),(34.5575191894877,35.5514817403644,36.5488175829166,37.5461534254689,
38.5434892680211,39.5408251105734,40.5381609531256,40.8407044966673),
 .UNSPECIFIED.);
#2667=B_SPLINE_CURVE_WITH_KNOTS('',3,(#37436,#37437,#37438,#37439,#37440,
#37441,#37442,#37443,#37444,#37445),.UNSPECIFIED.,.F.,.F.,(4,1,1,1,1,1,
1,4),(34.5575191894876,35.2567751297521,36.2547821003822,37.2527890710123,
38.2507960416424,39.2488030122724,40.2468099829025,40.8407044966672),
 .UNSPECIFIED.);
#2668=B_SPLINE_CURVE_WITH_KNOTS('',3,(#37450,#37451,#37452,#37453,#37454,
#37455,#37456,#37457,#37458,#37459,#37460),.UNSPECIFIED.,.F.,.F.,(4,1,1,
1,1,1,1,1,4),(28.2743338823081,28.5701308424987,29.5674666850509,30.5648025276032,
31.5621383701554,32.5594742127077,33.5568100552599,34.5541458978121,34.5575191894877),
 .UNSPECIFIED.);
#2669=B_SPLINE_CURVE_WITH_KNOTS('',3,(#37461,#37462,#37463,#37464,#37465,
#37466,#37467,#37468,#37469,#37470),.UNSPECIFIED.,.F.,.F.,(4,1,1,1,1,1,
1,4),(28.274333882308,29.2687333059716,30.2667402766016,31.2647472472317,
32.2627542178618,33.2607611884919,34.258768159122,34.5575191894876),
 .UNSPECIFIED.);
#2670=B_SPLINE_CURVE_WITH_KNOTS('',3,(#37475,#37476,#37477,#37478,#37479,
#37480,#37481,#37482,#37483,#37484),.UNSPECIFIED.,.F.,.F.,(4,1,1,1,1,1,
1,4),(21.9911485751285,22.5861157871852,23.5834516297375,24.5807874722897,
25.5781233148419,26.5754591573942,27.5727949999464,28.2743338823081),
 .UNSPECIFIED.);
#2671=B_SPLINE_CURVE_WITH_KNOTS('',3,(#37485,#37486,#37487,#37488,#37489,
#37490,#37491,#37492,#37493,#37494,#37495),.UNSPECIFIED.,.F.,.F.,(4,1,1,
1,1,1,1,1,4),(21.9911485751285,22.2826845115609,23.280691482191,24.2786984528211,
25.2767054234512,26.2747123940813,27.2727193647114,28.2707263353415,28.274333882308),
 .UNSPECIFIED.);
#2672=B_SPLINE_CURVE_WITH_KNOTS('',3,(#37500,#37501,#37502,#37503,#37504,
#37505,#37506,#37507,#37508,#37509),.UNSPECIFIED.,.F.,.F.,(4,1,1,1,1,1,
1,4),(15.7079632679489,16.6021007318718,17.599436574424,18.5967724169762,
19.5941082595285,20.5914441020807,21.588779944633,21.9911485751285),
 .UNSPECIFIED.);
#2673=B_SPLINE_CURVE_WITH_KNOTS('',3,(#37510,#37511,#37512,#37513,#37514,
#37515,#37516,#37517,#37518,#37519),.UNSPECIFIED.,.F.,.F.,(4,1,1,1,1,1,
1,4),(15.7079632679489,16.2946426877804,17.2926496584105,18.2906566290406,
19.2886635996707,20.2866705703008,21.2846775409308,21.9911485751285),
 .UNSPECIFIED.);
#2674=B_SPLINE_CURVE_WITH_KNOTS('',3,(#37522,#37523,#37524,#37525,#37526,
#37527,#37528,#37529,#37530,#37531,#37532,#37533,#37534,#37535,#37536,#37537,
#37538,#37539,#37540,#37541,#37542,#37543,#37544,#37545,#37546,#37547,#37548,
#37549,#37550,#37551,#37552,#37553,#37554,#37555,#37556,#37557,#37558,#37559,
#37560,#37561,#37562,#37563,#37564,#37565,#37566,#37567,#37568,#37569,#37570,
#37571,#37572,#37573,#37574,#37575,#37576,#37577,#37578,#37579,#37580,#37581,
#37582,#37583,#37584,#37585,#37586,#37587,#37588,#37589,#37590,#37591,#37592,
#37593,#37594,#37595,#37596,#37597,#37598,#37599,#37600),.UNSPECIFIED.,
 .F.,.F.,(4,3,3,3,3,3,3,3,3,3,3,3,3,3,3,3,3,3,3,3,3,3,3,3,3,3,4),(-0.996917990983956,
-0.964197655296454,-0.951513094737375,-0.939590005196496,-0.910398139253692,
-0.896458168447615,-0.866624051431682,-0.848513043381918,-0.839276821658768,
-0.836789934415749,-0.803176729602168,-0.780362864215826,-0.769651322799483,
-0.734439153414668,-0.711686399207869,-0.700944767019061,-0.669566542377212,
-0.648981044332524,-0.637888877288902,-0.602287825523676,-0.584615028650125,
-0.570052223933311,-0.532768447080654,-0.516116381189141,-0.50154558318824,
-0.495484670227998,-0.468408511919796),.UNSPECIFIED.);
#2675=B_SPLINE_CURVE_WITH_KNOTS('',3,(#37602,#37603,#37604,#37605,#37606,
#37607,#37608,#37609,#37610,#37611,#37612,#37613,#37614,#37615,#37616,#37617,
#37618,#37619,#37620,#37621,#37622,#37623,#37624,#37625,#37626,#37627,#37628,
#37629,#37630,#37631,#37632,#37633,#37634,#37635),.UNSPECIFIED.,.F.,.F.,
(4,3,3,3,3,3,3,3,3,3,3,4),(-0.271362855059921,-0.23333358174471,-0.202109628804149,
-0.191194824123734,-0.172574372312687,-0.139871461148431,-0.130049418747569,
-0.0948265930323134,-0.0669749700089491,-0.0565955729248257,-0.0239539643597006,
0.),.UNSPECIFIED.);
#2676=B_SPLINE_CURVE_WITH_KNOTS('',3,(#37638,#37639,#37640,#37641,#37642,
#37643,#37644,#37645,#37646,#37647,#37648,#37649,#37650,#37651,#37652,#37653,
#37654,#37655,#37656,#37657,#37658,#37659,#37660,#37661,#37662,#37663,#37664,
#37665,#37666,#37667,#37668,#37669,#37670,#37671,#37672,#37673,#37674,#37675,
#37676,#37677,#37678,#37679,#37680,#37681,#37682,#37683,#37684,#37685,#37686,
#37687,#37688,#37689,#37690,#37691,#37692,#37693,#37694,#37695,#37696,#37697,
#37698,#37699,#37700,#37701),.UNSPECIFIED.,.F.,.F.,(4,3,3,3,3,3,3,3,3,3,
3,3,3,3,3,3,3,3,3,3,3,4),(-0.468408511919796,-0.44532089356327,-0.431869826400524,
-0.394574417707956,-0.377959024336246,-0.36718387876206,-0.329707820210052,
-0.314417154781481,-0.297766482794163,-0.286364248592707,-0.248901620010442,
-0.233074500624702,-0.216543640108336,-0.17799293612575,-0.152182016671258,
-0.141011423916894,-0.12652726456846,-0.094895448426345,-0.0796457512037788,
-0.0683009962329189,-0.0289678476755453,0.),.UNSPECIFIED.);
#2677=B_SPLINE_CURVE_WITH_KNOTS('',3,(#38130,#38131,#38132,#38133,#38134,
#38135,#38136,#38137),.UNSPECIFIED.,.F.,.F.,(4,1,1,1,1,4),(11.6154215191105,
12.6127573616628,13.610093204215,14.6074290467673,15.6047648893195,15.7079632679489),
 .UNSPECIFIED.);
#2678=B_SPLINE_CURVE_WITH_KNOTS('',3,(#38138,#38139,#38140,#38141,#38142,
#38143,#38144,#38145,#38146,#38147,#38148,#38149,#38150,#38151,#38152,#38153,
#38154,#38155,#38156,#38157,#38158,#38159,#38160,#38161,#38162,#38163,#38164,
#38165,#38166,#38167,#38168,#38169,#38170,#38171,#38172,#38173,#38174,#38175,
#38176,#38177,#38178,#38179,#38180,#38181,#38182,#38183,#38184,#38185,#38186,
#38187,#38188,#38189,#38190,#38191,#38192,#38193,#38194,#38195),
 .UNSPECIFIED.,.F.,.F.,(4,3,3,3,3,3,3,3,3,3,3,3,3,3,3,3,3,3,3,4),(-0.364629307890661,
-0.350885759085945,-0.324346713718219,-0.304152838893849,-0.282934787914253,
-0.264003466919189,-0.252764227803326,-0.216347623970161,-0.198031500011342,
-0.186602740018901,-0.166173598315468,-0.146000730648533,-0.128382123165429,
-0.119003916100956,-0.0892529370757172,-0.0724905256163614,-0.0619084956994276,
-0.0517443199161659,-0.0194955210690912,0.),.UNSPECIFIED.);
#2679=B_SPLINE_CURVE_WITH_KNOTS('',3,(#38196,#38197,#38198,#38199,#38200,
#38201,#38202,#38203,#38204,#38205,#38206,#38207,#38208),.UNSPECIFIED.,
 .F.,.F.,(4,3,3,3,4),(-101.213804280572,-100.730920097777,-99.7335842552244,
-98.7362484126722,-98.3403213565322),.UNSPECIFIED.);
#2680=B_SPLINE_CURVE_WITH_KNOTS('',3,(#38211,#38212,#38213,#38214,#38215,
#38216,#38217,#38218,#38219),.UNSPECIFIED.,.F.,.F.,(4,1,1,1,1,1,4),(10.3757270560178,
11.30460783463,12.30261480526,13.3006217758901,14.2986287465202,15.2966357171503,
15.7079632679489),.UNSPECIFIED.);
#2681=B_SPLINE_CURVE_WITH_KNOTS('',3,(#38653,#38654,#38655,#38656,#38657,
#38658,#38659,#38660,#38661,#38662,#38663,#38664,#38665,#38666,#38667,#38668),
 .UNSPECIFIED.,.F.,.F.,(4,3,3,3,3,4),(95.3619706457233,95.8086691804886,
96.8066761511186,97.8046831217487,98.8026900923788,99.1486641472938),
 .UNSPECIFIED.);
#2682=B_SPLINE_CURVE_WITH_KNOTS('',3,(#38669,#38670,#38671,#38672,#38673,
#38674,#38675,#38676,#38677,#38678,#38679,#38680,#38681,#38682,#38683,#38684,
#38685,#38686,#38687,#38688,#38689,#38690,#38691,#38692,#38693,#38694,#38695,
#38696,#38697,#38698,#38699,#38700,#38701,#38702,#38703,#38704,#38705,#38706,
#38707,#38708,#38709,#38710,#38711,#38712,#38713,#38714,#38715,#38716,#38717,
#38718,#38719,#38720),.UNSPECIFIED.,.F.,.F.,(4,3,3,3,3,3,3,3,3,3,3,3,3,
3,3,3,3,4),(-0.366397579005845,-0.355461226466819,-0.328804438442731,-0.31606471842091,
-0.292558951597566,-0.280250898914551,-0.245275213061006,-0.218626183485931,
-0.207947804736759,-0.187209422476688,-0.163808244667102,-0.149577787474042,
-0.13876424622794,-0.104073184670955,-0.0827908372522071,-0.0667764467402658,
-0.0282827470320728,0.),.UNSPECIFIED.);
#2683=B_SPLINE_CURVE_WITH_KNOTS('',3,(#38774,#38775,#38776,#38777,#38778,
#38779,#38780,#38781,#38782,#38783),.UNSPECIFIED.,.F.,.F.,(4,3,3,4),(-4.09202352044854,
-3.99291737327004,-2.99468802995253,-2.07317267331973),.UNSPECIFIED.);
#2684=B_SPLINE_CURVE_WITH_KNOTS('',3,(#38786,#38787,#38788,#38789,#38790,
#38791,#38792),.UNSPECIFIED.,.F.,.F.,(4,3,4),(0.,0.999341140225982,1.12274180646093),
 .UNSPECIFIED.);
#2685=B_SPLINE_CURVE_WITH_KNOTS('',3,(#38797,#38798,#38799,#38800,#38801,
#38802,#38803,#38804,#38805,#38806,#38807,#38808,#38809,#38810,#38811,#38812,
#38813,#38814,#38815,#38816,#38817,#38818),.UNSPECIFIED.,.F.,.F.,(4,3,3,
3,3,3,3,4),(-10.3752088276281,-9.9822934331751,-8.98406408985759,-7.98583474654008,
-6.98760540322257,-5.98937605990506,-4.99114671658755,-4.09202352044854),
 .UNSPECIFIED.);
#2686=B_SPLINE_CURVE_WITH_KNOTS('',3,(#38819,#38820,#38821,#38822,#38823,
#38824,#38825,#38826,#38827,#38828,#38829,#38830,#38831,#38832,#38833,#38834,
#38835,#38836,#38837,#38838,#38839,#38840),.UNSPECIFIED.,.F.,.F.,(4,3,3,
3,3,3,3,4),(1.12274180646093,1.99868228045197,2.99802342067795,3.99736456090394,
4.99670570112992,5.99604684135591,6.99538798158189,7.40592711364052),
 .UNSPECIFIED.);
#2687=B_SPLINE_CURVE_WITH_KNOTS('',3,(#38845,#38846,#38847,#38848,#38849,
#38850,#38851,#38852,#38853,#38854,#38855,#38856,#38857,#38858,#38859,#38860,
#38861,#38862,#38863,#38864,#38865,#38866),.UNSPECIFIED.,.F.,.F.,(4,3,3,
3,3,3,3,4),(-16.6583941348077,-15.9716694930802,-14.9734401497627,-13.9752108064451,
-12.9769814631276,-11.9787521198101,-10.9805227764926,-10.3752088276281),
 .UNSPECIFIED.);
#2688=B_SPLINE_CURVE_WITH_KNOTS('',3,(#38867,#38868,#38869,#38870,#38871,
#38872,#38873,#38874,#38875,#38876,#38877,#38878,#38879,#38880,#38881,#38882,
#38883,#38884,#38885,#38886,#38887,#38888),.UNSPECIFIED.,.F.,.F.,(4,3,3,
3,3,3,3,4),(7.40592711364052,7.99472912180787,8.99407026203386,9.99341140225984,
10.9927525424858,11.9920936827118,12.9914348229378,13.6891124208201),
 .UNSPECIFIED.);
#2689=B_SPLINE_CURVE_WITH_KNOTS('',3,(#38893,#38894,#38895,#38896,#38897,
#38898,#38899,#38900,#38901,#38902,#38903,#38904,#38905,#38906,#38907,#38908,
#38909,#38910,#38911,#38912,#38913,#38914),.UNSPECIFIED.,.F.,.F.,(4,3,3,
3,3,3,3,4),(-22.9415794419873,-21.9610455529852,-20.9628162096677,-19.9645868663502,
-18.9663575230327,-17.9681281797152,-16.9698988363977,-16.6583941348077),
 .UNSPECIFIED.);
#2690=B_SPLINE_CURVE_WITH_KNOTS('',3,(#38915,#38916,#38917,#38918,#38919,
#38920,#38921,#38922,#38923,#38924,#38925,#38926,#38927,#38928,#38929,#38930,
#38931,#38932,#38933,#38934,#38935,#38936),.UNSPECIFIED.,.F.,.F.,(4,3,3,
3,3,3,3,4),(13.6891124208201,13.9907759631638,14.9901171033898,15.9894582436157,
16.9887993838417,17.9881405240677,18.9874816642937,19.9722977279997),
 .UNSPECIFIED.);
#2691=B_SPLINE_CURVE_WITH_KNOTS('',3,(#38941,#38942,#38943,#38944,#38945,
#38946,#38947,#38948,#38949,#38950,#38951,#38952,#38953,#38954,#38955,#38956,
#38957,#38958,#38959,#38960,#38961,#38962,#38963,#38964,#38965),
 .UNSPECIFIED.,.F.,.F.,(4,3,3,3,3,3,3,3,4),(-29.2247647491669,-28.9486509562078,
-27.9504216128903,-26.9521922695728,-25.9539629262553,-24.9557335829378,
-23.9575042396202,-22.9592748963027,-22.9415794419873),.UNSPECIFIED.);
#2692=B_SPLINE_CURVE_WITH_KNOTS('',3,(#38966,#38967,#38968,#38969,#38970,
#38971,#38972,#38973,#38974,#38975,#38976,#38977,#38978,#38979,#38980,#38981,
#38982,#38983,#38984,#38985,#38986,#38987,#38988,#38989,#38990),
 .UNSPECIFIED.,.F.,.F.,(4,3,3,3,3,3,3,3,4),(19.9722977279997,19.9868228045197,
20.9861639447457,21.9855050849716,22.9848462251976,23.9841873654236,24.9835285056496,
25.9828696458756,26.2554830351793),.UNSPECIFIED.);
#2693=B_SPLINE_CURVE_WITH_KNOTS('',3,(#38995,#38996,#38997,#38998,#38999,
#39000,#39001,#39002,#39003,#39004,#39005,#39006,#39007,#39008,#39009,#39010,
#39011,#39012,#39013,#39014,#39015,#39016),.UNSPECIFIED.,.F.,.F.,(4,3,3,
3,3,3,3,4),(-35.5079500563465,-34.9380270161129,-33.9397976727954,-32.9415683294778,
-31.9433389861603,-30.9451096428428,-29.9468802995253,-29.2247647491669),
 .UNSPECIFIED.);
#2694=B_SPLINE_CURVE_WITH_KNOTS('',3,(#39017,#39018,#39019,#39020,#39021,
#39022,#39023,#39024,#39025,#39026,#39027,#39028,#39029,#39030,#39031,#39032,
#39033,#39034,#39035,#39036,#39037,#39038),.UNSPECIFIED.,.F.,.F.,(4,3,3,
3,3,3,3,4),(26.2554830351793,26.9822107861016,27.9815519263275,28.9808930665535,
29.9802342067795,30.9795753470055,31.9789164872315,32.5386683423589),
 .UNSPECIFIED.);
#2695=B_SPLINE_CURVE_WITH_KNOTS('',3,(#39043,#39044,#39045,#39046,#39047,
#39048,#39049,#39050,#39051,#39052,#39053,#39054,#39055,#39056,#39057,#39058,
#39059,#39060,#39061,#39062,#39063,#39064),.UNSPECIFIED.,.F.,.F.,(4,3,3,
3,3,3,3,4),(-41.7911353635261,-40.9274030760179,-39.9291737327004,-38.9309443893829,
-37.9327150460654,-36.9344857027479,-35.9362563594304,-35.5079500563465),
 .UNSPECIFIED.);
#2696=B_SPLINE_CURVE_WITH_KNOTS('',3,(#39065,#39066,#39067,#39068,#39069,
#39070,#39071,#39072,#39073,#39074,#39075,#39076,#39077,#39078,#39079,#39080,
#39081,#39082,#39083,#39084,#39085,#39086),.UNSPECIFIED.,.F.,.F.,(4,3,3,
3,3,3,3,4),(32.5386683423589,32.9782576274575,33.9775987676834,34.9769399079094,
35.9762810481354,36.9756221883614,37.9749633285874,38.8218536495385),
 .UNSPECIFIED.);
#2697=B_SPLINE_CURVE_WITH_KNOTS('',3,(#39091,#39092,#39093,#39094,#39095,
#39096,#39097,#39098,#39099,#39100,#39101,#39102,#39103,#39104,#39105,#39106,
#39107,#39108,#39109,#39110,#39111,#39112,#39113,#39114,#39115),
 .UNSPECIFIED.,.F.,.F.,(4,3,3,3,3,3,3,3,4),(-48.0743206707057,-47.9150084792405,
-46.916779135923,-45.9185497926055,-44.920320449288,-43.9220911059705,-42.9238617626529,
-41.9256324193354,-41.7911353635261),.UNSPECIFIED.);
#2698=B_SPLINE_CURVE_WITH_KNOTS('',3,(#39116,#39117,#39118,#39119,#39120,
#39121,#39122,#39123,#39124,#39125,#39126,#39127,#39128,#39129,#39130,#39131,
#39132,#39133,#39134,#39135,#39136,#39137,#39138,#39139,#39140),
 .UNSPECIFIED.,.F.,.F.,(4,3,3,3,3,3,3,3,4),(38.8218536495385,38.9743044688134,
39.9736456090394,40.9729867492653,41.9723278894913,42.9716690297173,43.9710101699433,
44.9703513101693,45.105038956718),.UNSPECIFIED.);
#2699=B_SPLINE_CURVE_WITH_KNOTS('',3,(#39145,#39146,#39147,#39148,#39149,
#39150,#39151,#39152,#39153,#39154,#39155,#39156,#39157,#39158,#39159,#39160,
#39161,#39162,#39163,#39164,#39165,#39166),.UNSPECIFIED.,.F.,.F.,(4,3,3,
3,3,3,3,4),(-54.3575059778853,-53.9043845391456,-52.906155195828,-51.9079258525105,
-50.909696509193,-49.9114671658755,-48.913237822558,-48.0743206707057),
 .UNSPECIFIED.);
#2700=B_SPLINE_CURVE_WITH_KNOTS('',3,(#39167,#39168,#39169,#39170,#39171,
#39172,#39173,#39174,#39175,#39176,#39177,#39178,#39179,#39180,#39181,#39182,
#39183,#39184,#39185,#39186,#39187,#39188),.UNSPECIFIED.,.F.,.F.,(4,3,3,
3,3,3,3,4),(45.105038956718,45.9696924503953,46.9690335906212,47.9683747308472,
48.9677158710732,49.9670570112992,50.9663981515252,51.3882242638976),
 .UNSPECIFIED.);
#2701=B_SPLINE_CURVE_WITH_KNOTS('',3,(#39193,#39194,#39195,#39196,#39197,
#39198,#39199,#39200,#39201,#39202,#39203,#39204,#39205,#39206,#39207,#39208,
#39209,#39210,#39211,#39212,#39213,#39214),.UNSPECIFIED.,.F.,.F.,(4,3,3,
3,3,3,3,4),(-60.6406912850648,-59.8937605990506,-58.8955312557331,-57.8973019124156,
-56.8990725690981,-55.9008432257806,-54.9026138824631,-54.3575059778853),
 .UNSPECIFIED.);
#2702=B_SPLINE_CURVE_WITH_KNOTS('',3,(#39215,#39216,#39217,#39218,#39219,
#39220,#39221,#39222,#39223,#39224,#39225,#39226,#39227,#39228,#39229,#39230,
#39231,#39232,#39233,#39234,#39235,#39236),.UNSPECIFIED.,.F.,.F.,(4,3,3,
3,3,3,3,4),(51.3882242638976,51.9657392917511,52.9650804319771,53.9644215722031,
54.9637627124291,55.9631038526551,56.9624449928811,57.6714095710772),
 .UNSPECIFIED.);
#2703=B_SPLINE_CURVE_WITH_KNOTS('',3,(#39242,#39243,#39244,#39245,#39246,
#39247,#39248,#39249,#39250,#39251),.UNSPECIFIED.,.F.,.F.,(4,1,1,1,1,1,
1,4),(72.2566310325653,72.5079296898685,73.506159033186,74.5043883765035,
75.502617719821,76.5008470631385,77.499076406456,78.4973057497735),
 .UNSPECIFIED.);
#2704=B_SPLINE_CURVE_WITH_KNOTS('',3,(#39254,#39255,#39256,#39257,#39258,
#39259,#39260,#39261,#39262),.UNSPECIFIED.,.F.,.F.,(4,1,1,1,1,1,4),(72.2566310325652,
72.2598691287713,73.2592102689973,74.2585514092233,75.2578925494492,76.2572336896752,
77.2565748299012),.UNSPECIFIED.);
#2705=B_SPLINE_CURVE_WITH_KNOTS('',3,(#39267,#39268,#39269,#39270,#39271,
#39272,#39273,#39274,#39275,#39276),.UNSPECIFIED.,.F.,.F.,(4,1,1,1,1,1,
1,4),(65.9734457253856,66.5185536299634,67.5167829732809,68.5150123165984,
69.513241659916,70.5114710032335,71.509700346551,72.2566310325653),
 .UNSPECIFIED.);
#2706=B_SPLINE_CURVE_WITH_KNOTS('',3,(#39277,#39278,#39279,#39280,#39281,
#39282,#39283,#39284,#39285,#39286),.UNSPECIFIED.,.F.,.F.,(4,1,1,1,1,1,
1,4),(65.9734457253856,66.2638222874154,67.2631634276414,68.2625045678674,
69.2618457080933,70.2611868483193,71.2605279885453,72.2566310325652),
 .UNSPECIFIED.);
#2707=B_SPLINE_CURVE_WITH_KNOTS('',3,(#39291,#39292,#39293,#39294,#39295,
#39296,#39297,#39298,#39299,#39300),.UNSPECIFIED.,.F.,.F.,(4,1,1,1,1,1,
1,4),(59.6902604182061,60.5291775700584,61.5274069133759,62.5256362566934,
63.5238656000109,64.5220949433284,65.5203242866459,65.9734457253856),
 .UNSPECIFIED.);
#2708=B_SPLINE_CURVE_WITH_KNOTS('',3,(#39301,#39302,#39303,#39304,#39305,
#39306,#39307,#39308,#39309,#39310),.UNSPECIFIED.,.F.,.F.,(4,1,1,1,1,1,
1,4),(59.6902604182061,60.2677754460595,61.2671165862855,62.2664577265115,
63.2657988667374,64.2651400069634,65.2644811471894,65.9734457253856),
 .UNSPECIFIED.);
#2709=B_SPLINE_CURVE_WITH_KNOTS('',3,(#39315,#39316,#39317,#39318,#39319,
#39320,#39321,#39322,#39323,#39324,#39325),.UNSPECIFIED.,.F.,.F.,(4,1,1,
1,1,1,1,1,4),(53.4070751110265,53.5415721668358,54.5398015101533,55.5380308534708,
56.5362601967883,57.5344895401058,58.5327188834233,59.5309482267409,59.6902604182061),
 .UNSPECIFIED.);
#2710=B_SPLINE_CURVE_WITH_KNOTS('',3,(#39326,#39327,#39328,#39329,#39330,
#39331,#39332,#39333,#39334,#39335),.UNSPECIFIED.,.F.,.F.,(4,1,1,1,1,1,
1,4),(53.4070751110265,54.2717286047036,55.2710697449296,56.2704108851556,
57.2697520253815,58.2690931656075,59.2684343058335,59.6902604182061),
 .UNSPECIFIED.);
#2711=B_SPLINE_CURVE_WITH_KNOTS('',3,(#39340,#39341,#39342,#39343,#39344,
#39345,#39346,#39347,#39348,#39349),.UNSPECIFIED.,.F.,.F.,(4,1,1,1,1,1,
1,4),(47.1238898038469,47.5521961069307,48.5504254502482,49.5486547935658,
50.5468841368833,51.5451134802008,52.5433428235183,53.4070751110265),
 .UNSPECIFIED.);
#2712=B_SPLINE_CURVE_WITH_KNOTS('',3,(#39350,#39351,#39352,#39353,#39354,
#39355,#39356,#39357,#39358,#39359,#39360),.UNSPECIFIED.,.F.,.F.,(4,1,1,
1,1,1,1,1,4),(47.1238898038469,47.2763406231217,48.2756817633477,49.2750229035737,
50.2743640437997,51.2737051840256,52.2730463242516,53.2723874644776,53.4070751110265),
 .UNSPECIFIED.);
#2713=B_SPLINE_CURVE_WITH_KNOTS('',3,(#39365,#39366,#39367,#39368,#39369,
#39370,#39371,#39372,#39373,#39374),.UNSPECIFIED.,.F.,.F.,(4,1,1,1,1,1,
1,4),(40.8407044966673,41.5628200470257,42.5610493903432,43.5592787336607,
44.5575080769782,45.5557374202957,46.5539667636132,47.1238898038469),
 .UNSPECIFIED.);
#2714=B_SPLINE_CURVE_WITH_KNOTS('',3,(#39375,#39376,#39377,#39378,#39379,
#39380,#39381,#39382,#39383,#39384),.UNSPECIFIED.,.F.,.F.,(4,1,1,1,1,1,
1,4),(40.8407044966673,41.2802937817658,42.2796349219918,43.2789760622178,
44.2783172024438,45.2776583426697,46.2769994828957,47.1238898038469),
 .UNSPECIFIED.);
#2715=B_SPLINE_CURVE_WITH_KNOTS('',3,(#39389,#39390,#39391,#39392,#39393,
#39394,#39395,#39396,#39397,#39398,#39399),.UNSPECIFIED.,.F.,.F.,(4,1,1,
1,1,1,1,1,4),(34.5575191894877,34.5752146438031,35.5734439871206,36.5716733304381,
37.5699026737556,38.5681320170731,39.5663613603907,40.5645907037082,40.8407044966673),
 .UNSPECIFIED.);
#2716=B_SPLINE_CURVE_WITH_KNOTS('',3,(#39400,#39401,#39402,#39403,#39404,
#39405,#39406,#39407,#39408,#39409),.UNSPECIFIED.,.F.,.F.,(4,1,1,1,1,1,
1,4),(34.5575191894877,35.2842469404099,36.2835880806359,37.2829292208619,
38.2822703610879,39.2816115013138,40.2809526415398,40.8407044966673),
 .UNSPECIFIED.);
#2717=B_SPLINE_CURVE_WITH_KNOTS('',3,(#39414,#39415,#39416,#39417,#39418,
#39419,#39420,#39421,#39422,#39423),.UNSPECIFIED.,.F.,.F.,(4,1,1,1,1,1,
1,4),(28.2743338823081,28.585838583898,29.5840679272155,30.5822972705331,
31.5805266138506,32.5787559571681,33.5769853004856,34.5575191894877),
 .UNSPECIFIED.);
#2718=B_SPLINE_CURVE_WITH_KNOTS('',3,(#39424,#39425,#39426,#39427,#39428,
#39429,#39430,#39431,#39432,#39433,#39434),.UNSPECIFIED.,.F.,.F.,(4,1,1,
1,1,1,1,1,4),(28.2743338823081,28.288858958828,29.288200099054,30.28754123928,
31.286882379506,32.2862235197319,33.2855646599579,34.2849058001839,34.5575191894877),
 .UNSPECIFIED.);
#2719=B_SPLINE_CURVE_WITH_KNOTS('',3,(#39439,#39440,#39441,#39442,#39443,
#39444,#39445,#39446,#39447,#39448),.UNSPECIFIED.,.F.,.F.,(4,1,1,1,1,1,
1,4),(21.9911485751285,22.596462523993,23.5946918673105,24.592921210628,
25.5911505539455,26.589379897263,27.5876092405805,28.2743338823081),
 .UNSPECIFIED.);
#2720=B_SPLINE_CURVE_WITH_KNOTS('',3,(#39449,#39450,#39451,#39452,#39453,
#39454,#39455,#39456,#39457,#39458),.UNSPECIFIED.,.F.,.F.,(4,1,1,1,1,1,
1,4),(21.9911485751285,22.2928121174721,23.2921532576981,24.2914943979241,
25.2908355381501,26.290176678376,27.289517818602,28.2743338823081),
 .UNSPECIFIED.);
#2721=B_SPLINE_CURVE_WITH_KNOTS('',3,(#39463,#39464,#39465,#39466,#39467,
#39468,#39469,#39470,#39471,#39472),.UNSPECIFIED.,.F.,.F.,(4,1,1,1,1,1,
1,4),(15.7079632679489,16.6070864640879,17.6053158074054,18.6035451507229,
19.6017744940404,20.600003837358,21.5982331806755,21.9911485751285),
 .UNSPECIFIED.);
#2722=B_SPLINE_CURVE_WITH_KNOTS('',3,(#39473,#39474,#39475,#39476,#39477,
#39478,#39479,#39480,#39481,#39482),.UNSPECIFIED.,.F.,.F.,(4,1,1,1,1,1,
1,4),(15.7079632679489,16.2967652761162,17.2961064163422,18.2954475565682,
19.2947886967942,20.2941298370201,21.2934709772461,21.9911485751285),
 .UNSPECIFIED.);
#2723=B_SPLINE_CURVE_WITH_KNOTS('',3,(#39485,#39486,#39487,#39488,#39489,
#39490,#39491,#39492,#39493,#39494,#39495,#39496,#39497,#39498,#39499,#39500,
#39501,#39502,#39503,#39504,#39505,#39506,#39507,#39508,#39509,#39510,#39511,
#39512,#39513,#39514,#39515,#39516,#39517,#39518,#39519,#39520,#39521,#39522,
#39523,#39524,#39525,#39526,#39527,#39528,#39529,#39530,#39531,#39532,#39533,
#39534,#39535,#39536,#39537,#39538,#39539,#39540,#39541,#39542,#39543,#39544,
#39545,#39546,#39547,#39548,#39549,#39550,#39551,#39552,#39553,#39554,#39555,
#39556,#39557,#39558,#39559,#39560,#39561,#39562,#39563,#39564,#39565,#39566,
#39567,#39568,#39569,#39570,#39571,#39572,#39573,#39574,#39575,#39576,#39577,
#39578,#39579,#39580,#39581,#39582,#39583,#39584,#39585,#39586,#39587,#39588,
#39589,#39590,#39591,#39592,#39593,#39594,#39595,#39596,#39597,#39598,#39599,
#39600,#39601,#39602,#39603,#39604,#39605,#39606,#39607,#39608),
 .UNSPECIFIED.,.F.,.F.,(4,3,3,3,3,3,3,3,3,3,3,3,3,3,3,3,3,3,3,3,3,3,3,3,
3,3,3,3,3,3,3,3,3,3,3,3,3,3,3,3,3,4),(-0.753008129282183,-0.726412785409006,
-0.715916399573649,-0.694852053413067,-0.683242780289961,-0.673766450589417,
-0.652778815266657,-0.639500919906121,-0.631791179943898,-0.604637195598433,
-0.591408327349303,-0.58243092328052,-0.553935160168246,-0.540392555827386,
-0.528208940192808,-0.505508318677634,-0.491429191967348,-0.477982436820105,
-0.452062180399923,-0.438863938010204,-0.427153921531904,-0.400727666335641,
-0.382198730280871,-0.374301411139377,-0.345303428221882,-0.331998698266984,
-0.322788462765202,-0.292662279142726,-0.279737557595205,-0.270213961274558,
-0.2400599353808,-0.238094602813322,-0.224912522130576,-0.21640841250359,
-0.186556730675161,-0.170795284707343,-0.161336087437576,-0.129168886313724,
-0.116523493465494,-0.106577361616136,-0.097001685189873,-0.096536015547866),
 .UNSPECIFIED.);
#2724=B_SPLINE_CURVE_WITH_KNOTS('',3,(#39610,#39611,#39612,#39613,#39614,
#39615,#39616,#39617,#39618,#39619,#39620,#39621,#39622,#39623,#39624,#39625,
#39626,#39627,#39628,#39629,#39630,#39631,#39632,#39633,#39634,#39635,#39636,
#39637,#39638,#39639,#39640,#39641,#39642,#39643,#39644,#39645,#39646),
 .UNSPECIFIED.,.F.,.F.,(4,3,3,3,3,3,3,3,3,3,3,3,4),(-0.204609524178328,
-0.17392271218969,-0.152224313672341,-0.142809800777549,-0.129914959151416,
-0.113620867578377,-0.100585910230378,-0.0924114342381335,-0.0693085756786001,
-0.0545304238088379,-0.0417479715798885,-0.0152833907299223,0.),
 .UNSPECIFIED.);
#2725=B_SPLINE_CURVE_WITH_KNOTS('',3,(#39649,#39650,#39651,#39652,#39653,
#39654,#39655,#39656,#39657,#39658,#39659,#39660,#39661,#39662,#39663,#39664),
 .UNSPECIFIED.,.F.,.F.,(4,3,3,3,3,4),(-0.096536015547866,-0.0724020116608995,
-0.0590251911255789,-0.0503900123732228,-0.0186970194324831,0.),
 .UNSPECIFIED.);
#2726=B_SPLINE_CURVE_WITH_KNOTS('',3,(#39949,#39950,#39951,#39952,#39953,
#39954,#39955,#39956),.UNSPECIFIED.,.F.,.F.,(4,1,1,1,1,4),(11.6159397475004,
12.6141690908179,13.6123984341354,14.6106277774529,15.6088571207704,15.7079632679489),
 .UNSPECIFIED.);
#2727=B_SPLINE_CURVE_WITH_KNOTS('',3,(#39957,#39958,#39959,#39960,#39961,
#39962,#39963,#39964,#39965,#39966,#39967,#39968,#39969,#39970,#39971,#39972,
#39973,#39974,#39975,#39976,#39977,#39978,#39979,#39980,#39981,#39982,#39983,
#39984,#39985,#39986,#39987,#39988,#39989,#39990,#39991,#39992,#39993,#39994,
#39995,#39996,#39997,#39998,#39999,#40000,#40001,#40002,#40003,#40004,#40005),
 .UNSPECIFIED.,.F.,.F.,(4,3,3,3,3,3,3,3,3,3,3,3,3,3,3,3,4),(-0.275362278356883,
-0.264159546247523,-0.242523917618953,-0.228489201611509,-0.209076761803474,
-0.198077656999141,-0.168436231356347,-0.151777330299101,-0.139830254922987,
-0.12544363295055,-0.101855794992709,-0.0891849033129337,-0.0668886774847003,
-0.0515641266869526,-0.0405229119346731,-0.0142790183076863,0.),
 .UNSPECIFIED.);
#2728=B_SPLINE_CURVE_WITH_KNOTS('',3,(#40006,#40007,#40008,#40009,#40010,
#40011,#40012,#40013,#40014,#40015,#40016,#40017,#40018,#40019,#40020,#40021,
#40022,#40023,#40024),.UNSPECIFIED.,.F.,.F.,(4,3,3,3,3,3,4),(-65.3636982725397,
-64.8849073156381,-63.8866779723206,-62.8884486290032,-61.8902192856856,
-60.8919899423681,-60.6406912850648),.UNSPECIFIED.);
#2729=B_SPLINE_CURVE_WITH_KNOTS('',3,(#40027,#40028,#40029,#40030,#40031,
#40032,#40033,#40034,#40035),.UNSPECIFIED.,.F.,.F.,(4,1,1,1,1,1,4),(10.375208827628,
11.3000595749863,12.2994007152123,13.2987418554383,14.2980829956642,15.2974241358902,
15.7079632679489),.UNSPECIFIED.);
#2730=B_SPLINE_CURVE_WITH_KNOTS('',3,(#40325,#40326,#40327,#40328,#40329,
#40330,#40331,#40332,#40333,#40334,#40335,#40336,#40337,#40338,#40339,#40340,
#40341,#40342,#40343,#40344,#40345,#40346),.UNSPECIFIED.,.F.,.F.,(4,3,3,
3,3,3,3,4),(57.6714095710772,57.9617861331071,58.961127273333,59.960468413559,
60.959809553785,61.959150694011,62.958491834237,63.29052559922),
 .UNSPECIFIED.);
#2731=B_SPLINE_CURVE_WITH_KNOTS('',3,(#40347,#40348,#40349,#40350,#40351,
#40352,#40353,#40354,#40355,#40356,#40357,#40358,#40359,#40360,#40361,#40362,
#40363,#40364,#40365,#40366,#40367,#40368,#40369,#40370,#40371,#40372,#40373,
#40374,#40375,#40376,#40377,#40378,#40379,#40380,#40381,#40382,#40383,#40384,
#40385,#40386,#40387,#40388,#40389,#40390,#40391,#40392,#40393,#40394,#40395,
#40396,#40397,#40398),.UNSPECIFIED.,.F.,.F.,(4,3,3,3,3,3,3,3,3,3,3,3,3,
3,3,3,3,4),(-0.276631791712725,-0.267716618892456,-0.246046101828633,-0.235289362386452,
-0.214941892616146,-0.204749662554743,-0.176256346031651,-0.161806307413905,
-0.15286753466007,-0.140652476775023,-0.120886137603943,-0.110226811379351,
-0.100669960776508,-0.0755024705823808,-0.058604244392821,-0.0491682800449266,
-0.0181536719473738,0.),.UNSPECIFIED.);
#2732=B_SPLINE_CURVE_WITH_KNOTS('',3,(#40452,#40453,#40454,#40455,#40456,
#40457,#40458,#40459,#40460,#40461),.UNSPECIFIED.,.F.,.F.,(4,3,3,4),(-4.09202352044855,
-3.97107960880372,-2.97830970660279,-2.07317267331974),.UNSPECIFIED.);
#2733=B_SPLINE_CURVE_WITH_KNOTS('',3,(#40464,#40465,#40466,#40467,#40468,
#40469,#40470),.UNSPECIFIED.,.F.,.F.,(4,3,4),(0.,0.993500176108578,1.12274180646087),
 .UNSPECIFIED.);
#2734=B_SPLINE_CURVE_WITH_KNOTS('',3,(#40475,#40476,#40477,#40478,#40479,
#40480,#40481,#40482,#40483,#40484,#40485,#40486,#40487,#40488,#40489,#40490,
#40491,#40492,#40493,#40494,#40495,#40496),.UNSPECIFIED.,.F.,.F.,(4,3,3,
3,3,3,3,4),(-10.3752088276281,-9.92769902200931,-8.93492911980838,-7.94215921760745,
-6.94938931540652,-5.95661941320559,-4.96384951100465,-4.09202352044855),
 .UNSPECIFIED.);
#2735=B_SPLINE_CURVE_WITH_KNOTS('',3,(#40497,#40498,#40499,#40500,#40501,
#40502,#40503,#40504,#40505,#40506,#40507,#40508,#40509,#40510,#40511,#40512,
#40513,#40514,#40515,#40516,#40517,#40518),.UNSPECIFIED.,.F.,.F.,(4,3,3,
3,3,3,3,4),(1.12274180646087,1.98700035221716,2.98050052832574,3.97400070443431,
4.96750088054289,5.96100105665147,6.95450123276005,7.40592711364046),
 .UNSPECIFIED.);
#2736=B_SPLINE_CURVE_WITH_KNOTS('',3,(#40523,#40524,#40525,#40526,#40527,
#40528,#40529,#40530,#40531,#40532,#40533,#40534,#40535,#40536,#40537,#40538,
#40539,#40540,#40541,#40542,#40543,#40544),.UNSPECIFIED.,.F.,.F.,(4,3,3,
3,3,3,3,4),(-16.6583941348077,-15.8843184352149,-14.891548533014,-13.898778630813,
-12.9060087286121,-11.9132388264112,-10.9204689242102,-10.3752088276281),
 .UNSPECIFIED.);
#2737=B_SPLINE_CURVE_WITH_KNOTS('',3,(#40545,#40546,#40547,#40548,#40549,
#40550,#40551,#40552,#40553,#40554,#40555,#40556,#40557,#40558,#40559,#40560,
#40561,#40562,#40563,#40564,#40565,#40566),.UNSPECIFIED.,.F.,.F.,(4,3,3,
3,3,3,3,4),(7.40592711364046,7.94800140886863,8.94150158497721,9.93500176108579,
10.9285019371944,11.922002113303,12.9155022894115,13.68911242082),
 .UNSPECIFIED.);
#2738=B_SPLINE_CURVE_WITH_KNOTS('',3,(#40571,#40572,#40573,#40574,#40575,
#40576,#40577,#40578,#40579,#40580,#40581,#40582,#40583,#40584,#40585,#40586,
#40587,#40588,#40589,#40590,#40591,#40592,#40593,#40594,#40595),
 .UNSPECIFIED.,.F.,.F.,(4,3,3,3,3,3,3,3,4),(-22.9415794419873,-22.8337077506214,
-21.8409378484205,-20.8481679462195,-19.8553980440186,-18.8626281418177,
-17.8698582396168,-16.8770883374158,-16.6583941348077),.UNSPECIFIED.);
#2739=B_SPLINE_CURVE_WITH_KNOTS('',3,(#40596,#40597,#40598,#40599,#40600,
#40601,#40602,#40603,#40604,#40605,#40606,#40607,#40608,#40609,#40610,#40611,
#40612,#40613,#40614,#40615,#40616,#40617,#40618,#40619,#40620),
 .UNSPECIFIED.,.F.,.F.,(4,3,3,3,3,3,3,3,4),(13.68911242082,13.9090024655201,
14.9025026416287,15.8960028177373,16.8895029938458,17.8830031699544,18.876503346063,
19.8700035221716,19.9722977279996),.UNSPECIFIED.);
#2740=B_SPLINE_CURVE_WITH_KNOTS('',3,(#40625,#40626,#40627,#40628,#40629,
#40630,#40631,#40632,#40633,#40634,#40635,#40636,#40637,#40638,#40639,#40640,
#40641,#40642,#40643,#40644,#40645,#40646),.UNSPECIFIED.,.F.,.F.,(4,3,3,
3,3,3,3,4),(-29.2247647491669,-28.790327163827,-27.7975572616261,-26.8047873594251,
-25.8120174572242,-24.8192475550233,-23.8264776528223,-22.9415794419873),
 .UNSPECIFIED.);
#2741=B_SPLINE_CURVE_WITH_KNOTS('',3,(#40647,#40648,#40649,#40650,#40651,
#40652,#40653,#40654,#40655,#40656,#40657,#40658,#40659,#40660,#40661,#40662,
#40663,#40664,#40665,#40666,#40667,#40668),.UNSPECIFIED.,.F.,.F.,(4,3,3,
3,3,3,3,4),(19.9722977279996,20.8635036982802,21.8570038743887,22.8505040504973,
23.8440042266059,24.8375044027145,25.8310045788231,26.2554830351792),
 .UNSPECIFIED.);
#2742=B_SPLINE_CURVE_WITH_KNOTS('',3,(#40673,#40674,#40675,#40676,#40677,
#40678,#40679,#40680,#40681,#40682,#40683,#40684,#40685,#40686,#40687,#40688,
#40689,#40690,#40691,#40692,#40693,#40694),.UNSPECIFIED.,.F.,.F.,(4,3,3,
3,3,3,3,4),(-35.5079500563465,-34.7469465770326,-33.7541766748316,-32.7614067726307,
-31.7686368704298,-30.7758669682288,-29.7830970660279,-29.2247647491669),
 .UNSPECIFIED.);
#2743=B_SPLINE_CURVE_WITH_KNOTS('',3,(#40695,#40696,#40697,#40698,#40699,
#40700,#40701,#40702,#40703,#40704,#40705,#40706,#40707,#40708,#40709,#40710,
#40711,#40712,#40713,#40714,#40715,#40716),.UNSPECIFIED.,.F.,.F.,(4,3,3,
3,3,3,3,4),(26.2554830351792,26.8245047549316,27.8180049310402,28.8115051071488,
29.8050052832574,30.798505459366,31.7920056354745,32.5386683423588),
 .UNSPECIFIED.);
#2744=B_SPLINE_CURVE_WITH_KNOTS('',3,(#40721,#40722,#40723,#40724,#40725,
#40726,#40727,#40728,#40729,#40730,#40731,#40732,#40733,#40734,#40735,#40736,
#40737,#40738,#40739,#40740,#40741,#40742,#40743,#40744,#40745),
 .UNSPECIFIED.,.F.,.F.,(4,3,3,3,3,3,3,3,4),(-41.7911353635261,-41.6963358924391,
-40.7035659902382,-39.7107960880372,-38.7180261858363,-37.7252562836354,
-36.7324863814344,-35.7397164792335,-35.5079500563465),.UNSPECIFIED.);
#2745=B_SPLINE_CURVE_WITH_KNOTS('',3,(#40746,#40747,#40748,#40749,#40750,
#40751,#40752,#40753,#40754,#40755,#40756,#40757,#40758,#40759,#40760,#40761,
#40762,#40763,#40764,#40765,#40766,#40767,#40768,#40769,#40770),
 .UNSPECIFIED.,.F.,.F.,(4,3,3,3,3,3,3,3,4),(32.5386683423588,32.7855058115831,
33.7790059876917,34.7725061638003,35.7660063399088,36.7595065160174,37.753006692126,
38.7465068682346,38.8218536495384),.UNSPECIFIED.);
#2746=B_SPLINE_CURVE_WITH_KNOTS('',3,(#40775,#40776,#40777,#40778,#40779,
#40780,#40781,#40782,#40783,#40784,#40785,#40786,#40787,#40788,#40789,#40790,
#40791,#40792,#40793,#40794,#40795,#40796),.UNSPECIFIED.,.F.,.F.,(4,3,3,
3,3,3,3,4),(-48.0743206707057,-47.6529553056447,-46.6601854034437,-45.6674155012428,
-44.6746455990419,-43.6818756968409,-42.68910579464,-41.7911353635261),
 .UNSPECIFIED.);
#2747=B_SPLINE_CURVE_WITH_KNOTS('',3,(#40797,#40798,#40799,#40800,#40801,
#40802,#40803,#40804,#40805,#40806,#40807,#40808,#40809,#40810,#40811,#40812,
#40813,#40814,#40815,#40816,#40817,#40818),.UNSPECIFIED.,.F.,.F.,(4,3,3,
3,3,3,3,4),(38.8218536495384,39.7400070443432,40.7335072204517,41.7270073965603,
42.7205075726689,43.7140077487775,44.7075079248861,45.105038956718),
 .UNSPECIFIED.);
#2748=B_SPLINE_CURVE_WITH_KNOTS('',3,(#40823,#40824,#40825,#40826,#40827,
#40828,#40829,#40830,#40831,#40832,#40833,#40834,#40835,#40836,#40837,#40838,
#40839,#40840,#40841,#40842,#40843,#40844),.UNSPECIFIED.,.F.,.F.,(4,3,3,
3,3,3,3,4),(-54.3575059778853,-53.6095747188503,-52.6168048166493,-51.6240349144484,
-50.6312650122475,-49.6384951100465,-48.6457252078456,-48.0743206707057),
 .UNSPECIFIED.);
#2749=B_SPLINE_CURVE_WITH_KNOTS('',3,(#40845,#40846,#40847,#40848,#40849,
#40850,#40851,#40852,#40853,#40854,#40855,#40856,#40857,#40858,#40859,#40860,
#40861,#40862,#40863,#40864,#40865,#40866),.UNSPECIFIED.,.F.,.F.,(4,3,3,
3,3,3,3,4),(45.105038956718,45.7010081009946,46.6945082771032,47.6880084532118,
48.6815086293204,49.675008805429,50.6685089815375,51.3882242638976),
 .UNSPECIFIED.);
#2750=B_SPLINE_CURVE_WITH_KNOTS('',3,(#40871,#40872,#40873,#40874,#40875,
#40876,#40877,#40878,#40879,#40880,#40881,#40882,#40883,#40884,#40885,#40886,
#40887,#40888,#40889,#40890,#40891,#40892,#40893,#40894,#40895),
 .UNSPECIFIED.,.F.,.F.,(4,3,3,3,3,3,3,3,4),(-60.6406912850649,-60.5589640342568,
-59.5661941320559,-58.5734242298549,-57.580654327654,-56.5878844254531,
-55.5951145232521,-54.6023446210512,-54.3575059778853),.UNSPECIFIED.);
#2751=B_SPLINE_CURVE_WITH_KNOTS('',3,(#40896,#40897,#40898,#40899,#40900,
#40901,#40902,#40903,#40904,#40905,#40906,#40907,#40908,#40909,#40910,#40911,
#40912,#40913,#40914,#40915,#40916,#40917,#40918,#40919,#40920),
 .UNSPECIFIED.,.F.,.F.,(4,3,3,3,3,3,3,3,4),(51.3882242638976,51.6620091576461,
52.6555093337547,53.6490095098633,54.6425096859719,55.6360098620804,56.629510038189,
57.6230102142976,57.6714095710772),.UNSPECIFIED.);
#2752=B_SPLINE_CURVE_WITH_KNOTS('',3,(#40925,#40926,#40927,#40928,#40929,
#40930,#40931,#40932,#40933,#40934,#40935,#40936,#40937,#40938,#40939,#40940,
#40941,#40942,#40943,#40944,#40945,#40946),.UNSPECIFIED.,.F.,.F.,(4,3,3,
3,3,3,3,4),(-66.9238765922445,-66.5155834474624,-65.5228135452614,-64.5300436430605,
-63.5372737408596,-62.5445038386586,-61.5517339364577,-60.6406912850649),
 .UNSPECIFIED.);
#2753=B_SPLINE_CURVE_WITH_KNOTS('',3,(#40947,#40948,#40949,#40950,#40951,
#40952,#40953,#40954,#40955,#40956,#40957,#40958,#40959,#40960,#40961,#40962,
#40963,#40964,#40965,#40966,#40967,#40968),.UNSPECIFIED.,.F.,.F.,(4,3,3,
3,3,3,3,4),(57.6714095710772,58.6165103904062,59.6100105665148,60.6035107426233,
61.5970109187319,62.5905110948405,63.5840112709491,63.9545948782568),
 .UNSPECIFIED.);
#2754=B_SPLINE_CURVE_WITH_KNOTS('',3,(#40973,#40974,#40975,#40976,#40977,
#40978,#40979,#40980,#40981,#40982,#40983,#40984,#40985,#40986,#40987,#40988,
#40989,#40990,#40991,#40992,#40993,#40994),.UNSPECIFIED.,.F.,.F.,(4,3,3,
3,3,3,3,4),(-73.207061899424,-72.4722028606679,-71.479432958467,-70.4866630562661,
-69.4938931540652,-68.5011232518642,-67.5083533496633,-66.9238765922445),
 .UNSPECIFIED.);
#2755=B_SPLINE_CURVE_WITH_KNOTS('',3,(#40995,#40996,#40997,#40998,#40999,
#41000,#41001,#41002,#41003,#41004,#41005,#41006,#41007,#41008,#41009,#41010,
#41011,#41012,#41013,#41014,#41015,#41016),.UNSPECIFIED.,.F.,.F.,(4,3,3,
3,3,3,3,4),(63.9545948782568,64.5775114470576,65.5710116231662,66.5645117992748,
67.5580119753834,68.551512151492,69.5450123276005,70.2377801854364),
 .UNSPECIFIED.);
#2756=B_SPLINE_CURVE_WITH_KNOTS('',3,(#41021,#41022,#41023,#41024,#41025,
#41026,#41027,#41028,#41029,#41030,#41031,#41032,#41033,#41034,#41035,#41036,
#41037,#41038,#41039,#41040,#41041,#41042,#41043,#41044,#41045),
 .UNSPECIFIED.,.F.,.F.,(4,3,3,3,3,3,3,3,4),(-79.4902472066036,-79.4215921760745,
-78.4288222738735,-77.4360523716726,-76.4432824694717,-75.4505125672707,
-74.4577426650698,-73.4649727628689,-73.207061899424),.UNSPECIFIED.);
#2757=B_SPLINE_CURVE_WITH_KNOTS('',3,(#41046,#41047,#41048,#41049,#41050,
#41051,#41052,#41053,#41054,#41055,#41056,#41057,#41058,#41059,#41060,#41061,
#41062,#41063,#41064,#41065,#41066,#41067,#41068,#41069,#41070),
 .UNSPECIFIED.,.F.,.F.,(4,3,3,3,3,3,3,3,4),(70.2377801854364,70.5385125037091,
71.5320126798177,72.5255128559263,73.5190130320348,74.5125132081434,75.506013384252,
76.4995135603606,76.520965492616),.UNSPECIFIED.);
#2758=B_SPLINE_CURVE_WITH_KNOTS('',3,(#41075,#41076,#41077,#41078,#41079,
#41080,#41081,#41082,#41083,#41084,#41085,#41086,#41087,#41088,#41089,#41090,
#41091,#41092,#41093,#41094,#41095,#41096),.UNSPECIFIED.,.F.,.F.,(4,3,3,
3,3,3,3,4),(-85.7734325137832,-85.3782115892801,-84.3854416870791,-83.3926717848782,
-82.3999018826773,-81.4071319804763,-80.4143620782754,-79.4902472066036),
 .UNSPECIFIED.);
#2759=B_SPLINE_CURVE_WITH_KNOTS('',3,(#41097,#41098,#41099,#41100,#41101,
#41102,#41103,#41104,#41105,#41106,#41107,#41108,#41109,#41110,#41111,#41112,
#41113,#41114,#41115,#41116,#41117,#41118),.UNSPECIFIED.,.F.,.F.,(4,3,3,
3,3,3,3,4),(76.520965492616,77.4930137364692,78.4865139125777,79.4800140886863,
80.4735142647949,81.4670144409035,82.4605146170121,82.8041507997956),
 .UNSPECIFIED.);
#2760=B_SPLINE_CURVE_WITH_KNOTS('',3,(#41123,#41124,#41125,#41126,#41127,
#41128,#41129,#41130,#41131,#41132,#41133,#41134,#41135,#41136,#41137,#41138,
#41139,#41140,#41141,#41142,#41143,#41144),.UNSPECIFIED.,.F.,.F.,(4,3,3,
3,3,3,3,4),(-92.0566178209628,-91.3348310024856,-90.3420611002847,-89.3492911980838,
-88.3565212958828,-87.3637513936819,-86.370981491481,-85.7734325137832),
 .UNSPECIFIED.);
#2761=B_SPLINE_CURVE_WITH_KNOTS('',3,(#41145,#41146,#41147,#41148,#41149,
#41150,#41151,#41152,#41153,#41154,#41155,#41156,#41157,#41158,#41159,#41160,
#41161,#41162,#41163,#41164,#41165,#41166),.UNSPECIFIED.,.F.,.F.,(4,3,3,
3,3,3,3,4),(82.8041507997956,83.4540147931206,84.4475149692292,85.4410151453378,
86.4345153214464,87.428015497555,88.4215156736635,89.0873361069751),
 .UNSPECIFIED.);
#2762=B_SPLINE_CURVE_WITH_KNOTS('',3,(#41171,#41172,#41173,#41174,#41175,
#41176,#41177,#41178,#41179,#41180,#41181,#41182,#41183,#41184,#41185,#41186,
#41187,#41188,#41189,#41190,#41191,#41192,#41193,#41194,#41195),
 .UNSPECIFIED.,.F.,.F.,(4,3,3,3,3,3,3,3,4),(-98.3398031281424,-98.2842203178921,
-97.2914504156912,-96.2986805134903,-95.3059106112893,-94.3131407090884,
-93.3203708068875,-92.3276009046866,-92.0566178209628),.UNSPECIFIED.);
#2763=B_SPLINE_CURVE_WITH_KNOTS('',3,(#41196,#41197,#41198,#41199,#41200,
#41201,#41202,#41203,#41204,#41205,#41206,#41207,#41208,#41209,#41210,#41211,
#41212,#41213,#41214,#41215,#41216,#41217),.UNSPECIFIED.,.F.,.F.,(4,3,3,
3,3,3,3,4),(89.0873361069751,89.4150158497721,90.4085160258807,91.4020162019893,
92.3955163780979,93.3890165542064,94.382516730315,95.3705214141547),
 .UNSPECIFIED.);
#2764=B_SPLINE_CURVE_WITH_KNOTS('',3,(#41222,#41223,#41224,#41225,#41226,
#41227,#41228,#41229,#41230,#41231,#41232,#41233,#41234,#41235,#41236,#41237,
#41238,#41239,#41240,#41241,#41242,#41243),.UNSPECIFIED.,.F.,.F.,(4,3,3,
3,3,3,3,4),(-104.622988435322,-104.240839731098,-103.248069828897,-102.255299926696,
-101.262530024495,-100.269760122294,-99.2769902200931,-98.3398031281424),
 .UNSPECIFIED.);
#2765=B_SPLINE_CURVE_WITH_KNOTS('',3,(#41244,#41245,#41246,#41247,#41248,
#41249,#41250,#41251,#41252,#41253,#41254,#41255,#41256,#41257,#41258,#41259,
#41260,#41261,#41262,#41263,#41264,#41265),.UNSPECIFIED.,.F.,.F.,(4,3,3,
3,3,3,3,4),(95.3705214141547,96.3695170825322,97.3630172586407,98.3565174347493,
99.3500176108579,100.343517786966,101.337017963075,101.653706721334),
 .UNSPECIFIED.);
#2766=B_SPLINE_CURVE_WITH_KNOTS('',3,(#41270,#41271,#41272,#41273,#41274,
#41275,#41276,#41277,#41278,#41279,#41280,#41281,#41282,#41283,#41284,#41285,
#41286,#41287,#41288,#41289,#41290,#41291),.UNSPECIFIED.,.F.,.F.,(4,3,3,
3,3,3,3,4),(-110.906173742502,-110.197459144303,-109.204689242102,-108.211919339901,
-107.219149437701,-106.2263795355,-105.233609633299,-104.622988435322),
 .UNSPECIFIED.);
#2767=B_SPLINE_CURVE_WITH_KNOTS('',3,(#41292,#41293,#41294,#41295,#41296,
#41297,#41298,#41299,#41300,#41301,#41302,#41303,#41304,#41305,#41306,#41307,
#41308,#41309,#41310,#41311,#41312,#41313),.UNSPECIFIED.,.F.,.F.,(4,3,3,
3,3,3,3,4),(101.653706721334,102.330518139184,103.324018315292,104.317518491401,
105.311018667509,106.304518843618,107.298019019727,107.936892028514),
 .UNSPECIFIED.);
#2768=B_SPLINE_CURVE_WITH_KNOTS('',3,(#41319,#41320,#41321,#41322,#41323,
#41324,#41325,#41326,#41327,#41328),.UNSPECIFIED.,.F.,.F.,(4,1,1,1,1,1,
1,4),(122.522113490002,122.806168794005,123.798938696205,124.791708598406,
125.784478500607,126.777248402808,127.770018305009,128.76278820721),
 .UNSPECIFIED.);
#2769=B_SPLINE_CURVE_WITH_KNOTS('',3,(#41331,#41332,#41333,#41334,#41335,
#41336,#41337,#41338,#41339),.UNSPECIFIED.,.F.,.F.,(4,1,1,1,1,1,4),(122.522113490002,
122.554556406795,123.548056582903,124.541556759012,125.535056935121,126.528557111229,
127.522057287338),.UNSPECIFIED.);
#2770=B_SPLINE_CURVE_WITH_KNOTS('',3,(#41344,#41345,#41346,#41347,#41348,
#41349,#41350,#41351,#41352,#41353),.UNSPECIFIED.,.F.,.F.,(4,1,1,1,1,1,
1,4),(116.238928182822,116.849549380799,117.842319283,118.835089185201,
119.827859087402,120.820628989603,121.813398891804,122.522113490002),
 .UNSPECIFIED.);
#2771=B_SPLINE_CURVE_WITH_KNOTS('',3,(#41354,#41355,#41356,#41357,#41358,
#41359,#41360,#41361,#41362,#41363),.UNSPECIFIED.,.F.,.F.,(4,1,1,1,1,1,
1,4),(116.238928182822,116.593555350143,117.587055526252,118.580555702361,
119.574055878469,120.567556054578,121.561056230686,122.522113490002),
 .UNSPECIFIED.);
#2772=B_SPLINE_CURVE_WITH_KNOTS('',3,(#41368,#41369,#41370,#41371,#41372,
#41373,#41374,#41375,#41376,#41377),.UNSPECIFIED.,.F.,.F.,(4,1,1,1,1,1,
1,4),(109.955742875643,110.892929967593,111.885699869794,112.878469771995,
113.871239674196,114.864009576397,115.856779478598,116.238928182822),
 .UNSPECIFIED.);
#2773=B_SPLINE_CURVE_WITH_KNOTS('',3,(#41378,#41379,#41380,#41381,#41382,
#41383,#41384,#41385,#41386,#41387),.UNSPECIFIED.,.F.,.F.,(4,1,1,1,1,1,
1,4),(109.955742875643,110.632554293492,111.626054469601,112.619554645709,
113.613054821818,114.606554997926,115.600055174035,116.238928182822),
 .UNSPECIFIED.);
#2774=B_SPLINE_CURVE_WITH_KNOTS('',3,(#41392,#41393,#41394,#41395,#41396,
#41397,#41398,#41399,#41400,#41401,#41402),.UNSPECIFIED.,.F.,.F.,(4,1,1,
1,1,1,1,1,4),(103.672557568463,103.943540652187,104.936310554388,105.929080456589,
106.92185035879,107.914620260991,108.907390163192,109.900160065392,109.955742875643),
 .UNSPECIFIED.);
#2775=B_SPLINE_CURVE_WITH_KNOTS('',3,(#41403,#41404,#41405,#41406,#41407,
#41408,#41409,#41410,#41411,#41412,#41413),.UNSPECIFIED.,.F.,.F.,(4,1,1,
1,1,1,1,1,4),(103.672557568463,103.678053060732,104.67155323684,105.665053412949,
106.658553589058,107.652053765166,108.645553941275,109.639054117383,109.955742875643),
 .UNSPECIFIED.);
#2776=B_SPLINE_CURVE_WITH_KNOTS('',3,(#41418,#41419,#41420,#41421,#41422,
#41423,#41424,#41425,#41426,#41427),.UNSPECIFIED.,.F.,.F.,(4,1,1,1,1,1,
1,4),(97.3893722612836,97.9869212389813,98.9796911411822,99.9724610433832,
100.965230945584,101.958000847785,102.950770749986,103.672557568463),
 .UNSPECIFIED.);
#2777=B_SPLINE_CURVE_WITH_KNOTS('',3,(#41428,#41429,#41430,#41431,#41432,
#41433,#41434,#41435,#41436,#41437),.UNSPECIFIED.,.F.,.F.,(4,1,1,1,1,1,
1,4),(97.3893722612835,97.7170520040804,98.710552180189,99.7040523562976,
100.697552532406,101.691052708515,102.684552884623,103.672557568463),
 .UNSPECIFIED.);
#2778=B_SPLINE_CURVE_WITH_KNOTS('',3,(#41442,#41443,#41444,#41445,#41446,
#41447,#41448,#41449,#41450,#41451),.UNSPECIFIED.,.F.,.F.,(4,1,1,1,1,1,
1,4),(91.106186954104,92.0303018257757,93.0230717279766,94.0158416301776,
95.0086115323785,96.0013814345794,96.9941513367804,97.3893722612836),
 .UNSPECIFIED.);
#2779=B_SPLINE_CURVE_WITH_KNOTS('',3,(#41452,#41453,#41454,#41455,#41456,
#41457,#41458,#41459,#41460,#41461),.UNSPECIFIED.,.F.,.F.,(4,1,1,1,1,1,
1,4),(91.106186954104,91.756050947429,92.7495511235375,93.7430512996461,
94.7365514757547,95.7300516518633,96.7235518279718,97.3893722612835),
 .UNSPECIFIED.);
#2780=B_SPLINE_CURVE_WITH_KNOTS('',3,(#41466,#41467,#41468,#41469,#41470,
#41471,#41472,#41473,#41474,#41475,#41476),.UNSPECIFIED.,.F.,.F.,(4,1,1,
1,1,1,1,1,4),(84.8230016469244,85.0809125103692,86.0736824125701,87.0664523147711,
88.059222216972,89.0519921191729,90.0447620213739,91.0375319235748,91.106186954104),
 .UNSPECIFIED.);
#2781=B_SPLINE_CURVE_WITH_KNOTS('',3,(#41477,#41478,#41479,#41480,#41481,
#41482,#41483,#41484,#41485,#41486),.UNSPECIFIED.,.F.,.F.,(4,1,1,1,1,1,
1,4),(84.8230016469244,85.7950498907775,86.7885500668861,87.7820502429946,
88.7755504191032,89.7690505952118,90.7625507713204,91.106186954104),
 .UNSPECIFIED.);
#2782=B_SPLINE_CURVE_WITH_KNOTS('',3,(#41491,#41492,#41493,#41494,#41495,
#41496,#41497,#41498,#41499,#41500),.UNSPECIFIED.,.F.,.F.,(4,1,1,1,1,1,
1,4),(78.5398163397448,79.1242930971636,80.1170629993645,81.1098329015655,
82.1026028037664,83.0953727059673,84.0881426081683,84.8230016469244),
 .UNSPECIFIED.);
#2783=B_SPLINE_CURVE_WITH_KNOTS('',3,(#41501,#41502,#41503,#41504,#41505,
#41506,#41507,#41508,#41509,#41510,#41511),.UNSPECIFIED.,.F.,.F.,(4,1,1,
1,1,1,1,1,4),(78.5398163397448,78.8405486580174,79.834048834126,80.8275490102346,
81.8210491863432,82.8145493624517,83.8080495385603,84.8015497146689,84.8230016469244),
 .UNSPECIFIED.);
#2784=B_SPLINE_CURVE_WITH_KNOTS('',3,(#41516,#41517,#41518,#41519,#41520,
#41521,#41522,#41523,#41524,#41525),.UNSPECIFIED.,.F.,.F.,(4,1,1,1,1,1,
1,4),(72.2566310325652,73.167673683958,74.160443586159,75.1532134883599,
76.1459833905608,77.1387532927618,78.1315231949627,78.5398163397448),
 .UNSPECIFIED.);
#2785=B_SPLINE_CURVE_WITH_KNOTS('',3,(#41526,#41527,#41528,#41529,#41530,
#41531,#41532,#41533,#41534,#41535),.UNSPECIFIED.,.F.,.F.,(4,1,1,1,1,1,
1,4),(72.2566310325652,72.879547601366,73.8730477774745,74.8665479535831,
75.8600481296917,76.8535483058003,77.8470484819088,78.5398163397448),
 .UNSPECIFIED.);
#2786=B_SPLINE_CURVE_WITH_KNOTS('',3,(#41540,#41541,#41542,#41543,#41544,
#41545,#41546,#41547,#41548,#41549,#41550),.UNSPECIFIED.,.F.,.F.,(4,1,1,
1,1,1,1,1,4),(65.9734457253856,66.2182843685515,67.2110542707524,68.2038241729534,
69.1965940751543,70.1893639773552,71.1821338795562,72.1749037817571,72.2566310325652),
 .UNSPECIFIED.);
#2787=B_SPLINE_CURVE_WITH_KNOTS('',3,(#41551,#41552,#41553,#41554,#41555,
#41556,#41557,#41558,#41559,#41560),.UNSPECIFIED.,.F.,.F.,(4,1,1,1,1,1,
1,4),(65.9734457253856,66.9185465447145,67.9120467208231,68.9055468969316,
69.8990470730402,70.8925472491488,71.8860474252574,72.2566310325652),
 .UNSPECIFIED.);
#2788=B_SPLINE_CURVE_WITH_KNOTS('',3,(#41565,#41566,#41567,#41568,#41569,
#41570,#41571,#41572,#41573,#41574),.UNSPECIFIED.,.F.,.F.,(4,1,1,1,1,1,
1,4),(59.690260418206,60.2616649553459,61.2544348575469,62.2472047597478,
63.2399746619487,64.2327445641497,65.2255144663506,65.9734457253856),
 .UNSPECIFIED.);
#2789=B_SPLINE_CURVE_WITH_KNOTS('',3,(#41575,#41576,#41577,#41578,#41579,
#41580,#41581,#41582,#41583,#41584,#41585),.UNSPECIFIED.,.F.,.F.,(4,1,1,
1,1,1,1,1,4),(59.690260418206,59.9640453119544,60.957545488063,61.9510456641716,
62.9445458402802,63.9380460163887,64.9315461924973,65.9250463686059,65.9734457253856),
 .UNSPECIFIED.);
#2790=B_SPLINE_CURVE_WITH_KNOTS('',3,(#41590,#41591,#41592,#41593,#41594,
#41595,#41596,#41597,#41598,#41599),.UNSPECIFIED.,.F.,.F.,(4,1,1,1,1,1,
1,4),(53.4070751110264,54.3050455421403,55.2978154443413,56.2905853465422,
57.2833552487431,58.2761251509441,59.268895053145,59.690260418206),
 .UNSPECIFIED.);
#2791=B_SPLINE_CURVE_WITH_KNOTS('',3,(#41600,#41601,#41602,#41603,#41604,
#41605,#41606,#41607,#41608,#41609),.UNSPECIFIED.,.F.,.F.,(4,1,1,1,1,1,
1,4),(53.4070751110264,54.003044255303,54.9965444314115,55.9900446075201,
56.9835447836287,57.9770449597373,58.9705451358458,59.690260418206),
 .UNSPECIFIED.);
#2792=B_SPLINE_CURVE_WITH_KNOTS('',3,(#41614,#41615,#41616,#41617,#41618,
#41619,#41620,#41621,#41622,#41623,#41624),.UNSPECIFIED.,.F.,.F.,(4,1,1,
1,1,1,1,1,4),(47.1238898038468,47.3556562267338,48.3484261289348,49.3411960311357,
50.3339659333366,51.3267358355376,52.3195057377385,53.3122756399394,53.4070751110264),
 .UNSPECIFIED.);
#2793=B_SPLINE_CURVE_WITH_KNOTS('',3,(#41625,#41626,#41627,#41628,#41629,
#41630,#41631,#41632,#41633,#41634),.UNSPECIFIED.,.F.,.F.,(4,1,1,1,1,1,
1,4),(47.1238898038468,48.0420431986515,49.0355433747601,50.0290435508686,
51.0225437269772,52.0160439030858,53.0095440791944,53.4070751110264),
 .UNSPECIFIED.);
#2794=B_SPLINE_CURVE_WITH_KNOTS('',3,(#41639,#41640,#41641,#41642,#41643,
#41644,#41645,#41646,#41647,#41648),.UNSPECIFIED.,.F.,.F.,(4,1,1,1,1,1,
1,4),(40.8407044966672,41.3990368135282,42.3918067157292,43.3845766179301,
44.377346520131,45.370116422332,46.3628863245329,47.1238898038468),
 .UNSPECIFIED.);
#2795=B_SPLINE_CURVE_WITH_KNOTS('',3,(#41649,#41650,#41651,#41652,#41653,
#41654,#41655,#41656,#41657,#41658,#41659),.UNSPECIFIED.,.F.,.F.,(4,1,1,
1,1,1,1,1,4),(40.8407044966672,41.0875419658914,42.081042142,43.0745423181086,
44.0680424942172,45.0615426703257,46.0550428464343,47.0485430225429,47.1238898038468),
 .UNSPECIFIED.);
#2796=B_SPLINE_CURVE_WITH_KNOTS('',3,(#41664,#41665,#41666,#41667,#41668,
#41669,#41670,#41671,#41672,#41673),.UNSPECIFIED.,.F.,.F.,(4,1,1,1,1,1,
1,4),(34.5575191894876,35.4424174003227,36.4351873025236,37.4279572047245,
38.4207271069255,39.4134970091264,40.4062669113273,40.8407044966672),
 .UNSPECIFIED.);
#2797=B_SPLINE_CURVE_WITH_KNOTS('',3,(#41674,#41675,#41676,#41677,#41678,
#41679,#41680,#41681,#41682,#41683),.UNSPECIFIED.,.F.,.F.,(4,1,1,1,1,1,
1,4),(34.5575191894876,35.1265409092399,36.1200410853485,37.1135412614571,
38.1070414375657,39.1005416136743,40.0940417897828,40.8407044966672),
 .UNSPECIFIED.);
#2798=B_SPLINE_CURVE_WITH_KNOTS('',3,(#41688,#41689,#41690,#41691,#41692,
#41693,#41694,#41695,#41696,#41697,#41698),.UNSPECIFIED.,.F.,.F.,(4,1,1,
1,1,1,1,1,4),(28.2743338823081,28.4930280849161,29.4857979871171,30.478567889318,
31.4713377915189,32.4641076937199,33.4568775959208,34.4496474981217,34.5575191894876),
 .UNSPECIFIED.);
#2799=B_SPLINE_CURVE_WITH_KNOTS('',3,(#41699,#41700,#41701,#41702,#41703,
#41704,#41705,#41706,#41707,#41708),.UNSPECIFIED.,.F.,.F.,(4,1,1,1,1,1,
1,4),(28.274333882308,29.1655398525885,30.1590400286971,31.1525402048056,
32.1460403809142,33.1395405570228,34.1330407331314,34.5575191894876),
 .UNSPECIFIED.);
#2800=B_SPLINE_CURVE_WITH_KNOTS('',3,(#41713,#41714,#41715,#41716,#41717,
#41718,#41719,#41720,#41721,#41722),.UNSPECIFIED.,.F.,.F.,(4,1,1,1,1,1,
1,4),(21.9911485751285,22.5364086717106,23.5291785739115,24.5219484761124,
25.5147183783134,26.5074882805143,27.5002581827152,28.2743338823081),
 .UNSPECIFIED.);
#2801=B_SPLINE_CURVE_WITH_KNOTS('',3,(#41723,#41724,#41725,#41726,#41727,
#41728,#41729,#41730,#41731,#41732,#41733),.UNSPECIFIED.,.F.,.F.,(4,1,1,
1,1,1,1,1,4),(21.9911485751284,22.2110386198284,23.204538795937,24.1980389720456,
25.1915391481542,26.1850393242627,27.1785395003713,28.1720396764799,28.274333882308),
 .UNSPECIFIED.);
#2802=B_SPLINE_CURVE_WITH_KNOTS('',3,(#41738,#41739,#41740,#41741,#41742,
#41743,#41744,#41745,#41746,#41747),.UNSPECIFIED.,.F.,.F.,(4,1,1,1,1,1,
1,4),(15.7079632679489,16.579789258505,17.5725591607059,18.5653290629068,
19.5580989651078,20.5508688673087,21.5436387695096,21.9911485751285),
 .UNSPECIFIED.);
#2803=B_SPLINE_CURVE_WITH_KNOTS('',3,(#41748,#41749,#41750,#41751,#41752,
#41753,#41754,#41755,#41756,#41757),.UNSPECIFIED.,.F.,.F.,(4,1,1,1,1,1,
1,4),(15.7079632679489,16.2500375631769,17.2435377392855,18.2370379153941,
19.2305380915027,20.2240382676113,21.2175384437198,21.9911485751284),
 .UNSPECIFIED.);
#2804=B_SPLINE_CURVE_WITH_KNOTS('',3,(#41760,#41761,#41762,#41763,#41764,
#41765,#41766,#41767,#41768,#41769,#41770,#41771,#41772,#41773,#41774,#41775,
#41776,#41777,#41778,#41779,#41780,#41781,#41782,#41783,#41784,#41785,#41786,
#41787,#41788,#41789,#41790,#41791,#41792,#41793,#41794,#41795,#41796,#41797,
#41798,#41799,#41800,#41801,#41802,#41803,#41804,#41805,#41806,#41807,#41808,
#41809,#41810,#41811,#41812,#41813,#41814,#41815,#41816,#41817,#41818,#41819,
#41820,#41821,#41822,#41823,#41824,#41825,#41826,#41827,#41828,#41829,#41830,
#41831,#41832,#41833,#41834,#41835,#41836,#41837,#41838,#41839,#41840,#41841,
#41842,#41843,#41844,#41845,#41846,#41847,#41848,#41849,#41850,#41851,#41852,
#41853,#41854,#41855,#41856,#41857,#41858,#41859,#41860,#41861,#41862,#41863,
#41864,#41865,#41866,#41867,#41868,#41869,#41870,#41871,#41872,#41873,#41874,
#41875,#41876,#41877,#41878,#41879,#41880),.UNSPECIFIED.,.F.,.F.,(4,3,3,
3,3,3,3,3,3,3,3,3,3,3,3,3,3,3,3,3,3,3,3,3,3,3,3,3,3,3,3,3,3,3,3,3,3,3,3,
3,4),(-0.753008129282273,-0.726411087083563,-0.715881786499564,-0.695023186638146,
-0.683336694953651,-0.673827840112005,-0.646303346018245,-0.632512441881234,
-0.6236006747729,-0.596001444533992,-0.585111150938268,-0.576118283133321,
-0.547602758918121,-0.536376015702489,-0.528202226180116,-0.507015336770619,
-0.486225152468931,-0.477897600046977,-0.452583818906367,-0.439178352550759,
-0.427196798483684,-0.40191963698411,-0.385160728199621,-0.376642475484535,
-0.347726720901875,-0.333286923643958,-0.323497787746622,-0.293375916145958,
-0.277554167376485,-0.267492310267894,-0.241337846280271,-0.224844604159538,
-0.216317003933383,-0.18753716728625,-0.170582917097926,-0.162078349438165,
-0.131638003391508,-0.115498895283149,-0.106874758104641,-0.101197657344851,
-0.0965360155478817),.UNSPECIFIED.);
#2805=B_SPLINE_CURVE_WITH_KNOTS('',3,(#41882,#41883,#41884,#41885,#41886,
#41887,#41888,#41889,#41890,#41891,#41892,#41893,#41894,#41895,#41896,#41897,
#41898,#41899,#41900,#41901,#41902,#41903,#41904,#41905,#41906,#41907,#41908,
#41909,#41910,#41911,#41912,#41913,#41914,#41915),.UNSPECIFIED.,.F.,.F.,
(4,3,3,3,3,3,3,3,3,3,3,4),(-0.204609524178367,-0.173916487069214,-0.152160152794692,
-0.142779925772755,-0.129154387771013,-0.104956417030493,-0.0922484622970884,
-0.0691863467228163,-0.0542893062834328,-0.041770965424307,-0.0153008738219011,
0.),.UNSPECIFIED.);
#2806=B_SPLINE_CURVE_WITH_KNOTS('',3,(#41918,#41919,#41920,#41921,#41922,
#41923,#41924,#41925,#41926,#41927,#41928,#41929,#41930,#41931,#41932,#41933),
 .UNSPECIFIED.,.F.,.F.,(4,3,3,3,3,4),(-0.0965360155478817,-0.0724020116609113,
-0.0590192863946756,-0.0503863222172558,-0.0186895043865902,0.),
 .UNSPECIFIED.);
#2807=B_SPLINE_CURVE_WITH_KNOTS('',3,(#42422,#42423,#42424,#42425,#42426,
#42427,#42428,#42429),.UNSPECIFIED.,.F.,.F.,(4,1,1,1,1,4),(11.6159397475003,
12.6087096497013,13.6014795519022,14.5942494541031,15.5870193563041,15.7079632679489),
 .UNSPECIFIED.);
#2808=B_SPLINE_CURVE_WITH_KNOTS('',3,(#42430,#42431,#42432,#42433,#42434,
#42435,#42436,#42437,#42438,#42439,#42440,#42441,#42442,#42443,#42444,#42445,
#42446,#42447,#42448,#42449,#42450,#42451,#42452,#42453,#42454,#42455,#42456,
#42457,#42458,#42459,#42460,#42461,#42462,#42463,#42464,#42465,#42466,#42467,
#42468,#42469,#42470,#42471,#42472,#42473,#42474,#42475,#42476,#42477,#42478,
#42479,#42480,#42481,#42482,#42483,#42484),.UNSPECIFIED.,.F.,.F.,(4,3,3,
3,3,3,3,3,3,3,3,3,3,3,3,3,3,3,4),(-0.275362278356885,-0.262570109468003,
-0.240166040204702,-0.228737803218204,-0.209304350143588,-0.199561001302199,
-0.189130684518224,-0.159734566166372,-0.148075950500899,-0.139790942517999,
-0.124720142759856,-0.107306928893897,-0.096279762610833,-0.086780292972213,
-0.0650852197291597,-0.0467838010330817,-0.0380963509139461,-0.011916188874275,
0.),.UNSPECIFIED.);
#2809=B_SPLINE_CURVE_WITH_KNOTS('',3,(#42485,#42486,#42487,#42488,#42489,
#42490,#42491,#42492,#42493,#42494,#42495,#42496,#42497,#42498,#42499,#42500,
#42501,#42502,#42503),.UNSPECIFIED.,.F.,.F.,(4,3,3,3,3,3,4),(-115.629180729976,
-115.161308655308,-114.168538753107,-113.175768850906,-112.182998948705,
-111.190229046504,-110.906173742502),.UNSPECIFIED.);
#2810=B_SPLINE_CURVE_WITH_KNOTS('',3,(#42506,#42507,#42508,#42509,#42510,
#42511,#42512,#42513,#42514),.UNSPECIFIED.,.F.,.F.,(4,1,1,1,1,1,4),(10.375208827628,
11.282536682634,12.2760368587426,13.2695370348512,14.2630372109598,15.2565373870684,
15.7079632679489),.UNSPECIFIED.);
#2811=B_SPLINE_CURVE_WITH_KNOTS('',3,(#43008,#43009,#43010,#43011,#43012,
#43013,#43014,#43015,#43016,#43017,#43018,#43019,#43020,#43021,#43022,#43023,
#43024,#43025,#43026,#43027,#43028,#43029),.UNSPECIFIED.,.F.,.F.,(4,3,3,
3,3,3,3,4),(107.936892028514,108.291519195835,109.285019371944,110.278519548052,
111.272019724161,112.265519900269,113.259020076378,113.556008056657),
 .UNSPECIFIED.);
#2812=B_SPLINE_CURVE_WITH_KNOTS('',3,(#43030,#43031,#43032,#43033,#43034,
#43035,#43036,#43037,#43038,#43039,#43040,#43041,#43042,#43043,#43044,#43045,
#43046,#43047,#43048,#43049,#43050,#43051,#43052,#43053,#43054,#43055,#43056,
#43057,#43058,#43059,#43060,#43061,#43062,#43063,#43064,#43065,#43066,#43067,
#43068,#43069,#43070,#43071,#43072,#43073,#43074,#43075,#43076,#43077,#43078,
#43079,#43080,#43081),.UNSPECIFIED.,.F.,.F.,(4,3,3,3,3,3,3,3,3,3,3,3,3,
3,3,3,3,4),(-0.276631791712727,-0.266310431017225,-0.251016700765444,-0.236970857216412,
-0.216553357237997,-0.204277578780747,-0.175779167785564,-0.164239042752865,
-0.155154932673123,-0.139868422463251,-0.120223860282124,-0.110723029685393,
-0.100734922391118,-0.0755511917933386,-0.0588149891352748,-0.049317539854096,
-0.0183008691858031,0.),.UNSPECIFIED.);
#2813=B_SPLINE_CURVE_WITH_KNOTS('',3,(#43135,#43136,#43137,#43138,#43139,
#43140,#43141,#43142,#43143,#43144),.UNSPECIFIED.,.F.,.F.,(4,3,3,4),(-4.09323272002468,
-3.87290614346074,-2.90467960759555,-2.06652207565085),.UNSPECIFIED.);
#2814=B_SPLINE_CURVE_WITH_KNOTS('',3,(#43147,#43148,#43149,#43150,#43151,
#43152,#43153,#43154,#43155,#43156),.UNSPECIFIED.,.F.,.F.,(4,3,3,4),(0.,
0.487536136456814,0.97507227291363,1.11488200921596),.UNSPECIFIED.);
#2815=B_SPLINE_CURVE_WITH_KNOTS('',3,(#43161,#43162,#43163,#43164,#43165,
#43166,#43167,#43168,#43169,#43170,#43171,#43172,#43173,#43174,#43175,#43176,
#43177,#43178,#43179,#43180,#43181,#43182),.UNSPECIFIED.,.F.,.F.,(4,3,3,
3,3,3,3,4),(-10.3764180272043,-9.68226535865184,-8.71403882278665,-7.74581228692147,
-6.77758575105629,-5.8093592151911,-4.84113267932592,-4.09323272002468),
 .UNSPECIFIED.);
#2816=B_SPLINE_CURVE_WITH_KNOTS('',3,(#43183,#43184,#43185,#43186,#43187,
#43188,#43189,#43190,#43191,#43192,#43193,#43194,#43195,#43196,#43197,#43198,
#43199,#43200,#43201,#43202,#43203,#43204),.UNSPECIFIED.,.F.,.F.,(4,3,3,
3,3,3,3,4),(1.11488200921596,1.95014454582726,2.92521681874089,3.90028909165452,
4.87536136456815,5.85043363748178,6.82550591039541,7.39806731639555),
 .UNSPECIFIED.);
#2817=B_SPLINE_CURVE_WITH_KNOTS('',3,(#43210,#43211,#43212,#43213,#43214,
#43215,#43216,#43217,#43218,#43219,#43220),.UNSPECIFIED.,.F.,.F.,(4,1,1,
1,1,1,1,1,4),(21.9911485751286,22.2652224424413,23.2334489783065,24.2016755141717,
25.1699020500369,26.138128585902,27.1063551217672,27.5904683896998,28.0745816576324),
 .UNSPECIFIED.);
#2818=B_SPLINE_CURVE_WITH_KNOTS('',3,(#43223,#43224,#43225,#43226,#43227,
#43228,#43229,#43230,#43231),.UNSPECIFIED.,.F.,.F.,(4,1,1,1,1,1,4),(21.9911485751286,
22.9359800452579,23.9110523181715,24.8861245910851,25.8611968639988,26.3487330004556,
26.8362691369124),.UNSPECIFIED.);
#2819=B_SPLINE_CURVE_WITH_KNOTS('',3,(#43236,#43237,#43238,#43239,#43240,
#43241,#43242,#43243,#43244,#43245),.UNSPECIFIED.,.F.,.F.,(4,1,1,1,1,1,
1,4),(15.707963267949,16.4558632272502,17.4240897631154,18.3923162989806,
19.3605428348458,20.3287693707109,21.2969959065761,21.9911485751286),
 .UNSPECIFIED.);
#2820=B_SPLINE_CURVE_WITH_KNOTS('',3,(#43246,#43247,#43248,#43249,#43250,
#43251,#43252,#43253,#43254,#43255,#43256),.UNSPECIFIED.,.F.,.F.,(4,1,1,
1,1,1,1,1,4),(15.707963267949,16.1104741348625,17.0855464077761,18.0606186806897,
19.0356909536033,20.010763226517,20.9858354994306,21.9609077723442,21.9911485751286),
 .UNSPECIFIED.);
#2821=B_SPLINE_CURVE_WITH_KNOTS('',3,(#43259,#43260,#43261,#43262,#43263,
#43264,#43265,#43266,#43267,#43268,#43269,#43270,#43271,#43272,#43273,#43274,
#43275,#43276,#43277,#43278,#43279,#43280,#43281,#43282,#43283,#43284,#43285,
#43286,#43287,#43288,#43289,#43290,#43291,#43292,#43293,#43294,#43295,#43296,
#43297,#43298,#43299,#43300,#43301,#43302,#43303,#43304,#43305,#43306,#43307,
#43308,#43309,#43310,#43311,#43312,#43313,#43314,#43315,#43316,#43317,#43318,
#43319,#43320,#43321,#43322,#43323,#43324,#43325,#43326,#43327,#43328,#43329,
#43330,#43331,#43332,#43333,#43334,#43335,#43336,#43337,#43338,#43339,#43340,
#43341,#43342,#43343,#43344,#43345,#43346,#43347,#43348,#43349,#43350,#43351,
#43352,#43353,#43354,#43355,#43356,#43357,#43358,#43359,#43360,#43361,#43362,
#43363,#43364,#43365,#43366,#43367,#43368,#43369,#43370,#43371,#43372,#43373,
#43374,#43375,#43376,#43377,#43378,#43379,#43380,#43381,#43382,#43383,#43384,
#43385,#43386,#43387,#43388,#43389,#43390,#43391,#43392,#43393,#43394,#43395,
#43396,#43397,#43398,#43399,#43400,#43401,#43402,#43403,#43404,#43405,#43406),
 .UNSPECIFIED.,.F.,.F.,(4,3,3,3,3,3,3,3,3,3,3,3,3,3,3,3,3,3,3,3,3,3,3,3,
3,3,3,3,3,3,3,3,3,3,3,3,3,3,3,3,3,3,3,3,3,3,3,3,3,4),(-2.55484760629189,
-2.48695217528833,-2.44568453284157,-2.42070459558115,-2.35319160200125,
-2.3139257865929,-2.29446012350936,-2.22112134316782,-2.15284489776411,
-2.14778256282628,-2.13140597699043,-2.06209153930656,-2.00885523871797,
-1.98486130911199,-1.96992692853568,-1.89815536257881,-1.83937078561554,
-1.817015847285,-1.80036421341341,-1.72620354597493,-1.67173851911123,-1.64378629426763,
-1.62739425282856,-1.55539099825264,-1.48916408145581,-1.46822556014781,
-1.45145722328267,-1.37758996208556,-1.33403664657543,-1.30743916113377,
-1.29048333106531,-1.2185386082438,-1.1539632168897,-1.12355490177176,-1.10204286950436,
-1.02677942328141,-0.963665843738869,-0.934374946244716,-0.917466118562855,
-0.840611933806436,-0.784435130234986,-0.756523277472602,-0.739287897272494,
-0.66391879015127,-0.595738468922161,-0.571248146417653,-0.555619165378024,
-0.478231758999867,-0.402728776225848,-0.391197505234835),.UNSPECIFIED.);
#2822=B_SPLINE_CURVE_WITH_KNOTS('',3,(#43408,#43409,#43410,#43411,#43412,
#43413,#43414,#43415,#43416,#43417,#43418,#43419,#43420,#43421,#43422,#43423,
#43424,#43425,#43426,#43427,#43428,#43429,#43430,#43431,#43432,#43433,#43434,
#43435,#43436,#43437,#43438,#43439,#43440,#43441,#43442,#43443,#43444,#43445,
#43446,#43447,#43448,#43449,#43450,#43451,#43452,#43453,#43454,#43455,#43456),
 .UNSPECIFIED.,.F.,.F.,(4,3,3,3,3,3,3,3,3,3,3,3,3,3,3,3,4),(-0.691756841576666,
-0.614945525020825,-0.557220644991909,-0.525771290850366,-0.506808473351499,
-0.433893818313954,-0.428434150029101,-0.373272348832725,-0.346954927725707,
-0.325495518311274,-0.254200825411291,-0.207786945243596,-0.17148998018176,
-0.153620305836439,-0.084801943824183,-0.0177085843821423,0.),
 .UNSPECIFIED.);
#2823=B_SPLINE_CURVE_WITH_KNOTS('',3,(#43459,#43460,#43461,#43462,#43463,
#43464,#43465,#43466,#43467,#43468,#43469,#43470,#43471,#43472,#43473,#43474,
#43475,#43476,#43477,#43478,#43479,#43480,#43481,#43482,#43483),
 .UNSPECIFIED.,.F.,.F.,(4,3,3,3,3,3,3,3,4),(-0.391197505234835,-0.376635177103455,
-0.301774337514086,-0.226330753135565,-0.196964234530146,-0.179195669298564,
-0.100760744171276,-0.022735359240347,0.),.UNSPECIFIED.);
#2824=B_SPLINE_CURVE_WITH_KNOTS('',3,(#43576,#43577,#43578,#43579,#43580,
#43581,#43582,#43583,#43584),.UNSPECIFIED.,.F.,.F.,(4,1,1,1,1,1,4),(11.6147305479243,
12.0988438158569,12.5829570837895,13.5511836196547,14.5194101555198,15.487636691385,
15.707963267949),.UNSPECIFIED.);
#2825=B_SPLINE_CURVE_WITH_KNOTS('',3,(#43585,#43586,#43587,#43588,#43589,
#43590,#43591,#43592,#43593,#43594,#43595,#43596,#43597,#43598,#43599,#43600,
#43601,#43602,#43603,#43604,#43605,#43606,#43607,#43608,#43609,#43610,#43611,
#43612,#43613,#43614,#43615,#43616,#43617,#43618,#43619,#43620,#43621,#43622,
#43623,#43624,#43625,#43626,#43627,#43628,#43629,#43630,#43631,#43632,#43633,
#43634,#43635,#43636,#43637,#43638,#43639,#43640,#43641,#43642,#43643,#43644,
#43645,#43646,#43647,#43648),.UNSPECIFIED.,.F.,.F.,(4,3,3,3,3,3,3,3,3,3,
3,3,3,3,3,3,3,3,3,3,3,4),(-0.933975894023133,-0.870172144297646,-0.827170080065546,
-0.803663315340509,-0.727385743658459,-0.693021198251103,-0.668606761857492,
-0.594193624789495,-0.539597646441439,-0.51029826305353,-0.489836959863564,
-0.416327925555324,-0.363092036646369,-0.336301819444199,-0.31659765616087,
-0.24641892633565,-0.203384369919504,-0.167041232727781,-0.150137294418877,
-0.0818130912649662,-0.0151584267138751,0.),.UNSPECIFIED.);
#2826=B_SPLINE_CURVE_WITH_KNOTS('',3,(#43649,#43650,#43651,#43652,#43653,
#43654,#43655,#43656,#43657,#43658,#43659,#43660,#43661,#43662,#43663,#43664,
#43665,#43666,#43667),.UNSPECIFIED.,.F.,.F.,(4,3,3,3,3,3,4),(-14.947051955369,
-14.5233980379778,-13.5551715021126,-12.5869449662474,-11.6187184303822,
-10.650491894517,-10.3764180272043),.UNSPECIFIED.);
#2827=B_SPLINE_CURVE_WITH_KNOTS('',3,(#43670,#43671,#43672,#43673,#43674,
#43675,#43676,#43677,#43678),.UNSPECIFIED.,.F.,.F.,(4,1,1,1,1,1,4),(10.3764180272043,
11.2351127702943,12.2101850432079,13.1852573161216,14.1603295890352,15.1354018619488,
15.707963267949),.UNSPECIFIED.);
#2828=B_SPLINE_CURVE_WITH_KNOTS('',3,(#43776,#43777,#43778,#43779,#43780,
#43781,#43782,#43783,#43784,#43785,#43786,#43787,#43788,#43789,#43790,#43791,
#43792,#43793,#43794,#43795,#43796,#43797),.UNSPECIFIED.,.F.,.F.,(4,3,3,
3,3,3,3,4),(7.39806731639555,7.80057818330904,8.77565045622267,9.7507227291363,
10.7257950020499,11.7008672749636,12.6759395478772,12.8805298797181),
 .UNSPECIFIED.);
#2829=B_SPLINE_CURVE_WITH_KNOTS('',3,(#43798,#43799,#43800,#43801,#43802,
#43803,#43804,#43805,#43806,#43807,#43808,#43809,#43810,#43811,#43812,#43813,
#43814,#43815,#43816,#43817,#43818,#43819,#43820,#43821,#43822,#43823,#43824,
#43825,#43826,#43827,#43828,#43829,#43830,#43831,#43832,#43833,#43834,#43835,
#43836,#43837,#43838,#43839,#43840,#43841,#43842,#43843,#43844,#43845,#43846,
#43847,#43848,#43849,#43850,#43851,#43852,#43853,#43854,#43855,#43856,#43857,
#43858,#43859,#43860,#43861),.UNSPECIFIED.,.F.,.F.,(4,3,3,3,3,3,3,3,3,3,
3,3,3,3,3,3,3,3,3,3,3,4),(-0.937740963081767,-0.889617493595049,-0.848304455696462,
-0.828682446370235,-0.760262135956028,-0.724356285684949,-0.705545676850033,
-0.633958254388594,-0.580112260350483,-0.555771314501388,-0.535484356147626,
-0.4642344184685,-0.40739310428294,-0.380133656928136,-0.358792074193013,
-0.284322152713594,-0.236869161726259,-0.198441507541726,-0.17634790638339,
-0.0995983283272545,-0.0229227240658628,0.),.UNSPECIFIED.);
#2830=LINE('',#14566,#3462);
#2831=LINE('',#14601,#3463);
#2832=LINE('',#14628,#3464);
#2833=LINE('',#14679,#3465);
#2834=LINE('',#14727,#3466);
#2835=LINE('',#14775,#3467);
#2836=LINE('',#14826,#3468);
#2837=LINE('',#14874,#3469);
#2838=LINE('',#14922,#3470);
#2839=LINE('',#14973,#3471);
#2840=LINE('',#15024,#3472);
#2841=LINE('',#15072,#3473);
#2842=LINE('',#15123,#3474);
#2843=LINE('',#15162,#3475);
#2844=LINE('',#15184,#3476);
#2845=LINE('',#15208,#3477);
#2846=LINE('',#15233,#3478);
#2847=LINE('',#15258,#3479);
#2848=LINE('',#15282,#3480);
#2849=LINE('',#15307,#3481);
#2850=LINE('',#15331,#3482);
#2851=LINE('',#15356,#3483);
#2852=LINE('',#15380,#3484);
#2853=LINE('',#15405,#3485);
#2854=LINE('',#15430,#3486);
#2855=LINE('',#15454,#3487);
#2856=LINE('',#15471,#3488);
#2857=LINE('',#15506,#3489);
#2858=LINE('',#15533,#3490);
#2859=LINE('',#15584,#3491);
#2860=LINE('',#15632,#3492);
#2861=LINE('',#15680,#3493);
#2862=LINE('',#15731,#3494);
#2863=LINE('',#15779,#3495);
#2864=LINE('',#15827,#3496);
#2865=LINE('',#15878,#3497);
#2866=LINE('',#15929,#3498);
#2867=LINE('',#15977,#3499);
#2868=LINE('',#16028,#3500);
#2869=LINE('',#16067,#3501);
#2870=LINE('',#16089,#3502);
#2871=LINE('',#16113,#3503);
#2872=LINE('',#16138,#3504);
#2873=LINE('',#16163,#3505);
#2874=LINE('',#16187,#3506);
#2875=LINE('',#16212,#3507);
#2876=LINE('',#16236,#3508);
#2877=LINE('',#16261,#3509);
#2878=LINE('',#16285,#3510);
#2879=LINE('',#16310,#3511);
#2880=LINE('',#16335,#3512);
#2881=LINE('',#16359,#3513);
#2882=LINE('',#16376,#3514);
#2883=LINE('',#16411,#3515);
#2884=LINE('',#16438,#3516);
#2885=LINE('',#16489,#3517);
#2886=LINE('',#16537,#3518);
#2887=LINE('',#16585,#3519);
#2888=LINE('',#16636,#3520);
#2889=LINE('',#16684,#3521);
#2890=LINE('',#16732,#3522);
#2891=LINE('',#16783,#3523);
#2892=LINE('',#16834,#3524);
#2893=LINE('',#16882,#3525);
#2894=LINE('',#16933,#3526);
#2895=LINE('',#16972,#3527);
#2896=LINE('',#16994,#3528);
#2897=LINE('',#17018,#3529);
#2898=LINE('',#17043,#3530);
#2899=LINE('',#17068,#3531);
#2900=LINE('',#17092,#3532);
#2901=LINE('',#17117,#3533);
#2902=LINE('',#17141,#3534);
#2903=LINE('',#17166,#3535);
#2904=LINE('',#17190,#3536);
#2905=LINE('',#17215,#3537);
#2906=LINE('',#17240,#3538);
#2907=LINE('',#17264,#3539);
#2908=LINE('',#17281,#3540);
#2909=LINE('',#17316,#3541);
#2910=LINE('',#17343,#3542);
#2911=LINE('',#17394,#3543);
#2912=LINE('',#17442,#3544);
#2913=LINE('',#17490,#3545);
#2914=LINE('',#17541,#3546);
#2915=LINE('',#17589,#3547);
#2916=LINE('',#17637,#3548);
#2917=LINE('',#17688,#3549);
#2918=LINE('',#17739,#3550);
#2919=LINE('',#17787,#3551);
#2920=LINE('',#17838,#3552);
#2921=LINE('',#17877,#3553);
#2922=LINE('',#17899,#3554);
#2923=LINE('',#17923,#3555);
#2924=LINE('',#17948,#3556);
#2925=LINE('',#17973,#3557);
#2926=LINE('',#17997,#3558);
#2927=LINE('',#18022,#3559);
#2928=LINE('',#18046,#3560);
#2929=LINE('',#18071,#3561);
#2930=LINE('',#18095,#3562);
#2931=LINE('',#18120,#3563);
#2932=LINE('',#18145,#3564);
#2933=LINE('',#18169,#3565);
#2934=LINE('',#18187,#3566);
#2935=LINE('',#18197,#3567);
#2936=LINE('',#18200,#3568);
#2937=LINE('',#18210,#3569);
#2938=LINE('',#18213,#3570);
#2939=LINE('',#22115,#3571);
#2940=LINE('',#22121,#3572);
#2941=LINE('',#22126,#3573);
#2942=LINE('',#22128,#3574);
#2943=LINE('',#22130,#3575);
#2944=LINE('',#22131,#3576);
#2945=LINE('',#22134,#3577);
#2946=LINE('',#22136,#3578);
#2947=LINE('',#22137,#3579);
#2948=LINE('',#22140,#3580);
#2949=LINE('',#22142,#3581);
#2950=LINE('',#22143,#3582);
#2951=LINE('',#22145,#3583);
#2952=LINE('',#22149,#3584);
#2953=LINE('',#22151,#3585);
#2954=LINE('',#22153,#3586);
#2955=LINE('',#22154,#3587);
#2956=LINE('',#22158,#3588);
#2957=LINE('',#22160,#3589);
#2958=LINE('',#22162,#3590);
#2959=LINE('',#22163,#3591);
#2960=LINE('',#22165,#3592);
#2961=LINE('',#22166,#3593);
#2962=LINE('',#22168,#3594);
#2963=LINE('',#22173,#3595);
#2964=LINE('',#22179,#3596);
#2965=LINE('',#22187,#3597);
#2966=LINE('',#22191,#3598);
#2967=LINE('',#22195,#3599);
#2968=LINE('',#22198,#3600);
#2969=LINE('',#22201,#3601);
#2970=LINE('',#22204,#3602);
#2971=LINE('',#22207,#3603);
#2972=LINE('',#22208,#3604);
#2973=LINE('',#22211,#3605);
#2974=LINE('',#22215,#3606);
#2975=LINE('',#22216,#3607);
#2976=LINE('',#22219,#3608);
#2977=LINE('',#22222,#3609);
#2978=LINE('',#22226,#3610);
#2979=LINE('',#22227,#3611);
#2980=LINE('',#22231,#3612);
#2981=LINE('',#22235,#3613);
#2982=LINE('',#22237,#3614);
#2983=LINE('',#22239,#3615);
#2984=LINE('',#22240,#3616);
#2985=LINE('',#22242,#3617);
#2986=LINE('',#22244,#3618);
#2987=LINE('',#22246,#3619);
#2988=LINE('',#22247,#3620);
#2989=LINE('',#22250,#3621);
#2990=LINE('',#22252,#3622);
#2991=LINE('',#22253,#3623);
#2992=LINE('',#22255,#3624);
#2993=LINE('',#22256,#3625);
#2994=LINE('',#22257,#3626);
#2995=LINE('',#22264,#3627);
#2996=LINE('',#22321,#3628);
#2997=LINE('',#22408,#3629);
#2998=LINE('',#22477,#3630);
#2999=LINE('',#22534,#3631);
#3000=LINE('',#22621,#3632);
#3001=LINE('',#22690,#3633);
#3002=LINE('',#22706,#3634);
#3003=LINE('',#22744,#3635);
#3004=LINE('',#22780,#3636);
#3005=LINE('',#22800,#3637);
#3006=LINE('',#22816,#3638);
#3007=LINE('',#22854,#3639);
#3008=LINE('',#22890,#3640);
#3009=LINE('',#22912,#3641);
#3010=LINE('',#22913,#3642);
#3011=LINE('',#22919,#3643);
#3012=LINE('',#22920,#3644);
#3013=LINE('',#22924,#3645);
#3014=LINE('',#22926,#3646);
#3015=LINE('',#22928,#3647);
#3016=LINE('',#22929,#3648);
#3017=LINE('',#22933,#3649);
#3018=LINE('',#22935,#3650);
#3019=LINE('',#22937,#3651);
#3020=LINE('',#22938,#3652);
#3021=LINE('',#22942,#3653);
#3022=LINE('',#22945,#3654);
#3023=LINE('',#22947,#3655);
#3024=LINE('',#22948,#3656);
#3025=LINE('',#22951,#3657);
#3026=LINE('',#22953,#3658);
#3027=LINE('',#22954,#3659);
#3028=LINE('',#22958,#3660);
#3029=LINE('',#22960,#3661);
#3030=LINE('',#22962,#3662);
#3031=LINE('',#24560,#3663);
#3032=LINE('',#24567,#3664);
#3033=LINE('',#24608,#3665);
#3034=LINE('',#24637,#3666);
#3035=LINE('',#24641,#3667);
#3036=LINE('',#24645,#3668);
#3037=LINE('',#24647,#3669);
#3038=LINE('',#24649,#3670);
#3039=LINE('',#24650,#3671);
#3040=LINE('',#24662,#3672);
#3041=LINE('',#24664,#3673);
#3042=LINE('',#24666,#3674);
#3043=LINE('',#24688,#3675);
#3044=LINE('',#24695,#3676);
#3045=LINE('',#24757,#3677);
#3046=LINE('',#24761,#3678);
#3047=LINE('',#24765,#3679);
#3048=LINE('',#24769,#3680);
#3049=LINE('',#24772,#3681);
#3050=LINE('',#24774,#3682);
#3051=LINE('',#24779,#3683);
#3052=LINE('',#24780,#3684);
#3053=LINE('',#24781,#3685);
#3054=LINE('',#24784,#3686);
#3055=LINE('',#24785,#3687);
#3056=LINE('',#24788,#3688);
#3057=LINE('',#24789,#3689);
#3058=LINE('',#24791,#3690);
#3059=LINE('',#24801,#3691);
#3060=LINE('',#24809,#3692);
#3061=LINE('',#24813,#3693);
#3062=LINE('',#24819,#3694);
#3063=LINE('',#24854,#3695);
#3064=LINE('',#24881,#3696);
#3065=LINE('',#24932,#3697);
#3066=LINE('',#24980,#3698);
#3067=LINE('',#25028,#3699);
#3068=LINE('',#25079,#3700);
#3069=LINE('',#25127,#3701);
#3070=LINE('',#25175,#3702);
#3071=LINE('',#25226,#3703);
#3072=LINE('',#25277,#3704);
#3073=LINE('',#25325,#3705);
#3074=LINE('',#25376,#3706);
#3075=LINE('',#25415,#3707);
#3076=LINE('',#25437,#3708);
#3077=LINE('',#25461,#3709);
#3078=LINE('',#25486,#3710);
#3079=LINE('',#25511,#3711);
#3080=LINE('',#25535,#3712);
#3081=LINE('',#25560,#3713);
#3082=LINE('',#25584,#3714);
#3083=LINE('',#25609,#3715);
#3084=LINE('',#25633,#3716);
#3085=LINE('',#25658,#3717);
#3086=LINE('',#25683,#3718);
#3087=LINE('',#25707,#3719);
#3088=LINE('',#25724,#3720);
#3089=LINE('',#25745,#3721);
#3090=LINE('',#25796,#3722);
#3091=LINE('',#25847,#3723);
#3092=LINE('',#25895,#3724);
#3093=LINE('',#25946,#3725);
#3094=LINE('',#25997,#3726);
#3095=LINE('',#26045,#3727);
#3096=LINE('',#26084,#3728);
#3097=LINE('',#26105,#3729);
#3098=LINE('',#26156,#3730);
#3099=LINE('',#26207,#3731);
#3100=LINE('',#26255,#3732);
#3101=LINE('',#26306,#3733);
#3102=LINE('',#26357,#3734);
#3103=LINE('',#26405,#3735);
#3104=LINE('',#26444,#3736);
#3105=LINE('',#26468,#3737);
#3106=LINE('',#26492,#3738);
#3107=LINE('',#26517,#3739);
#3108=LINE('',#26542,#3740);
#3109=LINE('',#26566,#3741);
#3110=LINE('',#26591,#3742);
#3111=LINE('',#26616,#3743);
#3112=LINE('',#26633,#3744);
#3113=LINE('',#26657,#3745);
#3114=LINE('',#26681,#3746);
#3115=LINE('',#26706,#3747);
#3116=LINE('',#26731,#3748);
#3117=LINE('',#26755,#3749);
#3118=LINE('',#26780,#3750);
#3119=LINE('',#26805,#3751);
#3120=LINE('',#27546,#3752);
#3121=LINE('',#27548,#3753);
#3122=LINE('',#27550,#3754);
#3123=LINE('',#27552,#3755);
#3124=LINE('',#27553,#3756);
#3125=LINE('',#29260,#3757);
#3126=LINE('',#29268,#3758);
#3127=LINE('',#29281,#3759);
#3128=LINE('',#29283,#3760);
#3129=LINE('',#29286,#3761);
#3130=LINE('',#29288,#3762);
#3131=LINE('',#29289,#3763);
#3132=LINE('',#29292,#3764);
#3133=LINE('',#29294,#3765);
#3134=LINE('',#29295,#3766);
#3135=LINE('',#29297,#3767);
#3136=LINE('',#29300,#3768);
#3137=LINE('',#29302,#3769);
#3138=LINE('',#29303,#3770);
#3139=LINE('',#29305,#3771);
#3140=LINE('',#29311,#3772);
#3141=LINE('',#29323,#3773);
#3142=LINE('',#29341,#3774);
#3143=LINE('',#29348,#3775);
#3144=LINE('',#29351,#3776);
#3145=LINE('',#29355,#3777);
#3146=LINE('',#29363,#3778);
#3147=LINE('',#29369,#3779);
#3148=LINE('',#29374,#3780);
#3149=LINE('',#29376,#3781);
#3150=LINE('',#29378,#3782);
#3151=LINE('',#29379,#3783);
#3152=LINE('',#29382,#3784);
#3153=LINE('',#29384,#3785);
#3154=LINE('',#29385,#3786);
#3155=LINE('',#29388,#3787);
#3156=LINE('',#29390,#3788);
#3157=LINE('',#29391,#3789);
#3158=LINE('',#29393,#3790);
#3159=LINE('',#29394,#3791);
#3160=LINE('',#29859,#3792);
#3161=LINE('',#29894,#3793);
#3162=LINE('',#29921,#3794);
#3163=LINE('',#29972,#3795);
#3164=LINE('',#30020,#3796);
#3165=LINE('',#30068,#3797);
#3166=LINE('',#30119,#3798);
#3167=LINE('',#30167,#3799);
#3168=LINE('',#30215,#3800);
#3169=LINE('',#30266,#3801);
#3170=LINE('',#30317,#3802);
#3171=LINE('',#30365,#3803);
#3172=LINE('',#30416,#3804);
#3173=LINE('',#30455,#3805);
#3174=LINE('',#30477,#3806);
#3175=LINE('',#30501,#3807);
#3176=LINE('',#30526,#3808);
#3177=LINE('',#30551,#3809);
#3178=LINE('',#30575,#3810);
#3179=LINE('',#30600,#3811);
#3180=LINE('',#30624,#3812);
#3181=LINE('',#30649,#3813);
#3182=LINE('',#30673,#3814);
#3183=LINE('',#30698,#3815);
#3184=LINE('',#30723,#3816);
#3185=LINE('',#30747,#3817);
#3186=LINE('',#30764,#3818);
#3187=LINE('',#30773,#3819);
#3188=LINE('',#30790,#3820);
#3189=LINE('',#30841,#3821);
#3190=LINE('',#30892,#3822);
#3191=LINE('',#30940,#3823);
#3192=LINE('',#30991,#3824);
#3193=LINE('',#31042,#3825);
#3194=LINE('',#31090,#3826);
#3195=LINE('',#31141,#3827);
#3196=LINE('',#31192,#3828);
#3197=LINE('',#31240,#3829);
#3198=LINE('',#31291,#3830);
#3199=LINE('',#31342,#3831);
#3200=LINE('',#31390,#3832);
#3201=LINE('',#31441,#3833);
#3202=LINE('',#31492,#3834);
#3203=LINE('',#31540,#3835);
#3204=LINE('',#31591,#3836);
#3205=LINE('',#31630,#3837);
#3206=LINE('',#31654,#3838);
#3207=LINE('',#31678,#3839);
#3208=LINE('',#31703,#3840);
#3209=LINE('',#31728,#3841);
#3210=LINE('',#31752,#3842);
#3211=LINE('',#31777,#3843);
#3212=LINE('',#31802,#3844);
#3213=LINE('',#31826,#3845);
#3214=LINE('',#31851,#3846);
#3215=LINE('',#31876,#3847);
#3216=LINE('',#31900,#3848);
#3217=LINE('',#31925,#3849);
#3218=LINE('',#31950,#3850);
#3219=LINE('',#31974,#3851);
#3220=LINE('',#31999,#3852);
#3221=LINE('',#32024,#3853);
#3222=LINE('',#32048,#3854);
#3223=LINE('',#34268,#3855);
#3224=LINE('',#34270,#3856);
#3225=LINE('',#34272,#3857);
#3226=LINE('',#34273,#3858);
#3227=LINE('',#34276,#3859);
#3228=LINE('',#34278,#3860);
#3229=LINE('',#34279,#3861);
#3230=LINE('',#34282,#3862);
#3231=LINE('',#34284,#3863);
#3232=LINE('',#34285,#3864);
#3233=LINE('',#34287,#3865);
#3234=LINE('',#34288,#3866);
#3235=LINE('',#34295,#3867);
#3236=LINE('',#34304,#3868);
#3237=LINE('',#34321,#3869);
#3238=LINE('',#34372,#3870);
#3239=LINE('',#34423,#3871);
#3240=LINE('',#34471,#3872);
#3241=LINE('',#34519,#3873);
#3242=LINE('',#34570,#3874);
#3243=LINE('',#34621,#3875);
#3244=LINE('',#34669,#3876);
#3245=LINE('',#34720,#3877);
#3246=LINE('',#34759,#3878);
#3247=LINE('',#34783,#3879);
#3248=LINE('',#34807,#3880);
#3249=LINE('',#34832,#3881);
#3250=LINE('',#34856,#3882);
#3251=LINE('',#34881,#3883);
#3252=LINE('',#34905,#3884);
#3253=LINE('',#34930,#3885);
#3254=LINE('',#34955,#3886);
#3255=LINE('',#34979,#3887);
#3256=LINE('',#35818,#3888);
#3257=LINE('',#35823,#3889);
#3258=LINE('',#35825,#3890);
#3259=LINE('',#35827,#3891);
#3260=LINE('',#35828,#3892);
#3261=LINE('',#35832,#3893);
#3262=LINE('',#35833,#3894);
#3263=LINE('',#35834,#3895);
#3264=LINE('',#35837,#3896);
#3265=LINE('',#35839,#3897);
#3266=LINE('',#35841,#3898);
#3267=LINE('',#35842,#3899);
#3268=LINE('',#35845,#3900);
#3269=LINE('',#35846,#3901);
#3270=LINE('',#35849,#3902);
#3271=LINE('',#35851,#3903);
#3272=LINE('',#35852,#3904);
#3273=LINE('',#35854,#3905);
#3274=LINE('',#35855,#3906);
#3275=LINE('',#35863,#3907);
#3276=LINE('',#35868,#3908);
#3277=LINE('',#35870,#3909);
#3278=LINE('',#35872,#3910);
#3279=LINE('',#35873,#3911);
#3280=LINE('',#35876,#3912);
#3281=LINE('',#35878,#3913);
#3282=LINE('',#35879,#3914);
#3283=LINE('',#35882,#3915);
#3284=LINE('',#35884,#3916);
#3285=LINE('',#35885,#3917);
#3286=LINE('',#35887,#3918);
#3287=LINE('',#35888,#3919);
#3288=LINE('',#35905,#3920);
#3289=LINE('',#35909,#3921);
#3290=LINE('',#36374,#3922);
#3291=LINE('',#36398,#3923);
#3292=LINE('',#36446,#3924);
#3293=LINE('',#36494,#3925);
#3294=LINE('',#36542,#3926);
#3295=LINE('',#36590,#3927);
#3296=LINE('',#36638,#3928);
#3297=LINE('',#36686,#3929);
#3298=LINE('',#36740,#3930);
#3299=LINE('',#36788,#3931);
#3300=LINE('',#36836,#3932);
#3301=LINE('',#36890,#3933);
#3302=LINE('',#36938,#3934);
#3303=LINE('',#36986,#3935);
#3304=LINE('',#37034,#3936);
#3305=LINE('',#37085,#3937);
#3306=LINE('',#37133,#3938);
#3307=LINE('',#37155,#3939);
#3308=LINE('',#37179,#3940);
#3309=LINE('',#37203,#3941);
#3310=LINE('',#37229,#3942);
#3311=LINE('',#37253,#3943);
#3312=LINE('',#37277,#3944);
#3313=LINE('',#37302,#3945);
#3314=LINE('',#37327,#3946);
#3315=LINE('',#37351,#3947);
#3316=LINE('',#37376,#3948);
#3317=LINE('',#37401,#3949);
#3318=LINE('',#37425,#3950);
#3319=LINE('',#37449,#3951);
#3320=LINE('',#37474,#3952);
#3321=LINE('',#37499,#3953);
#3322=LINE('',#37703,#3954);
#3323=LINE('',#38725,#3955);
#3324=LINE('',#38727,#3956);
#3325=LINE('',#38729,#3957);
#3326=LINE('',#38730,#3958);
#3327=LINE('',#38733,#3959);
#3328=LINE('',#38735,#3960);
#3329=LINE('',#38736,#3961);
#3330=LINE('',#38739,#3962);
#3331=LINE('',#38741,#3963);
#3332=LINE('',#38742,#3964);
#3333=LINE('',#38745,#3965);
#3334=LINE('',#38747,#3966);
#3335=LINE('',#38748,#3967);
#3336=LINE('',#38751,#3968);
#3337=LINE('',#38753,#3969);
#3338=LINE('',#38754,#3970);
#3339=LINE('',#38756,#3971);
#3340=LINE('',#38757,#3972);
#3341=LINE('',#38764,#3973);
#3342=LINE('',#38772,#3974);
#3343=LINE('',#38796,#3975);
#3344=LINE('',#38844,#3976);
#3345=LINE('',#38892,#3977);
#3346=LINE('',#38940,#3978);
#3347=LINE('',#38994,#3979);
#3348=LINE('',#39042,#3980);
#3349=LINE('',#39090,#3981);
#3350=LINE('',#39144,#3982);
#3351=LINE('',#39192,#3983);
#3352=LINE('',#39240,#3984);
#3353=LINE('',#39266,#3985);
#3354=LINE('',#39290,#3986);
#3355=LINE('',#39314,#3987);
#3356=LINE('',#39339,#3988);
#3357=LINE('',#39364,#3989);
#3358=LINE('',#39388,#3990);
#3359=LINE('',#39413,#3991);
#3360=LINE('',#39438,#3992);
#3361=LINE('',#39462,#3993);
#3362=LINE('',#39666,#3994);
#3363=LINE('',#40403,#3995);
#3364=LINE('',#40405,#3996);
#3365=LINE('',#40407,#3997);
#3366=LINE('',#40408,#3998);
#3367=LINE('',#40411,#3999);
#3368=LINE('',#40413,#4000);
#3369=LINE('',#40414,#4001);
#3370=LINE('',#40417,#4002);
#3371=LINE('',#40419,#4003);
#3372=LINE('',#40420,#4004);
#3373=LINE('',#40423,#4005);
#3374=LINE('',#40425,#4006);
#3375=LINE('',#40426,#4007);
#3376=LINE('',#40429,#4008);
#3377=LINE('',#40431,#4009);
#3378=LINE('',#40432,#4010);
#3379=LINE('',#40434,#4011);
#3380=LINE('',#40435,#4012);
#3381=LINE('',#40442,#4013);
#3382=LINE('',#40450,#4014);
#3383=LINE('',#40474,#4015);
#3384=LINE('',#40522,#4016);
#3385=LINE('',#40570,#4017);
#3386=LINE('',#40624,#4018);
#3387=LINE('',#40672,#4019);
#3388=LINE('',#40720,#4020);
#3389=LINE('',#40774,#4021);
#3390=LINE('',#40822,#4022);
#3391=LINE('',#40870,#4023);
#3392=LINE('',#40924,#4024);
#3393=LINE('',#40972,#4025);
#3394=LINE('',#41020,#4026);
#3395=LINE('',#41074,#4027);
#3396=LINE('',#41122,#4028);
#3397=LINE('',#41170,#4029);
#3398=LINE('',#41221,#4030);
#3399=LINE('',#41269,#4031);
#3400=LINE('',#41317,#4032);
#3401=LINE('',#41343,#4033);
#3402=LINE('',#41367,#4034);
#3403=LINE('',#41391,#4035);
#3404=LINE('',#41417,#4036);
#3405=LINE('',#41441,#4037);
#3406=LINE('',#41465,#4038);
#3407=LINE('',#41490,#4039);
#3408=LINE('',#41515,#4040);
#3409=LINE('',#41539,#4041);
#3410=LINE('',#41564,#4042);
#3411=LINE('',#41589,#4043);
#3412=LINE('',#41613,#4044);
#3413=LINE('',#41638,#4045);
#3414=LINE('',#41663,#4046);
#3415=LINE('',#41687,#4047);
#3416=LINE('',#41712,#4048);
#3417=LINE('',#41737,#4049);
#3418=LINE('',#41935,#4050);
#3419=LINE('',#43086,#4051);
#3420=LINE('',#43088,#4052);
#3421=LINE('',#43090,#4053);
#3422=LINE('',#43091,#4054);
#3423=LINE('',#43094,#4055);
#3424=LINE('',#43096,#4056);
#3425=LINE('',#43097,#4057);
#3426=LINE('',#43100,#4058);
#3427=LINE('',#43102,#4059);
#3428=LINE('',#43103,#4060);
#3429=LINE('',#43106,#4061);
#3430=LINE('',#43108,#4062);
#3431=LINE('',#43109,#4063);
#3432=LINE('',#43112,#4064);
#3433=LINE('',#43114,#4065);
#3434=LINE('',#43115,#4066);
#3435=LINE('',#43117,#4067);
#3436=LINE('',#43118,#4068);
#3437=LINE('',#43125,#4069);
#3438=LINE('',#43133,#4070);
#3439=LINE('',#43160,#4071);
#3440=LINE('',#43208,#4072);
#3441=LINE('',#43235,#4073);
#3442=LINE('',#43485,#4074);
#3443=LINE('',#43866,#4075);
#3444=LINE('',#43868,#4076);
#3445=LINE('',#43870,#4077);
#3446=LINE('',#43871,#4078);
#3447=LINE('',#43874,#4079);
#3448=LINE('',#43876,#4080);
#3449=LINE('',#43877,#4081);
#3450=LINE('',#43880,#4082);
#3451=LINE('',#43882,#4083);
#3452=LINE('',#43883,#4084);
#3453=LINE('',#43886,#4085);
#3454=LINE('',#43888,#4086);
#3455=LINE('',#43889,#4087);
#3456=LINE('',#43892,#4088);
#3457=LINE('',#43894,#4089);
#3458=LINE('',#43895,#4090);
#3459=LINE('',#43897,#4091);
#3460=LINE('',#43898,#4092);
#3461=LINE('',#43905,#4093);
#3462=VECTOR('',#12273,0.2);
#3463=VECTOR('',#12276,0.2);
#3464=VECTOR('',#12281,0.2);
#3465=VECTOR('',#12284,0.2);
#3466=VECTOR('',#12287,0.2);
#3467=VECTOR('',#12290,0.2);
#3468=VECTOR('',#12293,0.2);
#3469=VECTOR('',#12296,0.2);
#3470=VECTOR('',#12299,0.2);
#3471=VECTOR('',#12302,0.2);
#3472=VECTOR('',#12305,0.2);
#3473=VECTOR('',#12308,0.2);
#3474=VECTOR('',#12311,0.2);
#3475=VECTOR('',#12316,0.205475000000001);
#3476=VECTOR('',#12321,0.205475000000001);
#3477=VECTOR('',#12324,0.205475000000001);
#3478=VECTOR('',#12327,0.205475000000001);
#3479=VECTOR('',#12330,0.205475000000001);
#3480=VECTOR('',#12333,0.205475000000001);
#3481=VECTOR('',#12336,0.205475000000001);
#3482=VECTOR('',#12339,0.205475000000001);
#3483=VECTOR('',#12342,0.205475000000001);
#3484=VECTOR('',#12345,0.205475000000001);
#3485=VECTOR('',#12348,0.205475000000001);
#3486=VECTOR('',#12351,0.205475000000001);
#3487=VECTOR('',#12354,0.205475000000001);
#3488=VECTOR('',#12359,0.2);
#3489=VECTOR('',#12362,0.2);
#3490=VECTOR('',#12367,0.2);
#3491=VECTOR('',#12370,0.2);
#3492=VECTOR('',#12373,0.2);
#3493=VECTOR('',#12376,0.2);
#3494=VECTOR('',#12379,0.2);
#3495=VECTOR('',#12382,0.2);
#3496=VECTOR('',#12385,0.2);
#3497=VECTOR('',#12388,0.2);
#3498=VECTOR('',#12391,0.2);
#3499=VECTOR('',#12394,0.2);
#3500=VECTOR('',#12397,0.2);
#3501=VECTOR('',#12402,0.205475000000001);
#3502=VECTOR('',#12407,0.205475000000001);
#3503=VECTOR('',#12410,0.205475000000001);
#3504=VECTOR('',#12413,0.205475000000001);
#3505=VECTOR('',#12416,0.205475000000001);
#3506=VECTOR('',#12419,0.205475000000001);
#3507=VECTOR('',#12422,0.205475000000001);
#3508=VECTOR('',#12425,0.205475000000001);
#3509=VECTOR('',#12428,0.205475000000001);
#3510=VECTOR('',#12431,0.205475000000001);
#3511=VECTOR('',#12434,0.205475000000001);
#3512=VECTOR('',#12437,0.205475000000001);
#3513=VECTOR('',#12440,0.205475000000001);
#3514=VECTOR('',#12445,0.2);
#3515=VECTOR('',#12448,0.2);
#3516=VECTOR('',#12453,0.2);
#3517=VECTOR('',#12456,0.2);
#3518=VECTOR('',#12459,0.2);
#3519=VECTOR('',#12462,0.2);
#3520=VECTOR('',#12465,0.2);
#3521=VECTOR('',#12468,0.2);
#3522=VECTOR('',#12471,0.2);
#3523=VECTOR('',#12474,0.2);
#3524=VECTOR('',#12477,0.2);
#3525=VECTOR('',#12480,0.2);
#3526=VECTOR('',#12483,0.2);
#3527=VECTOR('',#12488,0.205475);
#3528=VECTOR('',#12493,0.205475);
#3529=VECTOR('',#12496,0.205475);
#3530=VECTOR('',#12499,0.205475);
#3531=VECTOR('',#12502,0.205475);
#3532=VECTOR('',#12505,0.205475);
#3533=VECTOR('',#12508,0.205475);
#3534=VECTOR('',#12511,0.205475);
#3535=VECTOR('',#12514,0.205475);
#3536=VECTOR('',#12517,0.205475);
#3537=VECTOR('',#12520,0.205475);
#3538=VECTOR('',#12523,0.205475);
#3539=VECTOR('',#12526,0.205475);
#3540=VECTOR('',#12531,0.2);
#3541=VECTOR('',#12534,0.2);
#3542=VECTOR('',#12539,0.2);
#3543=VECTOR('',#12542,0.2);
#3544=VECTOR('',#12545,0.2);
#3545=VECTOR('',#12548,0.2);
#3546=VECTOR('',#12551,0.2);
#3547=VECTOR('',#12554,0.2);
#3548=VECTOR('',#12557,0.2);
#3549=VECTOR('',#12560,0.2);
#3550=VECTOR('',#12563,0.2);
#3551=VECTOR('',#12566,0.2);
#3552=VECTOR('',#12569,0.2);
#3553=VECTOR('',#12574,0.205475);
#3554=VECTOR('',#12579,0.205475);
#3555=VECTOR('',#12582,0.205475);
#3556=VECTOR('',#12585,0.205475);
#3557=VECTOR('',#12588,0.205475);
#3558=VECTOR('',#12591,0.205475);
#3559=VECTOR('',#12594,0.205475);
#3560=VECTOR('',#12597,0.205475);
#3561=VECTOR('',#12600,0.205475);
#3562=VECTOR('',#12603,0.205475);
#3563=VECTOR('',#12606,0.205475);
#3564=VECTOR('',#12609,0.205475);
#3565=VECTOR('',#12612,0.205475);
#3566=VECTOR('',#12619,0.6);
#3567=VECTOR('',#12632,0.4);
#3568=VECTOR('',#12635,0.25);
#3569=VECTOR('',#12648,0.4);
#3570=VECTOR('',#12651,0.25);
#3571=VECTOR('',#12690,0.3);
#3572=VECTOR('',#12697,0.3);
#3573=VECTOR('',#12702,1.);
#3574=VECTOR('',#12703,1.);
#3575=VECTOR('',#12704,1.);
#3576=VECTOR('',#12705,1.);
#3577=VECTOR('',#12708,1.);
#3578=VECTOR('',#12709,1.);
#3579=VECTOR('',#12710,1.);
#3580=VECTOR('',#12713,1.);
#3581=VECTOR('',#12714,1.);
#3582=VECTOR('',#12715,1.);
#3583=VECTOR('',#12718,1.);
#3584=VECTOR('',#12721,1.);
#3585=VECTOR('',#12722,1.);
#3586=VECTOR('',#12723,1.);
#3587=VECTOR('',#12724,1.);
#3588=VECTOR('',#12727,1.);
#3589=VECTOR('',#12728,1.);
#3590=VECTOR('',#12729,1.);
#3591=VECTOR('',#12730,1.);
#3592=VECTOR('',#12733,1.);
#3593=VECTOR('',#12734,1.);
#3594=VECTOR('',#12737,1.);
#3595=VECTOR('',#12742,0.65);
#3596=VECTOR('',#12749,0.8);
#3597=VECTOR('',#12758,1.);
#3598=VECTOR('',#12761,1.);
#3599=VECTOR('',#12764,1.);
#3600=VECTOR('',#12767,1.);
#3601=VECTOR('',#12770,1.);
#3602=VECTOR('',#12773,1.);
#3603=VECTOR('',#12776,1.);
#3604=VECTOR('',#12777,1.);
#3605=VECTOR('',#12780,1.);
#3606=VECTOR('',#12785,1.);
#3607=VECTOR('',#12786,1.);
#3608=VECTOR('',#12789,1.);
#3609=VECTOR('',#12792,1.);
#3610=VECTOR('',#12797,1.);
#3611=VECTOR('',#12798,1.);
#3612=VECTOR('',#12805,1.);
#3613=VECTOR('',#12808,1.);
#3614=VECTOR('',#12809,1.);
#3615=VECTOR('',#12810,1.);
#3616=VECTOR('',#12811,1.);
#3617=VECTOR('',#12814,1.);
#3618=VECTOR('',#12815,1.);
#3619=VECTOR('',#12816,1.);
#3620=VECTOR('',#12817,1.);
#3621=VECTOR('',#12820,1.);
#3622=VECTOR('',#12821,1.);
#3623=VECTOR('',#12822,1.);
#3624=VECTOR('',#12825,1.);
#3625=VECTOR('',#12826,1.);
#3626=VECTOR('',#12827,1.);
#3627=VECTOR('',#12836,0.5);
#3628=VECTOR('',#12841,0.5);
#3629=VECTOR('',#12844,0.5);
#3630=VECTOR('',#12849,0.5);
#3631=VECTOR('',#12854,0.5);
#3632=VECTOR('',#12857,0.5);
#3633=VECTOR('',#12862,0.5099);
#3634=VECTOR('',#12867,0.5099);
#3635=VECTOR('',#12870,0.5099);
#3636=VECTOR('',#12873,0.5099);
#3637=VECTOR('',#12878,0.5099);
#3638=VECTOR('',#12883,0.5099);
#3639=VECTOR('',#12886,0.5099);
#3640=VECTOR('',#12889,0.5099);
#3641=VECTOR('',#12896,1.);
#3642=VECTOR('',#12897,1.);
#3643=VECTOR('',#12902,1.);
#3644=VECTOR('',#12903,1.);
#3645=VECTOR('',#12906,1.);
#3646=VECTOR('',#12907,1.);
#3647=VECTOR('',#12908,1.);
#3648=VECTOR('',#12909,1.);
#3649=VECTOR('',#12912,1.);
#3650=VECTOR('',#12913,1.);
#3651=VECTOR('',#12914,1.);
#3652=VECTOR('',#12915,1.);
#3653=VECTOR('',#12920,1.);
#3654=VECTOR('',#12923,1.);
#3655=VECTOR('',#12924,1.);
#3656=VECTOR('',#12925,1.);
#3657=VECTOR('',#12928,1.);
#3658=VECTOR('',#12929,1.);
#3659=VECTOR('',#12930,1.);
#3660=VECTOR('',#12935,1.);
#3661=VECTOR('',#12938,1.);
#3662=VECTOR('',#12941,1.);
#3663=VECTOR('',#12962,0.4);
#3664=VECTOR('',#12971,0.2);
#3665=VECTOR('',#12974,1.);
#3666=VECTOR('',#12977,1.);
#3667=VECTOR('',#12984,1.);
#3668=VECTOR('',#12987,1.);
#3669=VECTOR('',#12988,1.);
#3670=VECTOR('',#12989,1.);
#3671=VECTOR('',#12990,1.);
#3672=VECTOR('',#13001,1.);
#3673=VECTOR('',#13002,1.);
#3674=VECTOR('',#13003,1.);
#3675=VECTOR('',#13016,0.4);
#3676=VECTOR('',#13025,0.2);
#3677=VECTOR('',#13036,0.25);
#3678=VECTOR('',#13041,0.25);
#3679=VECTOR('',#13046,0.25);
#3680=VECTOR('',#13051,0.25);
#3681=VECTOR('',#13056,0.6);
#3682=VECTOR('',#13057,0.6);
#3683=VECTOR('',#13062,1.);
#3684=VECTOR('',#13063,1.);
#3685=VECTOR('',#13064,1.);
#3686=VECTOR('',#13067,1.);
#3687=VECTOR('',#13068,1.);
#3688=VECTOR('',#13071,1.);
#3689=VECTOR('',#13072,1.);
#3690=VECTOR('',#13075,1.);
#3691=VECTOR('',#13088,0.8);
#3692=VECTOR('',#13099,0.4);
#3693=VECTOR('',#13104,0.6);
#3694=VECTOR('',#13111,0.2);
#3695=VECTOR('',#13114,0.2);
#3696=VECTOR('',#13119,0.2);
#3697=VECTOR('',#13122,0.2);
#3698=VECTOR('',#13125,0.2);
#3699=VECTOR('',#13128,0.2);
#3700=VECTOR('',#13131,0.2);
#3701=VECTOR('',#13134,0.2);
#3702=VECTOR('',#13137,0.2);
#3703=VECTOR('',#13140,0.2);
#3704=VECTOR('',#13143,0.2);
#3705=VECTOR('',#13146,0.2);
#3706=VECTOR('',#13149,0.2);
#3707=VECTOR('',#13154,0.205475);
#3708=VECTOR('',#13159,0.205475);
#3709=VECTOR('',#13162,0.205475);
#3710=VECTOR('',#13165,0.205475);
#3711=VECTOR('',#13168,0.205475);
#3712=VECTOR('',#13171,0.205475);
#3713=VECTOR('',#13174,0.205475);
#3714=VECTOR('',#13177,0.205475);
#3715=VECTOR('',#13180,0.205475);
#3716=VECTOR('',#13183,0.205475);
#3717=VECTOR('',#13186,0.205475);
#3718=VECTOR('',#13189,0.205475);
#3719=VECTOR('',#13192,0.205475);
#3720=VECTOR('',#13197,0.15);
#3721=VECTOR('',#13202,0.15);
#3722=VECTOR('',#13205,0.15);
#3723=VECTOR('',#13208,0.15);
#3724=VECTOR('',#13211,0.15);
#3725=VECTOR('',#13214,0.15);
#3726=VECTOR('',#13217,0.15);
#3727=VECTOR('',#13220,0.15);
#3728=VECTOR('',#13225,0.15);
#3729=VECTOR('',#13230,0.15);
#3730=VECTOR('',#13233,0.15);
#3731=VECTOR('',#13236,0.15);
#3732=VECTOR('',#13239,0.15);
#3733=VECTOR('',#13242,0.15);
#3734=VECTOR('',#13245,0.15);
#3735=VECTOR('',#13248,0.15);
#3736=VECTOR('',#13253,0.1543);
#3737=VECTOR('',#13258,0.1543);
#3738=VECTOR('',#13261,0.1543);
#3739=VECTOR('',#13264,0.1543);
#3740=VECTOR('',#13267,0.1543);
#3741=VECTOR('',#13270,0.1543);
#3742=VECTOR('',#13273,0.1543);
#3743=VECTOR('',#13276,0.1543);
#3744=VECTOR('',#13281,0.1543);
#3745=VECTOR('',#13286,0.1543);
#3746=VECTOR('',#13289,0.1543);
#3747=VECTOR('',#13292,0.1543);
#3748=VECTOR('',#13295,0.1543);
#3749=VECTOR('',#13298,0.1543);
#3750=VECTOR('',#13301,0.1543);
#3751=VECTOR('',#13304,0.1543);
#3752=VECTOR('',#13313,1.);
#3753=VECTOR('',#13314,1.);
#3754=VECTOR('',#13315,1.);
#3755=VECTOR('',#13316,1.);
#3756=VECTOR('',#13317,1.);
#3757=VECTOR('',#13342,0.6);
#3758=VECTOR('',#13353,0.6);
#3759=VECTOR('',#13370,1.);
#3760=VECTOR('',#13373,0.6);
#3761=VECTOR('',#13376,1.);
#3762=VECTOR('',#13377,1.);
#3763=VECTOR('',#13378,1.);
#3764=VECTOR('',#13381,1.);
#3765=VECTOR('',#13382,1.);
#3766=VECTOR('',#13383,1.);
#3767=VECTOR('',#13386,1.);
#3768=VECTOR('',#13389,1.);
#3769=VECTOR('',#13390,1.);
#3770=VECTOR('',#13391,1.);
#3771=VECTOR('',#13394,1.);
#3772=VECTOR('',#13403,0.6);
#3773=VECTOR('',#13420,2.2);
#3774=VECTOR('',#13445,0.4);
#3775=VECTOR('',#13454,0.25);
#3776=VECTOR('',#13457,0.6);
#3777=VECTOR('',#13462,1.);
#3778=VECTOR('',#13473,0.2);
#3779=VECTOR('',#13480,0.2);
#3780=VECTOR('',#13485,1.);
#3781=VECTOR('',#13486,1.);
#3782=VECTOR('',#13487,1.);
#3783=VECTOR('',#13488,1.);
#3784=VECTOR('',#13491,1.);
#3785=VECTOR('',#13492,1.);
#3786=VECTOR('',#13493,1.);
#3787=VECTOR('',#13496,1.);
#3788=VECTOR('',#13497,1.);
#3789=VECTOR('',#13498,1.);
#3790=VECTOR('',#13501,1.);
#3791=VECTOR('',#13502,1.);
#3792=VECTOR('',#13521,0.2);
#3793=VECTOR('',#13524,0.2);
#3794=VECTOR('',#13529,0.2);
#3795=VECTOR('',#13532,0.2);
#3796=VECTOR('',#13535,0.2);
#3797=VECTOR('',#13538,0.2);
#3798=VECTOR('',#13541,0.2);
#3799=VECTOR('',#13544,0.2);
#3800=VECTOR('',#13547,0.2);
#3801=VECTOR('',#13550,0.2);
#3802=VECTOR('',#13553,0.2);
#3803=VECTOR('',#13556,0.2);
#3804=VECTOR('',#13559,0.2);
#3805=VECTOR('',#13564,0.205475);
#3806=VECTOR('',#13569,0.205475);
#3807=VECTOR('',#13572,0.205475);
#3808=VECTOR('',#13575,0.205475);
#3809=VECTOR('',#13578,0.205475);
#3810=VECTOR('',#13581,0.205475);
#3811=VECTOR('',#13584,0.205475);
#3812=VECTOR('',#13587,0.205475);
#3813=VECTOR('',#13590,0.205475);
#3814=VECTOR('',#13593,0.205475);
#3815=VECTOR('',#13596,0.205475);
#3816=VECTOR('',#13599,0.205475);
#3817=VECTOR('',#13602,0.205475);
#3818=VECTOR('',#13607,0.15);
#3819=VECTOR('',#13610,0.15);
#3820=VECTOR('',#13617,0.15);
#3821=VECTOR('',#13620,0.15);
#3822=VECTOR('',#13623,0.15);
#3823=VECTOR('',#13626,0.15);
#3824=VECTOR('',#13629,0.15);
#3825=VECTOR('',#13632,0.15);
#3826=VECTOR('',#13635,0.15);
#3827=VECTOR('',#13638,0.15);
#3828=VECTOR('',#13641,0.15);
#3829=VECTOR('',#13644,0.15);
#3830=VECTOR('',#13647,0.15);
#3831=VECTOR('',#13650,0.15);
#3832=VECTOR('',#13653,0.15);
#3833=VECTOR('',#13656,0.15);
#3834=VECTOR('',#13659,0.15);
#3835=VECTOR('',#13662,0.15);
#3836=VECTOR('',#13665,0.15);
#3837=VECTOR('',#13670,0.1543);
#3838=VECTOR('',#13675,0.1543);
#3839=VECTOR('',#13678,0.1543);
#3840=VECTOR('',#13681,0.1543);
#3841=VECTOR('',#13684,0.1543);
#3842=VECTOR('',#13687,0.1543);
#3843=VECTOR('',#13690,0.1543);
#3844=VECTOR('',#13693,0.1543);
#3845=VECTOR('',#13696,0.1543);
#3846=VECTOR('',#13699,0.1543);
#3847=VECTOR('',#13702,0.1543);
#3848=VECTOR('',#13705,0.1543);
#3849=VECTOR('',#13708,0.1543);
#3850=VECTOR('',#13711,0.1543);
#3851=VECTOR('',#13714,0.1543);
#3852=VECTOR('',#13717,0.1543);
#3853=VECTOR('',#13720,0.1543);
#3854=VECTOR('',#13723,0.1543);
#3855=VECTOR('',#13744,1.);
#3856=VECTOR('',#13745,1.);
#3857=VECTOR('',#13746,1.);
#3858=VECTOR('',#13747,1.);
#3859=VECTOR('',#13750,1.);
#3860=VECTOR('',#13751,1.);
#3861=VECTOR('',#13752,1.);
#3862=VECTOR('',#13755,1.);
#3863=VECTOR('',#13756,1.);
#3864=VECTOR('',#13757,1.);
#3865=VECTOR('',#13760,1.);
#3866=VECTOR('',#13761,1.);
#3867=VECTOR('',#13770,0.15);
#3868=VECTOR('',#13773,0.15);
#3869=VECTOR('',#13780,0.15);
#3870=VECTOR('',#13783,0.15);
#3871=VECTOR('',#13786,0.15);
#3872=VECTOR('',#13789,0.15);
#3873=VECTOR('',#13792,0.15);
#3874=VECTOR('',#13795,0.15);
#3875=VECTOR('',#13798,0.15);
#3876=VECTOR('',#13801,0.15);
#3877=VECTOR('',#13804,0.15);
#3878=VECTOR('',#13809,0.1543);
#3879=VECTOR('',#13814,0.1543);
#3880=VECTOR('',#13817,0.1543);
#3881=VECTOR('',#13820,0.1543);
#3882=VECTOR('',#13823,0.1543);
#3883=VECTOR('',#13826,0.1543);
#3884=VECTOR('',#13829,0.1543);
#3885=VECTOR('',#13832,0.1543);
#3886=VECTOR('',#13835,0.1543);
#3887=VECTOR('',#13838,0.1543);
#3888=VECTOR('',#13853,0.2);
#3889=VECTOR('',#13858,1.);
#3890=VECTOR('',#13859,1.);
#3891=VECTOR('',#13860,1.);
#3892=VECTOR('',#13861,1.);
#3893=VECTOR('',#13864,1.);
#3894=VECTOR('',#13865,1.);
#3895=VECTOR('',#13866,1.);
#3896=VECTOR('',#13869,1.);
#3897=VECTOR('',#13870,1.);
#3898=VECTOR('',#13871,1.);
#3899=VECTOR('',#13872,1.);
#3900=VECTOR('',#13875,1.);
#3901=VECTOR('',#13876,1.);
#3902=VECTOR('',#13879,1.);
#3903=VECTOR('',#13880,1.);
#3904=VECTOR('',#13881,1.);
#3905=VECTOR('',#13884,1.);
#3906=VECTOR('',#13885,1.);
#3907=VECTOR('',#13896,0.2);
#3908=VECTOR('',#13901,1.);
#3909=VECTOR('',#13902,1.);
#3910=VECTOR('',#13903,1.);
#3911=VECTOR('',#13904,1.);
#3912=VECTOR('',#13907,1.);
#3913=VECTOR('',#13908,1.);
#3914=VECTOR('',#13909,1.);
#3915=VECTOR('',#13912,1.);
#3916=VECTOR('',#13913,1.);
#3917=VECTOR('',#13914,1.);
#3918=VECTOR('',#13917,1.);
#3919=VECTOR('',#13918,1.);
#3920=VECTOR('',#13941,0.35);
#3921=VECTOR('',#13946,0.2);
#3922=VECTOR('',#13965,0.2);
#3923=VECTOR('',#13970,0.2);
#3924=VECTOR('',#13973,0.2);
#3925=VECTOR('',#13976,0.2);
#3926=VECTOR('',#13979,0.2);
#3927=VECTOR('',#13982,0.2);
#3928=VECTOR('',#13985,0.2);
#3929=VECTOR('',#13988,0.2);
#3930=VECTOR('',#13991,0.2);
#3931=VECTOR('',#13994,0.2);
#3932=VECTOR('',#13997,0.2);
#3933=VECTOR('',#14000,0.2);
#3934=VECTOR('',#14003,0.2);
#3935=VECTOR('',#14006,0.2);
#3936=VECTOR('',#14009,0.2);
#3937=VECTOR('',#14012,0.2);
#3938=VECTOR('',#14015,0.15555);
#3939=VECTOR('',#14020,0.15555);
#3940=VECTOR('',#14023,0.15555);
#3941=VECTOR('',#14026,0.15555);
#3942=VECTOR('',#14029,0.15555);
#3943=VECTOR('',#14032,0.15555);
#3944=VECTOR('',#14035,0.15555);
#3945=VECTOR('',#14038,0.15555);
#3946=VECTOR('',#14041,0.15555);
#3947=VECTOR('',#14044,0.15555);
#3948=VECTOR('',#14047,0.15555);
#3949=VECTOR('',#14050,0.15555);
#3950=VECTOR('',#14053,0.15555);
#3951=VECTOR('',#14056,0.15555);
#3952=VECTOR('',#14059,0.15555);
#3953=VECTOR('',#14062,0.15555);
#3954=VECTOR('',#14067,0.15);
#3955=VECTOR('',#14078,1.);
#3956=VECTOR('',#14079,1.);
#3957=VECTOR('',#14080,1.);
#3958=VECTOR('',#14081,1.);
#3959=VECTOR('',#14084,1.);
#3960=VECTOR('',#14085,1.);
#3961=VECTOR('',#14086,1.);
#3962=VECTOR('',#14089,1.);
#3963=VECTOR('',#14090,1.);
#3964=VECTOR('',#14091,1.);
#3965=VECTOR('',#14094,1.);
#3966=VECTOR('',#14095,1.);
#3967=VECTOR('',#14096,1.);
#3968=VECTOR('',#14099,1.);
#3969=VECTOR('',#14100,1.);
#3970=VECTOR('',#14101,1.);
#3971=VECTOR('',#14104,1.);
#3972=VECTOR('',#14105,1.);
#3973=VECTOR('',#14114,0.35);
#3974=VECTOR('',#14125,0.15);
#3975=VECTOR('',#14130,0.15);
#3976=VECTOR('',#14133,0.15);
#3977=VECTOR('',#14136,0.15);
#3978=VECTOR('',#14139,0.15);
#3979=VECTOR('',#14142,0.15);
#3980=VECTOR('',#14145,0.15);
#3981=VECTOR('',#14148,0.15);
#3982=VECTOR('',#14151,0.15);
#3983=VECTOR('',#14154,0.15);
#3984=VECTOR('',#14157,0.117775);
#3985=VECTOR('',#14162,0.117775);
#3986=VECTOR('',#14165,0.117775);
#3987=VECTOR('',#14168,0.117775);
#3988=VECTOR('',#14171,0.117775);
#3989=VECTOR('',#14174,0.117775);
#3990=VECTOR('',#14177,0.117775);
#3991=VECTOR('',#14180,0.117775);
#3992=VECTOR('',#14183,0.117775);
#3993=VECTOR('',#14186,0.117775);
#3994=VECTOR('',#14191,0.1);
#3995=VECTOR('',#14202,1.);
#3996=VECTOR('',#14203,1.);
#3997=VECTOR('',#14204,1.);
#3998=VECTOR('',#14205,1.);
#3999=VECTOR('',#14208,1.);
#4000=VECTOR('',#14209,1.);
#4001=VECTOR('',#14210,1.);
#4002=VECTOR('',#14213,1.);
#4003=VECTOR('',#14214,1.);
#4004=VECTOR('',#14215,1.);
#4005=VECTOR('',#14218,1.);
#4006=VECTOR('',#14219,1.);
#4007=VECTOR('',#14220,1.);
#4008=VECTOR('',#14223,1.);
#4009=VECTOR('',#14224,1.);
#4010=VECTOR('',#14225,1.);
#4011=VECTOR('',#14228,1.);
#4012=VECTOR('',#14229,1.);
#4013=VECTOR('',#14238,0.3);
#4014=VECTOR('',#14249,0.15);
#4015=VECTOR('',#14254,0.15);
#4016=VECTOR('',#14257,0.15);
#4017=VECTOR('',#14260,0.15);
#4018=VECTOR('',#14263,0.15);
#4019=VECTOR('',#14266,0.15);
#4020=VECTOR('',#14269,0.15);
#4021=VECTOR('',#14272,0.15);
#4022=VECTOR('',#14275,0.15);
#4023=VECTOR('',#14278,0.15);
#4024=VECTOR('',#14281,0.15);
#4025=VECTOR('',#14284,0.15);
#4026=VECTOR('',#14287,0.15);
#4027=VECTOR('',#14290,0.15);
#4028=VECTOR('',#14293,0.15);
#4029=VECTOR('',#14296,0.15);
#4030=VECTOR('',#14299,0.15);
#4031=VECTOR('',#14302,0.15);
#4032=VECTOR('',#14305,0.117775);
#4033=VECTOR('',#14310,0.117775);
#4034=VECTOR('',#14313,0.117775);
#4035=VECTOR('',#14316,0.117775);
#4036=VECTOR('',#14319,0.117775);
#4037=VECTOR('',#14322,0.117775);
#4038=VECTOR('',#14325,0.117775);
#4039=VECTOR('',#14328,0.117775);
#4040=VECTOR('',#14331,0.117775);
#4041=VECTOR('',#14334,0.117775);
#4042=VECTOR('',#14337,0.117775);
#4043=VECTOR('',#14340,0.117775);
#4044=VECTOR('',#14343,0.117775);
#4045=VECTOR('',#14346,0.117775);
#4046=VECTOR('',#14349,0.117775);
#4047=VECTOR('',#14352,0.117775);
#4048=VECTOR('',#14355,0.117775);
#4049=VECTOR('',#14358,0.117775);
#4050=VECTOR('',#14363,0.1);
#4051=VECTOR('',#14374,1.);
#4052=VECTOR('',#14375,1.);
#4053=VECTOR('',#14376,1.);
#4054=VECTOR('',#14377,1.);
#4055=VECTOR('',#14380,1.);
#4056=VECTOR('',#14381,1.);
#4057=VECTOR('',#14382,1.);
#4058=VECTOR('',#14385,1.);
#4059=VECTOR('',#14386,1.);
#4060=VECTOR('',#14387,1.);
#4061=VECTOR('',#14390,1.);
#4062=VECTOR('',#14391,1.);
#4063=VECTOR('',#14392,1.);
#4064=VECTOR('',#14395,1.);
#4065=VECTOR('',#14396,1.);
#4066=VECTOR('',#14397,1.);
#4067=VECTOR('',#14400,1.);
#4068=VECTOR('',#14401,1.);
#4069=VECTOR('',#14410,0.3);
#4070=VECTOR('',#14421,0.5);
#4071=VECTOR('',#14426,0.5);
#4072=VECTOR('',#14429,0.40705);
#4073=VECTOR('',#14434,0.40705);
#4074=VECTOR('',#14439,0.45);
#4075=VECTOR('',#14450,1.);
#4076=VECTOR('',#14451,1.);
#4077=VECTOR('',#14452,1.);
#4078=VECTOR('',#14453,1.);
#4079=VECTOR('',#14456,1.);
#4080=VECTOR('',#14457,1.);
#4081=VECTOR('',#14458,1.);
#4082=VECTOR('',#14461,1.);
#4083=VECTOR('',#14462,1.);
#4084=VECTOR('',#14463,1.);
#4085=VECTOR('',#14466,1.);
#4086=VECTOR('',#14467,1.);
#4087=VECTOR('',#14468,1.);
#4088=VECTOR('',#14471,1.);
#4089=VECTOR('',#14472,1.);
#4090=VECTOR('',#14473,1.);
#4091=VECTOR('',#14476,1.);
#4092=VECTOR('',#14477,1.);
#4093=VECTOR('',#14486,0.6);
#4094=VERTEX_POINT('',#14564);
#4095=VERTEX_POINT('',#14565);
#4096=VERTEX_POINT('',#14567);
#4097=VERTEX_POINT('',#14590);
#4098=VERTEX_POINT('',#14592);
#4099=VERTEX_POINT('',#14600);
#4100=VERTEX_POINT('',#14626);
#4101=VERTEX_POINT('',#14627);
#4102=VERTEX_POINT('',#14677);
#4103=VERTEX_POINT('',#14678);
#4104=VERTEX_POINT('',#14725);
#4105=VERTEX_POINT('',#14726);
#4106=VERTEX_POINT('',#14773);
#4107=VERTEX_POINT('',#14774);
#4108=VERTEX_POINT('',#14824);
#4109=VERTEX_POINT('',#14825);
#4110=VERTEX_POINT('',#14872);
#4111=VERTEX_POINT('',#14873);
#4112=VERTEX_POINT('',#14920);
#4113=VERTEX_POINT('',#14921);
#4114=VERTEX_POINT('',#14971);
#4115=VERTEX_POINT('',#14972);
#4116=VERTEX_POINT('',#15022);
#4117=VERTEX_POINT('',#15023);
#4118=VERTEX_POINT('',#15070);
#4119=VERTEX_POINT('',#15071);
#4120=VERTEX_POINT('',#15121);
#4121=VERTEX_POINT('',#15122);
#4122=VERTEX_POINT('',#15124);
#4123=VERTEX_POINT('',#15138);
#4124=VERTEX_POINT('',#15160);
#4125=VERTEX_POINT('',#15161);
#4126=VERTEX_POINT('',#15163);
#4127=VERTEX_POINT('',#15171);
#4128=VERTEX_POINT('',#15182);
#4129=VERTEX_POINT('',#15183);
#4130=VERTEX_POINT('',#15206);
#4131=VERTEX_POINT('',#15207);
#4132=VERTEX_POINT('',#15231);
#4133=VERTEX_POINT('',#15232);
#4134=VERTEX_POINT('',#15256);
#4135=VERTEX_POINT('',#15257);
#4136=VERTEX_POINT('',#15280);
#4137=VERTEX_POINT('',#15281);
#4138=VERTEX_POINT('',#15305);
#4139=VERTEX_POINT('',#15306);
#4140=VERTEX_POINT('',#15329);
#4141=VERTEX_POINT('',#15330);
#4142=VERTEX_POINT('',#15354);
#4143=VERTEX_POINT('',#15355);
#4144=VERTEX_POINT('',#15378);
#4145=VERTEX_POINT('',#15379);
#4146=VERTEX_POINT('',#15403);
#4147=VERTEX_POINT('',#15404);
#4148=VERTEX_POINT('',#15428);
#4149=VERTEX_POINT('',#15429);
#4150=VERTEX_POINT('',#15452);
#4151=VERTEX_POINT('',#15453);
#4152=VERTEX_POINT('',#15455);
#4153=VERTEX_POINT('',#15461);
#4154=VERTEX_POINT('',#15469);
#4155=VERTEX_POINT('',#15470);
#4156=VERTEX_POINT('',#15472);
#4157=VERTEX_POINT('',#15495);
#4158=VERTEX_POINT('',#15497);
#4159=VERTEX_POINT('',#15505);
#4160=VERTEX_POINT('',#15531);
#4161=VERTEX_POINT('',#15532);
#4162=VERTEX_POINT('',#15582);
#4163=VERTEX_POINT('',#15583);
#4164=VERTEX_POINT('',#15630);
#4165=VERTEX_POINT('',#15631);
#4166=VERTEX_POINT('',#15678);
#4167=VERTEX_POINT('',#15679);
#4168=VERTEX_POINT('',#15729);
#4169=VERTEX_POINT('',#15730);
#4170=VERTEX_POINT('',#15777);
#4171=VERTEX_POINT('',#15778);
#4172=VERTEX_POINT('',#15825);
#4173=VERTEX_POINT('',#15826);
#4174=VERTEX_POINT('',#15876);
#4175=VERTEX_POINT('',#15877);
#4176=VERTEX_POINT('',#15927);
#4177=VERTEX_POINT('',#15928);
#4178=VERTEX_POINT('',#15975);
#4179=VERTEX_POINT('',#15976);
#4180=VERTEX_POINT('',#16026);
#4181=VERTEX_POINT('',#16027);
#4182=VERTEX_POINT('',#16029);
#4183=VERTEX_POINT('',#16043);
#4184=VERTEX_POINT('',#16065);
#4185=VERTEX_POINT('',#16066);
#4186=VERTEX_POINT('',#16068);
#4187=VERTEX_POINT('',#16076);
#4188=VERTEX_POINT('',#16087);
#4189=VERTEX_POINT('',#16088);
#4190=VERTEX_POINT('',#16111);
#4191=VERTEX_POINT('',#16112);
#4192=VERTEX_POINT('',#16136);
#4193=VERTEX_POINT('',#16137);
#4194=VERTEX_POINT('',#16161);
#4195=VERTEX_POINT('',#16162);
#4196=VERTEX_POINT('',#16185);
#4197=VERTEX_POINT('',#16186);
#4198=VERTEX_POINT('',#16210);
#4199=VERTEX_POINT('',#16211);
#4200=VERTEX_POINT('',#16234);
#4201=VERTEX_POINT('',#16235);
#4202=VERTEX_POINT('',#16259);
#4203=VERTEX_POINT('',#16260);
#4204=VERTEX_POINT('',#16283);
#4205=VERTEX_POINT('',#16284);
#4206=VERTEX_POINT('',#16308);
#4207=VERTEX_POINT('',#16309);
#4208=VERTEX_POINT('',#16333);
#4209=VERTEX_POINT('',#16334);
#4210=VERTEX_POINT('',#16357);
#4211=VERTEX_POINT('',#16358);
#4212=VERTEX_POINT('',#16360);
#4213=VERTEX_POINT('',#16366);
#4214=VERTEX_POINT('',#16374);
#4215=VERTEX_POINT('',#16375);
#4216=VERTEX_POINT('',#16377);
#4217=VERTEX_POINT('',#16400);
#4218=VERTEX_POINT('',#16402);
#4219=VERTEX_POINT('',#16410);
#4220=VERTEX_POINT('',#16436);
#4221=VERTEX_POINT('',#16437);
#4222=VERTEX_POINT('',#16487);
#4223=VERTEX_POINT('',#16488);
#4224=VERTEX_POINT('',#16535);
#4225=VERTEX_POINT('',#16536);
#4226=VERTEX_POINT('',#16583);
#4227=VERTEX_POINT('',#16584);
#4228=VERTEX_POINT('',#16634);
#4229=VERTEX_POINT('',#16635);
#4230=VERTEX_POINT('',#16682);
#4231=VERTEX_POINT('',#16683);
#4232=VERTEX_POINT('',#16730);
#4233=VERTEX_POINT('',#16731);
#4234=VERTEX_POINT('',#16781);
#4235=VERTEX_POINT('',#16782);
#4236=VERTEX_POINT('',#16832);
#4237=VERTEX_POINT('',#16833);
#4238=VERTEX_POINT('',#16880);
#4239=VERTEX_POINT('',#16881);
#4240=VERTEX_POINT('',#16931);
#4241=VERTEX_POINT('',#16932);
#4242=VERTEX_POINT('',#16934);
#4243=VERTEX_POINT('',#16948);
#4244=VERTEX_POINT('',#16970);
#4245=VERTEX_POINT('',#16971);
#4246=VERTEX_POINT('',#16973);
#4247=VERTEX_POINT('',#16981);
#4248=VERTEX_POINT('',#16992);
#4249=VERTEX_POINT('',#16993);
#4250=VERTEX_POINT('',#17016);
#4251=VERTEX_POINT('',#17017);
#4252=VERTEX_POINT('',#17041);
#4253=VERTEX_POINT('',#17042);
#4254=VERTEX_POINT('',#17066);
#4255=VERTEX_POINT('',#17067);
#4256=VERTEX_POINT('',#17090);
#4257=VERTEX_POINT('',#17091);
#4258=VERTEX_POINT('',#17115);
#4259=VERTEX_POINT('',#17116);
#4260=VERTEX_POINT('',#17139);
#4261=VERTEX_POINT('',#17140);
#4262=VERTEX_POINT('',#17164);
#4263=VERTEX_POINT('',#17165);
#4264=VERTEX_POINT('',#17188);
#4265=VERTEX_POINT('',#17189);
#4266=VERTEX_POINT('',#17213);
#4267=VERTEX_POINT('',#17214);
#4268=VERTEX_POINT('',#17238);
#4269=VERTEX_POINT('',#17239);
#4270=VERTEX_POINT('',#17262);
#4271=VERTEX_POINT('',#17263);
#4272=VERTEX_POINT('',#17265);
#4273=VERTEX_POINT('',#17271);
#4274=VERTEX_POINT('',#17279);
#4275=VERTEX_POINT('',#17280);
#4276=VERTEX_POINT('',#17282);
#4277=VERTEX_POINT('',#17305);
#4278=VERTEX_POINT('',#17307);
#4279=VERTEX_POINT('',#17315);
#4280=VERTEX_POINT('',#17341);
#4281=VERTEX_POINT('',#17342);
#4282=VERTEX_POINT('',#17392);
#4283=VERTEX_POINT('',#17393);
#4284=VERTEX_POINT('',#17440);
#4285=VERTEX_POINT('',#17441);
#4286=VERTEX_POINT('',#17488);
#4287=VERTEX_POINT('',#17489);
#4288=VERTEX_POINT('',#17539);
#4289=VERTEX_POINT('',#17540);
#4290=VERTEX_POINT('',#17587);
#4291=VERTEX_POINT('',#17588);
#4292=VERTEX_POINT('',#17635);
#4293=VERTEX_POINT('',#17636);
#4294=VERTEX_POINT('',#17686);
#4295=VERTEX_POINT('',#17687);
#4296=VERTEX_POINT('',#17737);
#4297=VERTEX_POINT('',#17738);
#4298=VERTEX_POINT('',#17785);
#4299=VERTEX_POINT('',#17786);
#4300=VERTEX_POINT('',#17836);
#4301=VERTEX_POINT('',#17837);
#4302=VERTEX_POINT('',#17839);
#4303=VERTEX_POINT('',#17853);
#4304=VERTEX_POINT('',#17875);
#4305=VERTEX_POINT('',#17876);
#4306=VERTEX_POINT('',#17878);
#4307=VERTEX_POINT('',#17886);
#4308=VERTEX_POINT('',#17897);
#4309=VERTEX_POINT('',#17898);
#4310=VERTEX_POINT('',#17921);
#4311=VERTEX_POINT('',#17922);
#4312=VERTEX_POINT('',#17946);
#4313=VERTEX_POINT('',#17947);
#4314=VERTEX_POINT('',#17971);
#4315=VERTEX_POINT('',#17972);
#4316=VERTEX_POINT('',#17995);
#4317=VERTEX_POINT('',#17996);
#4318=VERTEX_POINT('',#18020);
#4319=VERTEX_POINT('',#18021);
#4320=VERTEX_POINT('',#18044);
#4321=VERTEX_POINT('',#18045);
#4322=VERTEX_POINT('',#18069);
#4323=VERTEX_POINT('',#18070);
#4324=VERTEX_POINT('',#18093);
#4325=VERTEX_POINT('',#18094);
#4326=VERTEX_POINT('',#18118);
#4327=VERTEX_POINT('',#18119);
#4328=VERTEX_POINT('',#18143);
#4329=VERTEX_POINT('',#18144);
#4330=VERTEX_POINT('',#18167);
#4331=VERTEX_POINT('',#18168);
#4332=VERTEX_POINT('',#18170);
#4333=VERTEX_POINT('',#18176);
#4334=VERTEX_POINT('',#18184);
#4335=VERTEX_POINT('',#18186);
#4336=VERTEX_POINT('',#18190);
#4337=VERTEX_POINT('',#18192);
#4338=VERTEX_POINT('',#18195);
#4339=VERTEX_POINT('',#18199);
#4340=VERTEX_POINT('',#18203);
#4341=VERTEX_POINT('',#18205);
#4342=VERTEX_POINT('',#18208);
#4343=VERTEX_POINT('',#18212);
#4344=VERTEX_POINT('',#22112);
#4345=VERTEX_POINT('',#22114);
#4346=VERTEX_POINT('',#22118);
#4347=VERTEX_POINT('',#22120);
#4348=VERTEX_POINT('',#22124);
#4349=VERTEX_POINT('',#22125);
#4350=VERTEX_POINT('',#22127);
#4351=VERTEX_POINT('',#22129);
#4352=VERTEX_POINT('',#22133);
#4353=VERTEX_POINT('',#22135);
#4354=VERTEX_POINT('',#22139);
#4355=VERTEX_POINT('',#22141);
#4356=VERTEX_POINT('',#22147);
#4357=VERTEX_POINT('',#22148);
#4358=VERTEX_POINT('',#22150);
#4359=VERTEX_POINT('',#22152);
#4360=VERTEX_POINT('',#22156);
#4361=VERTEX_POINT('',#22157);
#4362=VERTEX_POINT('',#22159);
#4363=VERTEX_POINT('',#22161);
#4364=VERTEX_POINT('',#22170);
#4365=VERTEX_POINT('',#22172);
#4366=VERTEX_POINT('',#22176);
#4367=VERTEX_POINT('',#22178);
#4368=VERTEX_POINT('',#22183);
#4369=VERTEX_POINT('',#22184);
#4370=VERTEX_POINT('',#22186);
#4371=VERTEX_POINT('',#22188);
#4372=VERTEX_POINT('',#22190);
#4373=VERTEX_POINT('',#22192);
#4374=VERTEX_POINT('',#22194);
#4375=VERTEX_POINT('',#22196);
#4376=VERTEX_POINT('',#22200);
#4377=VERTEX_POINT('',#22202);
#4378=VERTEX_POINT('',#22206);
#4379=VERTEX_POINT('',#22210);
#4380=VERTEX_POINT('',#22214);
#4381=VERTEX_POINT('',#22218);
#4382=VERTEX_POINT('',#22220);
#4383=VERTEX_POINT('',#22225);
#4384=VERTEX_POINT('',#22233);
#4385=VERTEX_POINT('',#22234);
#4386=VERTEX_POINT('',#22236);
#4387=VERTEX_POINT('',#22238);
#4388=VERTEX_POINT('',#22243);
#4389=VERTEX_POINT('',#22245);
#4390=VERTEX_POINT('',#22249);
#4391=VERTEX_POINT('',#22251);
#4392=VERTEX_POINT('',#22262);
#4393=VERTEX_POINT('',#22263);
#4394=VERTEX_POINT('',#22265);
#4395=VERTEX_POINT('',#22285);
#4396=VERTEX_POINT('',#22319);
#4397=VERTEX_POINT('',#22320);
#4398=VERTEX_POINT('',#22406);
#4399=VERTEX_POINT('',#22407);
#4400=VERTEX_POINT('',#22409);
#4401=VERTEX_POINT('',#22435);
#4402=VERTEX_POINT('',#22475);
#4403=VERTEX_POINT('',#22476);
#4404=VERTEX_POINT('',#22478);
#4405=VERTEX_POINT('',#22498);
#4406=VERTEX_POINT('',#22532);
#4407=VERTEX_POINT('',#22533);
#4408=VERTEX_POINT('',#22619);
#4409=VERTEX_POINT('',#22620);
#4410=VERTEX_POINT('',#22622);
#4411=VERTEX_POINT('',#22648);
#4412=VERTEX_POINT('',#22688);
#4413=VERTEX_POINT('',#22689);
#4414=VERTEX_POINT('',#22691);
#4415=VERTEX_POINT('',#22696);
#4416=VERTEX_POINT('',#22704);
#4417=VERTEX_POINT('',#22705);
#4418=VERTEX_POINT('',#22742);
#4419=VERTEX_POINT('',#22743);
#4420=VERTEX_POINT('',#22778);
#4421=VERTEX_POINT('',#22779);
#4422=VERTEX_POINT('',#22781);
#4423=VERTEX_POINT('',#22788);
#4424=VERTEX_POINT('',#22798);
#4425=VERTEX_POINT('',#22799);
#4426=VERTEX_POINT('',#22801);
#4427=VERTEX_POINT('',#22806);
#4428=VERTEX_POINT('',#22814);
#4429=VERTEX_POINT('',#22815);
#4430=VERTEX_POINT('',#22852);
#4431=VERTEX_POINT('',#22853);
#4432=VERTEX_POINT('',#22888);
#4433=VERTEX_POINT('',#22889);
#4434=VERTEX_POINT('',#22891);
#4435=VERTEX_POINT('',#22898);
#4436=VERTEX_POINT('',#22908);
#4437=VERTEX_POINT('',#22909);
#4438=VERTEX_POINT('',#22911);
#4439=VERTEX_POINT('',#22915);
#4440=VERTEX_POINT('',#22916);
#4441=VERTEX_POINT('',#22918);
#4442=VERTEX_POINT('',#22922);
#4443=VERTEX_POINT('',#22923);
#4444=VERTEX_POINT('',#22925);
#4445=VERTEX_POINT('',#22927);
#4446=VERTEX_POINT('',#22931);
#4447=VERTEX_POINT('',#22932);
#4448=VERTEX_POINT('',#22934);
#4449=VERTEX_POINT('',#22936);
#4450=VERTEX_POINT('',#22940);
#4451=VERTEX_POINT('',#22944);
#4452=VERTEX_POINT('',#22946);
#4453=VERTEX_POINT('',#22950);
#4454=VERTEX_POINT('',#22952);
#4455=VERTEX_POINT('',#22956);
#4456=VERTEX_POINT('',#22964);
#4457=VERTEX_POINT('',#24556);
#4458=VERTEX_POINT('',#24559);
#4459=VERTEX_POINT('',#24563);
#4460=VERTEX_POINT('',#24566);
#4461=VERTEX_POINT('',#24568);
#4462=VERTEX_POINT('',#24606);
#4463=VERTEX_POINT('',#24607);
#4464=VERTEX_POINT('',#24623);
#4465=VERTEX_POINT('',#24636);
#4466=VERTEX_POINT('',#24643);
#4467=VERTEX_POINT('',#24644);
#4468=VERTEX_POINT('',#24646);
#4469=VERTEX_POINT('',#24648);
#4470=VERTEX_POINT('',#24651);
#4471=VERTEX_POINT('',#24653);
#4472=VERTEX_POINT('',#24655);
#4473=VERTEX_POINT('',#24657);
#4474=VERTEX_POINT('',#24659);
#4475=VERTEX_POINT('',#24661);
#4476=VERTEX_POINT('',#24663);
#4477=VERTEX_POINT('',#24665);
#4478=VERTEX_POINT('',#24684);
#4479=VERTEX_POINT('',#24687);
#4480=VERTEX_POINT('',#24691);
#4481=VERTEX_POINT('',#24694);
#4482=VERTEX_POINT('',#24696);
#4483=VERTEX_POINT('',#24707);
#4484=VERTEX_POINT('',#24718);
#4485=VERTEX_POINT('',#24756);
#4486=VERTEX_POINT('',#24760);
#4487=VERTEX_POINT('',#24764);
#4488=VERTEX_POINT('',#24768);
#4489=VERTEX_POINT('',#24773);
#4490=VERTEX_POINT('',#24777);
#4491=VERTEX_POINT('',#24778);
#4492=VERTEX_POINT('',#24783);
#4493=VERTEX_POINT('',#24787);
#4494=VERTEX_POINT('',#24795);
#4495=VERTEX_POINT('',#24797);
#4496=VERTEX_POINT('',#24800);
#4497=VERTEX_POINT('',#24804);
#4498=VERTEX_POINT('',#24807);
#4499=VERTEX_POINT('',#24811);
#4500=VERTEX_POINT('',#24817);
#4501=VERTEX_POINT('',#24818);
#4502=VERTEX_POINT('',#24820);
#4503=VERTEX_POINT('',#24843);
#4504=VERTEX_POINT('',#24845);
#4505=VERTEX_POINT('',#24853);
#4506=VERTEX_POINT('',#24879);
#4507=VERTEX_POINT('',#24880);
#4508=VERTEX_POINT('',#24930);
#4509=VERTEX_POINT('',#24931);
#4510=VERTEX_POINT('',#24978);
#4511=VERTEX_POINT('',#24979);
#4512=VERTEX_POINT('',#25026);
#4513=VERTEX_POINT('',#25027);
#4514=VERTEX_POINT('',#25077);
#4515=VERTEX_POINT('',#25078);
#4516=VERTEX_POINT('',#25125);
#4517=VERTEX_POINT('',#25126);
#4518=VERTEX_POINT('',#25173);
#4519=VERTEX_POINT('',#25174);
#4520=VERTEX_POINT('',#25224);
#4521=VERTEX_POINT('',#25225);
#4522=VERTEX_POINT('',#25275);
#4523=VERTEX_POINT('',#25276);
#4524=VERTEX_POINT('',#25323);
#4525=VERTEX_POINT('',#25324);
#4526=VERTEX_POINT('',#25374);
#4527=VERTEX_POINT('',#25375);
#4528=VERTEX_POINT('',#25377);
#4529=VERTEX_POINT('',#25391);
#4530=VERTEX_POINT('',#25413);
#4531=VERTEX_POINT('',#25414);
#4532=VERTEX_POINT('',#25416);
#4533=VERTEX_POINT('',#25424);
#4534=VERTEX_POINT('',#25435);
#4535=VERTEX_POINT('',#25436);
#4536=VERTEX_POINT('',#25459);
#4537=VERTEX_POINT('',#25460);
#4538=VERTEX_POINT('',#25484);
#4539=VERTEX_POINT('',#25485);
#4540=VERTEX_POINT('',#25509);
#4541=VERTEX_POINT('',#25510);
#4542=VERTEX_POINT('',#25533);
#4543=VERTEX_POINT('',#25534);
#4544=VERTEX_POINT('',#25558);
#4545=VERTEX_POINT('',#25559);
#4546=VERTEX_POINT('',#25582);
#4547=VERTEX_POINT('',#25583);
#4548=VERTEX_POINT('',#25607);
#4549=VERTEX_POINT('',#25608);
#4550=VERTEX_POINT('',#25631);
#4551=VERTEX_POINT('',#25632);
#4552=VERTEX_POINT('',#25656);
#4553=VERTEX_POINT('',#25657);
#4554=VERTEX_POINT('',#25681);
#4555=VERTEX_POINT('',#25682);
#4556=VERTEX_POINT('',#25705);
#4557=VERTEX_POINT('',#25706);
#4558=VERTEX_POINT('',#25708);
#4559=VERTEX_POINT('',#25714);
#4560=VERTEX_POINT('',#25722);
#4561=VERTEX_POINT('',#25723);
#4562=VERTEX_POINT('',#25725);
#4563=VERTEX_POINT('',#25730);
#4564=VERTEX_POINT('',#25743);
#4565=VERTEX_POINT('',#25744);
#4566=VERTEX_POINT('',#25794);
#4567=VERTEX_POINT('',#25795);
#4568=VERTEX_POINT('',#25845);
#4569=VERTEX_POINT('',#25846);
#4570=VERTEX_POINT('',#25893);
#4571=VERTEX_POINT('',#25894);
#4572=VERTEX_POINT('',#25944);
#4573=VERTEX_POINT('',#25945);
#4574=VERTEX_POINT('',#25995);
#4575=VERTEX_POINT('',#25996);
#4576=VERTEX_POINT('',#26043);
#4577=VERTEX_POINT('',#26044);
#4578=VERTEX_POINT('',#26046);
#4579=VERTEX_POINT('',#26060);
#4580=VERTEX_POINT('',#26082);
#4581=VERTEX_POINT('',#26083);
#4582=VERTEX_POINT('',#26085);
#4583=VERTEX_POINT('',#26090);
#4584=VERTEX_POINT('',#26103);
#4585=VERTEX_POINT('',#26104);
#4586=VERTEX_POINT('',#26154);
#4587=VERTEX_POINT('',#26155);
#4588=VERTEX_POINT('',#26205);
#4589=VERTEX_POINT('',#26206);
#4590=VERTEX_POINT('',#26253);
#4591=VERTEX_POINT('',#26254);
#4592=VERTEX_POINT('',#26304);
#4593=VERTEX_POINT('',#26305);
#4594=VERTEX_POINT('',#26355);
#4595=VERTEX_POINT('',#26356);
#4596=VERTEX_POINT('',#26403);
#4597=VERTEX_POINT('',#26404);
#4598=VERTEX_POINT('',#26406);
#4599=VERTEX_POINT('',#26420);
#4600=VERTEX_POINT('',#26442);
#4601=VERTEX_POINT('',#26443);
#4602=VERTEX_POINT('',#26445);
#4603=VERTEX_POINT('',#26454);
#4604=VERTEX_POINT('',#26466);
#4605=VERTEX_POINT('',#26467);
#4606=VERTEX_POINT('',#26490);
#4607=VERTEX_POINT('',#26491);
#4608=VERTEX_POINT('',#26515);
#4609=VERTEX_POINT('',#26516);
#4610=VERTEX_POINT('',#26540);
#4611=VERTEX_POINT('',#26541);
#4612=VERTEX_POINT('',#26564);
#4613=VERTEX_POINT('',#26565);
#4614=VERTEX_POINT('',#26589);
#4615=VERTEX_POINT('',#26590);
#4616=VERTEX_POINT('',#26614);
#4617=VERTEX_POINT('',#26615);
#4618=VERTEX_POINT('',#26617);
#4619=VERTEX_POINT('',#26623);
#4620=VERTEX_POINT('',#26631);
#4621=VERTEX_POINT('',#26632);
#4622=VERTEX_POINT('',#26634);
#4623=VERTEX_POINT('',#26643);
#4624=VERTEX_POINT('',#26655);
#4625=VERTEX_POINT('',#26656);
#4626=VERTEX_POINT('',#26679);
#4627=VERTEX_POINT('',#26680);
#4628=VERTEX_POINT('',#26704);
#4629=VERTEX_POINT('',#26705);
#4630=VERTEX_POINT('',#26729);
#4631=VERTEX_POINT('',#26730);
#4632=VERTEX_POINT('',#26753);
#4633=VERTEX_POINT('',#26754);
#4634=VERTEX_POINT('',#26778);
#4635=VERTEX_POINT('',#26779);
#4636=VERTEX_POINT('',#26803);
#4637=VERTEX_POINT('',#26804);
#4638=VERTEX_POINT('',#26806);
#4639=VERTEX_POINT('',#26812);
#4640=VERTEX_POINT('',#27542);
#4641=VERTEX_POINT('',#27543);
#4642=VERTEX_POINT('',#27545);
#4643=VERTEX_POINT('',#27547);
#4644=VERTEX_POINT('',#27549);
#4645=VERTEX_POINT('',#27551);
#4646=VERTEX_POINT('',#29253);
#4647=VERTEX_POINT('',#29255);
#4648=VERTEX_POINT('',#29259);
#4649=VERTEX_POINT('',#29263);
#4650=VERTEX_POINT('',#29267);
#4651=VERTEX_POINT('',#29271);
#4652=VERTEX_POINT('',#29273);
#4653=VERTEX_POINT('',#29276);
#4654=VERTEX_POINT('',#29278);
#4655=VERTEX_POINT('',#29285);
#4656=VERTEX_POINT('',#29287);
#4657=VERTEX_POINT('',#29291);
#4658=VERTEX_POINT('',#29293);
#4659=VERTEX_POINT('',#29299);
#4660=VERTEX_POINT('',#29301);
#4661=VERTEX_POINT('',#29309);
#4662=VERTEX_POINT('',#29316);
#4663=VERTEX_POINT('',#29318);
#4664=VERTEX_POINT('',#29322);
#4665=VERTEX_POINT('',#29326);
#4666=VERTEX_POINT('',#29329);
#4667=VERTEX_POINT('',#29333);
#4668=VERTEX_POINT('',#29336);
#4669=VERTEX_POINT('',#29338);
#4670=VERTEX_POINT('',#29343);
#4671=VERTEX_POINT('',#29345);
#4672=VERTEX_POINT('',#29350);
#4673=VERTEX_POINT('',#29354);
#4674=VERTEX_POINT('',#29360);
#4675=VERTEX_POINT('',#29362);
#4676=VERTEX_POINT('',#29366);
#4677=VERTEX_POINT('',#29368);
#4678=VERTEX_POINT('',#29372);
#4679=VERTEX_POINT('',#29373);
#4680=VERTEX_POINT('',#29375);
#4681=VERTEX_POINT('',#29377);
#4682=VERTEX_POINT('',#29381);
#4683=VERTEX_POINT('',#29383);
#4684=VERTEX_POINT('',#29387);
#4685=VERTEX_POINT('',#29389);
#4686=VERTEX_POINT('',#29808);
#4687=VERTEX_POINT('',#29810);
#4688=VERTEX_POINT('',#29857);
#4689=VERTEX_POINT('',#29858);
#4690=VERTEX_POINT('',#29860);
#4691=VERTEX_POINT('',#29883);
#4692=VERTEX_POINT('',#29885);
#4693=VERTEX_POINT('',#29893);
#4694=VERTEX_POINT('',#29919);
#4695=VERTEX_POINT('',#29920);
#4696=VERTEX_POINT('',#29970);
#4697=VERTEX_POINT('',#29971);
#4698=VERTEX_POINT('',#30018);
#4699=VERTEX_POINT('',#30019);
#4700=VERTEX_POINT('',#30066);
#4701=VERTEX_POINT('',#30067);
#4702=VERTEX_POINT('',#30117);
#4703=VERTEX_POINT('',#30118);
#4704=VERTEX_POINT('',#30165);
#4705=VERTEX_POINT('',#30166);
#4706=VERTEX_POINT('',#30213);
#4707=VERTEX_POINT('',#30214);
#4708=VERTEX_POINT('',#30264);
#4709=VERTEX_POINT('',#30265);
#4710=VERTEX_POINT('',#30315);
#4711=VERTEX_POINT('',#30316);
#4712=VERTEX_POINT('',#30363);
#4713=VERTEX_POINT('',#30364);
#4714=VERTEX_POINT('',#30414);
#4715=VERTEX_POINT('',#30415);
#4716=VERTEX_POINT('',#30417);
#4717=VERTEX_POINT('',#30431);
#4718=VERTEX_POINT('',#30453);
#4719=VERTEX_POINT('',#30454);
#4720=VERTEX_POINT('',#30456);
#4721=VERTEX_POINT('',#30464);
#4722=VERTEX_POINT('',#30475);
#4723=VERTEX_POINT('',#30476);
#4724=VERTEX_POINT('',#30499);
#4725=VERTEX_POINT('',#30500);
#4726=VERTEX_POINT('',#30524);
#4727=VERTEX_POINT('',#30525);
#4728=VERTEX_POINT('',#30549);
#4729=VERTEX_POINT('',#30550);
#4730=VERTEX_POINT('',#30573);
#4731=VERTEX_POINT('',#30574);
#4732=VERTEX_POINT('',#30598);
#4733=VERTEX_POINT('',#30599);
#4734=VERTEX_POINT('',#30622);
#4735=VERTEX_POINT('',#30623);
#4736=VERTEX_POINT('',#30647);
#4737=VERTEX_POINT('',#30648);
#4738=VERTEX_POINT('',#30671);
#4739=VERTEX_POINT('',#30672);
#4740=VERTEX_POINT('',#30696);
#4741=VERTEX_POINT('',#30697);
#4742=VERTEX_POINT('',#30721);
#4743=VERTEX_POINT('',#30722);
#4744=VERTEX_POINT('',#30745);
#4745=VERTEX_POINT('',#30746);
#4746=VERTEX_POINT('',#30748);
#4747=VERTEX_POINT('',#30754);
#4748=VERTEX_POINT('',#30762);
#4749=VERTEX_POINT('',#30763);
#4750=VERTEX_POINT('',#30765);
#4751=VERTEX_POINT('',#30770);
#4752=VERTEX_POINT('',#30772);
#4753=VERTEX_POINT('',#30775);
#4754=VERTEX_POINT('',#30788);
#4755=VERTEX_POINT('',#30789);
#4756=VERTEX_POINT('',#30839);
#4757=VERTEX_POINT('',#30840);
#4758=VERTEX_POINT('',#30890);
#4759=VERTEX_POINT('',#30891);
#4760=VERTEX_POINT('',#30938);
#4761=VERTEX_POINT('',#30939);
#4762=VERTEX_POINT('',#30989);
#4763=VERTEX_POINT('',#30990);
#4764=VERTEX_POINT('',#31040);
#4765=VERTEX_POINT('',#31041);
#4766=VERTEX_POINT('',#31088);
#4767=VERTEX_POINT('',#31089);
#4768=VERTEX_POINT('',#31139);
#4769=VERTEX_POINT('',#31140);
#4770=VERTEX_POINT('',#31190);
#4771=VERTEX_POINT('',#31191);
#4772=VERTEX_POINT('',#31238);
#4773=VERTEX_POINT('',#31239);
#4774=VERTEX_POINT('',#31289);
#4775=VERTEX_POINT('',#31290);
#4776=VERTEX_POINT('',#31340);
#4777=VERTEX_POINT('',#31341);
#4778=VERTEX_POINT('',#31388);
#4779=VERTEX_POINT('',#31389);
#4780=VERTEX_POINT('',#31439);
#4781=VERTEX_POINT('',#31440);
#4782=VERTEX_POINT('',#31490);
#4783=VERTEX_POINT('',#31491);
#4784=VERTEX_POINT('',#31538);
#4785=VERTEX_POINT('',#31539);
#4786=VERTEX_POINT('',#31589);
#4787=VERTEX_POINT('',#31590);
#4788=VERTEX_POINT('',#31592);
#4789=VERTEX_POINT('',#31606);
#4790=VERTEX_POINT('',#31628);
#4791=VERTEX_POINT('',#31629);
#4792=VERTEX_POINT('',#31631);
#4793=VERTEX_POINT('',#31640);
#4794=VERTEX_POINT('',#31652);
#4795=VERTEX_POINT('',#31653);
#4796=VERTEX_POINT('',#31676);
#4797=VERTEX_POINT('',#31677);
#4798=VERTEX_POINT('',#31701);
#4799=VERTEX_POINT('',#31702);
#4800=VERTEX_POINT('',#31726);
#4801=VERTEX_POINT('',#31727);
#4802=VERTEX_POINT('',#31750);
#4803=VERTEX_POINT('',#31751);
#4804=VERTEX_POINT('',#31775);
#4805=VERTEX_POINT('',#31776);
#4806=VERTEX_POINT('',#31800);
#4807=VERTEX_POINT('',#31801);
#4808=VERTEX_POINT('',#31824);
#4809=VERTEX_POINT('',#31825);
#4810=VERTEX_POINT('',#31849);
#4811=VERTEX_POINT('',#31850);
#4812=VERTEX_POINT('',#31874);
#4813=VERTEX_POINT('',#31875);
#4814=VERTEX_POINT('',#31898);
#4815=VERTEX_POINT('',#31899);
#4816=VERTEX_POINT('',#31923);
#4817=VERTEX_POINT('',#31924);
#4818=VERTEX_POINT('',#31948);
#4819=VERTEX_POINT('',#31949);
#4820=VERTEX_POINT('',#31972);
#4821=VERTEX_POINT('',#31973);
#4822=VERTEX_POINT('',#31997);
#4823=VERTEX_POINT('',#31998);
#4824=VERTEX_POINT('',#32022);
#4825=VERTEX_POINT('',#32023);
#4826=VERTEX_POINT('',#32046);
#4827=VERTEX_POINT('',#32047);
#4828=VERTEX_POINT('',#32049);
#4829=VERTEX_POINT('',#32055);
#4830=VERTEX_POINT('',#34266);
#4831=VERTEX_POINT('',#34267);
#4832=VERTEX_POINT('',#34269);
#4833=VERTEX_POINT('',#34271);
#4834=VERTEX_POINT('',#34275);
#4835=VERTEX_POINT('',#34277);
#4836=VERTEX_POINT('',#34281);
#4837=VERTEX_POINT('',#34283);
#4838=VERTEX_POINT('',#34293);
#4839=VERTEX_POINT('',#34294);
#4840=VERTEX_POINT('',#34296);
#4841=VERTEX_POINT('',#34301);
#4842=VERTEX_POINT('',#34303);
#4843=VERTEX_POINT('',#34306);
#4844=VERTEX_POINT('',#34319);
#4845=VERTEX_POINT('',#34320);
#4846=VERTEX_POINT('',#34370);
#4847=VERTEX_POINT('',#34371);
#4848=VERTEX_POINT('',#34421);
#4849=VERTEX_POINT('',#34422);
#4850=VERTEX_POINT('',#34469);
#4851=VERTEX_POINT('',#34470);
#4852=VERTEX_POINT('',#34517);
#4853=VERTEX_POINT('',#34518);
#4854=VERTEX_POINT('',#34568);
#4855=VERTEX_POINT('',#34569);
#4856=VERTEX_POINT('',#34619);
#4857=VERTEX_POINT('',#34620);
#4858=VERTEX_POINT('',#34667);
#4859=VERTEX_POINT('',#34668);
#4860=VERTEX_POINT('',#34718);
#4861=VERTEX_POINT('',#34719);
#4862=VERTEX_POINT('',#34721);
#4863=VERTEX_POINT('',#34735);
#4864=VERTEX_POINT('',#34757);
#4865=VERTEX_POINT('',#34758);
#4866=VERTEX_POINT('',#34760);
#4867=VERTEX_POINT('',#34769);
#4868=VERTEX_POINT('',#34781);
#4869=VERTEX_POINT('',#34782);
#4870=VERTEX_POINT('',#34805);
#4871=VERTEX_POINT('',#34806);
#4872=VERTEX_POINT('',#34830);
#4873=VERTEX_POINT('',#34831);
#4874=VERTEX_POINT('',#34854);
#4875=VERTEX_POINT('',#34855);
#4876=VERTEX_POINT('',#34879);
#4877=VERTEX_POINT('',#34880);
#4878=VERTEX_POINT('',#34903);
#4879=VERTEX_POINT('',#34904);
#4880=VERTEX_POINT('',#34928);
#4881=VERTEX_POINT('',#34929);
#4882=VERTEX_POINT('',#34953);
#4883=VERTEX_POINT('',#34954);
#4884=VERTEX_POINT('',#34977);
#4885=VERTEX_POINT('',#34978);
#4886=VERTEX_POINT('',#34980);
#4887=VERTEX_POINT('',#34986);
#4888=VERTEX_POINT('',#35815);
#4889=VERTEX_POINT('',#35817);
#4890=VERTEX_POINT('',#35821);
#4891=VERTEX_POINT('',#35822);
#4892=VERTEX_POINT('',#35824);
#4893=VERTEX_POINT('',#35826);
#4894=VERTEX_POINT('',#35830);
#4895=VERTEX_POINT('',#35831);
#4896=VERTEX_POINT('',#35836);
#4897=VERTEX_POINT('',#35838);
#4898=VERTEX_POINT('',#35840);
#4899=VERTEX_POINT('',#35844);
#4900=VERTEX_POINT('',#35848);
#4901=VERTEX_POINT('',#35850);
#4902=VERTEX_POINT('',#35860);
#4903=VERTEX_POINT('',#35862);
#4904=VERTEX_POINT('',#35866);
#4905=VERTEX_POINT('',#35867);
#4906=VERTEX_POINT('',#35869);
#4907=VERTEX_POINT('',#35871);
#4908=VERTEX_POINT('',#35875);
#4909=VERTEX_POINT('',#35877);
#4910=VERTEX_POINT('',#35881);
#4911=VERTEX_POINT('',#35883);
#4912=VERTEX_POINT('',#35893);
#4913=VERTEX_POINT('',#35894);
#4914=VERTEX_POINT('',#35898);
#4915=VERTEX_POINT('',#35900);
#4916=VERTEX_POINT('',#35903);
#4917=VERTEX_POINT('',#35908);
#4918=VERTEX_POINT('',#36323);
#4919=VERTEX_POINT('',#36325);
#4920=VERTEX_POINT('',#36372);
#4921=VERTEX_POINT('',#36373);
#4922=VERTEX_POINT('',#36375);
#4923=VERTEX_POINT('',#36386);
#4924=VERTEX_POINT('',#36396);
#4925=VERTEX_POINT('',#36397);
#4926=VERTEX_POINT('',#36444);
#4927=VERTEX_POINT('',#36445);
#4928=VERTEX_POINT('',#36492);
#4929=VERTEX_POINT('',#36493);
#4930=VERTEX_POINT('',#36540);
#4931=VERTEX_POINT('',#36541);
#4932=VERTEX_POINT('',#36588);
#4933=VERTEX_POINT('',#36589);
#4934=VERTEX_POINT('',#36636);
#4935=VERTEX_POINT('',#36637);
#4936=VERTEX_POINT('',#36684);
#4937=VERTEX_POINT('',#36685);
#4938=VERTEX_POINT('',#36738);
#4939=VERTEX_POINT('',#36739);
#4940=VERTEX_POINT('',#36786);
#4941=VERTEX_POINT('',#36787);
#4942=VERTEX_POINT('',#36834);
#4943=VERTEX_POINT('',#36835);
#4944=VERTEX_POINT('',#36888);
#4945=VERTEX_POINT('',#36889);
#4946=VERTEX_POINT('',#36936);
#4947=VERTEX_POINT('',#36937);
#4948=VERTEX_POINT('',#36984);
#4949=VERTEX_POINT('',#36985);
#4950=VERTEX_POINT('',#37032);
#4951=VERTEX_POINT('',#37033);
#4952=VERTEX_POINT('',#37083);
#4953=VERTEX_POINT('',#37084);
#4954=VERTEX_POINT('',#37131);
#4955=VERTEX_POINT('',#37132);
#4956=VERTEX_POINT('',#37134);
#4957=VERTEX_POINT('',#37143);
#4958=VERTEX_POINT('',#37153);
#4959=VERTEX_POINT('',#37154);
#4960=VERTEX_POINT('',#37177);
#4961=VERTEX_POINT('',#37178);
#4962=VERTEX_POINT('',#37201);
#4963=VERTEX_POINT('',#37202);
#4964=VERTEX_POINT('',#37227);
#4965=VERTEX_POINT('',#37228);
#4966=VERTEX_POINT('',#37251);
#4967=VERTEX_POINT('',#37252);
#4968=VERTEX_POINT('',#37275);
#4969=VERTEX_POINT('',#37276);
#4970=VERTEX_POINT('',#37300);
#4971=VERTEX_POINT('',#37301);
#4972=VERTEX_POINT('',#37325);
#4973=VERTEX_POINT('',#37326);
#4974=VERTEX_POINT('',#37349);
#4975=VERTEX_POINT('',#37350);
#4976=VERTEX_POINT('',#37374);
#4977=VERTEX_POINT('',#37375);
#4978=VERTEX_POINT('',#37399);
#4979=VERTEX_POINT('',#37400);
#4980=VERTEX_POINT('',#37423);
#4981=VERTEX_POINT('',#37424);
#4982=VERTEX_POINT('',#37447);
#4983=VERTEX_POINT('',#37448);
#4984=VERTEX_POINT('',#37472);
#4985=VERTEX_POINT('',#37473);
#4986=VERTEX_POINT('',#37497);
#4987=VERTEX_POINT('',#37498);
#4988=VERTEX_POINT('',#37521);
#4989=VERTEX_POINT('',#37601);
#4990=VERTEX_POINT('',#37636);
#4991=VERTEX_POINT('',#37702);
#4992=VERTEX_POINT('',#38129);
#4993=VERTEX_POINT('',#38210);
#4994=VERTEX_POINT('',#38723);
#4995=VERTEX_POINT('',#38724);
#4996=VERTEX_POINT('',#38726);
#4997=VERTEX_POINT('',#38728);
#4998=VERTEX_POINT('',#38732);
#4999=VERTEX_POINT('',#38734);
#5000=VERTEX_POINT('',#38738);
#5001=VERTEX_POINT('',#38740);
#5002=VERTEX_POINT('',#38744);
#5003=VERTEX_POINT('',#38746);
#5004=VERTEX_POINT('',#38750);
#5005=VERTEX_POINT('',#38752);
#5006=VERTEX_POINT('',#38760);
#5007=VERTEX_POINT('',#38763);
#5008=VERTEX_POINT('',#38770);
#5009=VERTEX_POINT('',#38771);
#5010=VERTEX_POINT('',#38773);
#5011=VERTEX_POINT('',#38784);
#5012=VERTEX_POINT('',#38794);
#5013=VERTEX_POINT('',#38795);
#5014=VERTEX_POINT('',#38842);
#5015=VERTEX_POINT('',#38843);
#5016=VERTEX_POINT('',#38890);
#5017=VERTEX_POINT('',#38891);
#5018=VERTEX_POINT('',#38938);
#5019=VERTEX_POINT('',#38939);
#5020=VERTEX_POINT('',#38992);
#5021=VERTEX_POINT('',#38993);
#5022=VERTEX_POINT('',#39040);
#5023=VERTEX_POINT('',#39041);
#5024=VERTEX_POINT('',#39088);
#5025=VERTEX_POINT('',#39089);
#5026=VERTEX_POINT('',#39142);
#5027=VERTEX_POINT('',#39143);
#5028=VERTEX_POINT('',#39190);
#5029=VERTEX_POINT('',#39191);
#5030=VERTEX_POINT('',#39238);
#5031=VERTEX_POINT('',#39239);
#5032=VERTEX_POINT('',#39241);
#5033=VERTEX_POINT('',#39252);
#5034=VERTEX_POINT('',#39264);
#5035=VERTEX_POINT('',#39265);
#5036=VERTEX_POINT('',#39288);
#5037=VERTEX_POINT('',#39289);
#5038=VERTEX_POINT('',#39312);
#5039=VERTEX_POINT('',#39313);
#5040=VERTEX_POINT('',#39337);
#5041=VERTEX_POINT('',#39338);
#5042=VERTEX_POINT('',#39362);
#5043=VERTEX_POINT('',#39363);
#5044=VERTEX_POINT('',#39386);
#5045=VERTEX_POINT('',#39387);
#5046=VERTEX_POINT('',#39411);
#5047=VERTEX_POINT('',#39412);
#5048=VERTEX_POINT('',#39436);
#5049=VERTEX_POINT('',#39437);
#5050=VERTEX_POINT('',#39460);
#5051=VERTEX_POINT('',#39461);
#5052=VERTEX_POINT('',#39484);
#5053=VERTEX_POINT('',#39609);
#5054=VERTEX_POINT('',#39647);
#5055=VERTEX_POINT('',#39665);
#5056=VERTEX_POINT('',#39948);
#5057=VERTEX_POINT('',#40026);
#5058=VERTEX_POINT('',#40401);
#5059=VERTEX_POINT('',#40402);
#5060=VERTEX_POINT('',#40404);
#5061=VERTEX_POINT('',#40406);
#5062=VERTEX_POINT('',#40410);
#5063=VERTEX_POINT('',#40412);
#5064=VERTEX_POINT('',#40416);
#5065=VERTEX_POINT('',#40418);
#5066=VERTEX_POINT('',#40422);
#5067=VERTEX_POINT('',#40424);
#5068=VERTEX_POINT('',#40428);
#5069=VERTEX_POINT('',#40430);
#5070=VERTEX_POINT('',#40438);
#5071=VERTEX_POINT('',#40441);
#5072=VERTEX_POINT('',#40448);
#5073=VERTEX_POINT('',#40449);
#5074=VERTEX_POINT('',#40451);
#5075=VERTEX_POINT('',#40462);
#5076=VERTEX_POINT('',#40472);
#5077=VERTEX_POINT('',#40473);
#5078=VERTEX_POINT('',#40520);
#5079=VERTEX_POINT('',#40521);
#5080=VERTEX_POINT('',#40568);
#5081=VERTEX_POINT('',#40569);
#5082=VERTEX_POINT('',#40622);
#5083=VERTEX_POINT('',#40623);
#5084=VERTEX_POINT('',#40670);
#5085=VERTEX_POINT('',#40671);
#5086=VERTEX_POINT('',#40718);
#5087=VERTEX_POINT('',#40719);
#5088=VERTEX_POINT('',#40772);
#5089=VERTEX_POINT('',#40773);
#5090=VERTEX_POINT('',#40820);
#5091=VERTEX_POINT('',#40821);
#5092=VERTEX_POINT('',#40868);
#5093=VERTEX_POINT('',#40869);
#5094=VERTEX_POINT('',#40922);
#5095=VERTEX_POINT('',#40923);
#5096=VERTEX_POINT('',#40970);
#5097=VERTEX_POINT('',#40971);
#5098=VERTEX_POINT('',#41018);
#5099=VERTEX_POINT('',#41019);
#5100=VERTEX_POINT('',#41072);
#5101=VERTEX_POINT('',#41073);
#5102=VERTEX_POINT('',#41120);
#5103=VERTEX_POINT('',#41121);
#5104=VERTEX_POINT('',#41168);
#5105=VERTEX_POINT('',#41169);
#5106=VERTEX_POINT('',#41219);
#5107=VERTEX_POINT('',#41220);
#5108=VERTEX_POINT('',#41267);
#5109=VERTEX_POINT('',#41268);
#5110=VERTEX_POINT('',#41315);
#5111=VERTEX_POINT('',#41316);
#5112=VERTEX_POINT('',#41318);
#5113=VERTEX_POINT('',#41329);
#5114=VERTEX_POINT('',#41341);
#5115=VERTEX_POINT('',#41342);
#5116=VERTEX_POINT('',#41365);
#5117=VERTEX_POINT('',#41366);
#5118=VERTEX_POINT('',#41389);
#5119=VERTEX_POINT('',#41390);
#5120=VERTEX_POINT('',#41415);
#5121=VERTEX_POINT('',#41416);
#5122=VERTEX_POINT('',#41439);
#5123=VERTEX_POINT('',#41440);
#5124=VERTEX_POINT('',#41463);
#5125=VERTEX_POINT('',#41464);
#5126=VERTEX_POINT('',#41488);
#5127=VERTEX_POINT('',#41489);
#5128=VERTEX_POINT('',#41513);
#5129=VERTEX_POINT('',#41514);
#5130=VERTEX_POINT('',#41537);
#5131=VERTEX_POINT('',#41538);
#5132=VERTEX_POINT('',#41562);
#5133=VERTEX_POINT('',#41563);
#5134=VERTEX_POINT('',#41587);
#5135=VERTEX_POINT('',#41588);
#5136=VERTEX_POINT('',#41611);
#5137=VERTEX_POINT('',#41612);
#5138=VERTEX_POINT('',#41636);
#5139=VERTEX_POINT('',#41637);
#5140=VERTEX_POINT('',#41661);
#5141=VERTEX_POINT('',#41662);
#5142=VERTEX_POINT('',#41685);
#5143=VERTEX_POINT('',#41686);
#5144=VERTEX_POINT('',#41710);
#5145=VERTEX_POINT('',#41711);
#5146=VERTEX_POINT('',#41735);
#5147=VERTEX_POINT('',#41736);
#5148=VERTEX_POINT('',#41759);
#5149=VERTEX_POINT('',#41881);
#5150=VERTEX_POINT('',#41916);
#5151=VERTEX_POINT('',#41934);
#5152=VERTEX_POINT('',#42421);
#5153=VERTEX_POINT('',#42505);
#5154=VERTEX_POINT('',#43084);
#5155=VERTEX_POINT('',#43085);
#5156=VERTEX_POINT('',#43087);
#5157=VERTEX_POINT('',#43089);
#5158=VERTEX_POINT('',#43093);
#5159=VERTEX_POINT('',#43095);
#5160=VERTEX_POINT('',#43099);
#5161=VERTEX_POINT('',#43101);
#5162=VERTEX_POINT('',#43105);
#5163=VERTEX_POINT('',#43107);
#5164=VERTEX_POINT('',#43111);
#5165=VERTEX_POINT('',#43113);
#5166=VERTEX_POINT('',#43121);
#5167=VERTEX_POINT('',#43124);
#5168=VERTEX_POINT('',#43131);
#5169=VERTEX_POINT('',#43132);
#5170=VERTEX_POINT('',#43134);
#5171=VERTEX_POINT('',#43145);
#5172=VERTEX_POINT('',#43158);
#5173=VERTEX_POINT('',#43159);
#5174=VERTEX_POINT('',#43206);
#5175=VERTEX_POINT('',#43207);
#5176=VERTEX_POINT('',#43209);
#5177=VERTEX_POINT('',#43221);
#5178=VERTEX_POINT('',#43233);
#5179=VERTEX_POINT('',#43234);
#5180=VERTEX_POINT('',#43258);
#5181=VERTEX_POINT('',#43407);
#5182=VERTEX_POINT('',#43457);
#5183=VERTEX_POINT('',#43484);
#5184=VERTEX_POINT('',#43575);
#5185=VERTEX_POINT('',#43669);
#5186=VERTEX_POINT('',#43864);
#5187=VERTEX_POINT('',#43865);
#5188=VERTEX_POINT('',#43867);
#5189=VERTEX_POINT('',#43869);
#5190=VERTEX_POINT('',#43873);
#5191=VERTEX_POINT('',#43875);
#5192=VERTEX_POINT('',#43879);
#5193=VERTEX_POINT('',#43881);
#5194=VERTEX_POINT('',#43885);
#5195=VERTEX_POINT('',#43887);
#5196=VERTEX_POINT('',#43891);
#5197=VERTEX_POINT('',#43893);
#5198=VERTEX_POINT('',#43901);
#5199=VERTEX_POINT('',#43904);
#5200=EDGE_CURVE('',#4094,#4095,#2830,.T.);
#5201=EDGE_CURVE('',#4095,#4096,#1992,.T.);
#5202=EDGE_CURVE('',#4096,#4097,#1801,.T.);
#5203=EDGE_CURVE('',#4097,#4098,#1993,.T.);
#5204=EDGE_CURVE('',#4098,#4099,#2831,.T.);
#5205=EDGE_CURVE('',#4099,#4099,#1802,.F.);
#5206=EDGE_CURVE('',#4098,#4094,#1994,.T.);
#5207=EDGE_CURVE('',#4100,#4101,#2832,.T.);
#5208=EDGE_CURVE('',#4101,#4095,#1995,.T.);
#5209=EDGE_CURVE('',#4094,#4100,#1996,.T.);
#5210=EDGE_CURVE('',#4102,#4103,#2833,.T.);
#5211=EDGE_CURVE('',#4103,#4101,#1997,.T.);
#5212=EDGE_CURVE('',#4100,#4102,#1998,.T.);
#5213=EDGE_CURVE('',#4104,#4105,#2834,.T.);
#5214=EDGE_CURVE('',#4105,#4103,#1999,.T.);
#5215=EDGE_CURVE('',#4102,#4104,#2000,.T.);
#5216=EDGE_CURVE('',#4106,#4107,#2835,.T.);
#5217=EDGE_CURVE('',#4107,#4105,#2001,.T.);
#5218=EDGE_CURVE('',#4104,#4106,#2002,.T.);
#5219=EDGE_CURVE('',#4108,#4109,#2836,.T.);
#5220=EDGE_CURVE('',#4109,#4107,#2003,.T.);
#5221=EDGE_CURVE('',#4106,#4108,#2004,.T.);
#5222=EDGE_CURVE('',#4110,#4111,#2837,.T.);
#5223=EDGE_CURVE('',#4111,#4109,#2005,.T.);
#5224=EDGE_CURVE('',#4108,#4110,#2006,.T.);
#5225=EDGE_CURVE('',#4112,#4113,#2838,.T.);
#5226=EDGE_CURVE('',#4113,#4111,#2007,.T.);
#5227=EDGE_CURVE('',#4110,#4112,#2008,.T.);
#5228=EDGE_CURVE('',#4114,#4115,#2839,.T.);
#5229=EDGE_CURVE('',#4115,#4113,#2009,.T.);
#5230=EDGE_CURVE('',#4112,#4114,#2010,.T.);
#5231=EDGE_CURVE('',#4116,#4117,#2840,.T.);
#5232=EDGE_CURVE('',#4117,#4115,#2011,.T.);
#5233=EDGE_CURVE('',#4114,#4116,#2012,.T.);
#5234=EDGE_CURVE('',#4118,#4119,#2841,.T.);
#5235=EDGE_CURVE('',#4119,#4117,#2013,.T.);
#5236=EDGE_CURVE('',#4116,#4118,#2014,.T.);
#5237=EDGE_CURVE('',#4120,#4121,#2842,.T.);
#5238=EDGE_CURVE('',#4120,#4122,#2015,.T.);
#5239=EDGE_CURVE('',#4123,#4122,#1803,.T.);
#5240=EDGE_CURVE('',#4123,#4121,#2016,.T.);
#5241=EDGE_CURVE('',#4124,#4125,#2843,.T.);
#5242=EDGE_CURVE('',#4125,#4126,#2017,.T.);
#5243=EDGE_CURVE('',#4127,#4126,#1804,.T.);
#5244=EDGE_CURVE('',#4124,#4127,#2018,.T.);
#5245=EDGE_CURVE('',#4128,#4129,#2844,.T.);
#5246=EDGE_CURVE('',#4129,#4125,#2019,.T.);
#5247=EDGE_CURVE('',#4128,#4124,#2020,.T.);
#5248=EDGE_CURVE('',#4130,#4131,#2845,.T.);
#5249=EDGE_CURVE('',#4131,#4129,#2021,.T.);
#5250=EDGE_CURVE('',#4130,#4128,#2022,.T.);
#5251=EDGE_CURVE('',#4132,#4133,#2846,.T.);
#5252=EDGE_CURVE('',#4133,#4131,#2023,.T.);
#5253=EDGE_CURVE('',#4132,#4130,#2024,.T.);
#5254=EDGE_CURVE('',#4134,#4135,#2847,.T.);
#5255=EDGE_CURVE('',#4135,#4133,#2025,.T.);
#5256=EDGE_CURVE('',#4134,#4132,#2026,.T.);
#5257=EDGE_CURVE('',#4136,#4137,#2848,.T.);
#5258=EDGE_CURVE('',#4137,#4135,#2027,.T.);
#5259=EDGE_CURVE('',#4136,#4134,#2028,.T.);
#5260=EDGE_CURVE('',#4138,#4139,#2849,.T.);
#5261=EDGE_CURVE('',#4139,#4137,#2029,.T.);
#5262=EDGE_CURVE('',#4138,#4136,#2030,.T.);
#5263=EDGE_CURVE('',#4140,#4141,#2850,.T.);
#5264=EDGE_CURVE('',#4141,#4139,#2031,.T.);
#5265=EDGE_CURVE('',#4140,#4138,#2032,.T.);
#5266=EDGE_CURVE('',#4142,#4143,#2851,.T.);
#5267=EDGE_CURVE('',#4143,#4141,#2033,.T.);
#5268=EDGE_CURVE('',#4142,#4140,#2034,.T.);
#5269=EDGE_CURVE('',#4144,#4145,#2852,.T.);
#5270=EDGE_CURVE('',#4145,#4143,#2035,.T.);
#5271=EDGE_CURVE('',#4144,#4142,#2036,.T.);
#5272=EDGE_CURVE('',#4146,#4147,#2853,.T.);
#5273=EDGE_CURVE('',#4147,#4145,#2037,.T.);
#5274=EDGE_CURVE('',#4146,#4144,#2038,.T.);
#5275=EDGE_CURVE('',#4148,#4149,#2854,.T.);
#5276=EDGE_CURVE('',#4149,#4147,#2039,.T.);
#5277=EDGE_CURVE('',#4148,#4146,#2040,.T.);
#5278=EDGE_CURVE('',#4150,#4151,#2855,.T.);
#5279=EDGE_CURVE('',#4152,#4150,#2041,.T.);
#5280=EDGE_CURVE('',#4153,#4152,#1805,.T.);
#5281=EDGE_CURVE('',#4153,#4151,#2042,.T.);
#5282=EDGE_CURVE('',#4154,#4155,#2856,.T.);
#5283=EDGE_CURVE('',#4155,#4156,#2043,.T.);
#5284=EDGE_CURVE('',#4156,#4157,#1806,.T.);
#5285=EDGE_CURVE('',#4157,#4158,#2044,.T.);
#5286=EDGE_CURVE('',#4158,#4159,#2857,.T.);
#5287=EDGE_CURVE('',#4159,#4159,#1807,.F.);
#5288=EDGE_CURVE('',#4158,#4154,#2045,.T.);
#5289=EDGE_CURVE('',#4160,#4161,#2858,.T.);
#5290=EDGE_CURVE('',#4161,#4155,#2046,.T.);
#5291=EDGE_CURVE('',#4154,#4160,#2047,.T.);
#5292=EDGE_CURVE('',#4162,#4163,#2859,.T.);
#5293=EDGE_CURVE('',#4163,#4161,#2048,.T.);
#5294=EDGE_CURVE('',#4160,#4162,#2049,.T.);
#5295=EDGE_CURVE('',#4164,#4165,#2860,.T.);
#5296=EDGE_CURVE('',#4165,#4163,#2050,.T.);
#5297=EDGE_CURVE('',#4162,#4164,#2051,.T.);
#5298=EDGE_CURVE('',#4166,#4167,#2861,.T.);
#5299=EDGE_CURVE('',#4167,#4165,#2052,.T.);
#5300=EDGE_CURVE('',#4164,#4166,#2053,.T.);
#5301=EDGE_CURVE('',#4168,#4169,#2862,.T.);
#5302=EDGE_CURVE('',#4169,#4167,#2054,.T.);
#5303=EDGE_CURVE('',#4166,#4168,#2055,.T.);
#5304=EDGE_CURVE('',#4170,#4171,#2863,.T.);
#5305=EDGE_CURVE('',#4171,#4169,#2056,.T.);
#5306=EDGE_CURVE('',#4168,#4170,#2057,.T.);
#5307=EDGE_CURVE('',#4172,#4173,#2864,.T.);
#5308=EDGE_CURVE('',#4173,#4171,#2058,.T.);
#5309=EDGE_CURVE('',#4170,#4172,#2059,.T.);
#5310=EDGE_CURVE('',#4174,#4175,#2865,.T.);
#5311=EDGE_CURVE('',#4175,#4173,#2060,.T.);
#5312=EDGE_CURVE('',#4172,#4174,#2061,.T.);
#5313=EDGE_CURVE('',#4176,#4177,#2866,.T.);
#5314=EDGE_CURVE('',#4177,#4175,#2062,.T.);
#5315=EDGE_CURVE('',#4174,#4176,#2063,.T.);
#5316=EDGE_CURVE('',#4178,#4179,#2867,.T.);
#5317=EDGE_CURVE('',#4179,#4177,#2064,.T.);
#5318=EDGE_CURVE('',#4176,#4178,#2065,.T.);
#5319=EDGE_CURVE('',#4180,#4181,#2868,.T.);
#5320=EDGE_CURVE('',#4180,#4182,#2066,.T.);
#5321=EDGE_CURVE('',#4183,#4182,#1808,.T.);
#5322=EDGE_CURVE('',#4183,#4181,#2067,.T.);
#5323=EDGE_CURVE('',#4184,#4185,#2869,.T.);
#5324=EDGE_CURVE('',#4185,#4186,#2068,.T.);
#5325=EDGE_CURVE('',#4187,#4186,#1809,.T.);
#5326=EDGE_CURVE('',#4184,#4187,#2069,.T.);
#5327=EDGE_CURVE('',#4188,#4189,#2870,.T.);
#5328=EDGE_CURVE('',#4189,#4185,#2070,.T.);
#5329=EDGE_CURVE('',#4188,#4184,#2071,.T.);
#5330=EDGE_CURVE('',#4190,#4191,#2871,.T.);
#5331=EDGE_CURVE('',#4191,#4189,#2072,.T.);
#5332=EDGE_CURVE('',#4190,#4188,#2073,.T.);
#5333=EDGE_CURVE('',#4192,#4193,#2872,.T.);
#5334=EDGE_CURVE('',#4193,#4191,#2074,.T.);
#5335=EDGE_CURVE('',#4192,#4190,#2075,.T.);
#5336=EDGE_CURVE('',#4194,#4195,#2873,.T.);
#5337=EDGE_CURVE('',#4195,#4193,#2076,.T.);
#5338=EDGE_CURVE('',#4194,#4192,#2077,.T.);
#5339=EDGE_CURVE('',#4196,#4197,#2874,.T.);
#5340=EDGE_CURVE('',#4197,#4195,#2078,.T.);
#5341=EDGE_CURVE('',#4196,#4194,#2079,.T.);
#5342=EDGE_CURVE('',#4198,#4199,#2875,.T.);
#5343=EDGE_CURVE('',#4199,#4197,#2080,.T.);
#5344=EDGE_CURVE('',#4198,#4196,#2081,.T.);
#5345=EDGE_CURVE('',#4200,#4201,#2876,.T.);
#5346=EDGE_CURVE('',#4201,#4199,#2082,.T.);
#5347=EDGE_CURVE('',#4200,#4198,#2083,.T.);
#5348=EDGE_CURVE('',#4202,#4203,#2877,.T.);
#5349=EDGE_CURVE('',#4203,#4201,#2084,.T.);
#5350=EDGE_CURVE('',#4202,#4200,#2085,.T.);
#5351=EDGE_CURVE('',#4204,#4205,#2878,.T.);
#5352=EDGE_CURVE('',#4205,#4203,#2086,.T.);
#5353=EDGE_CURVE('',#4204,#4202,#2087,.T.);
#5354=EDGE_CURVE('',#4206,#4207,#2879,.T.);
#5355=EDGE_CURVE('',#4207,#4205,#2088,.T.);
#5356=EDGE_CURVE('',#4206,#4204,#2089,.T.);
#5357=EDGE_CURVE('',#4208,#4209,#2880,.T.);
#5358=EDGE_CURVE('',#4209,#4207,#2090,.T.);
#5359=EDGE_CURVE('',#4208,#4206,#2091,.T.);
#5360=EDGE_CURVE('',#4210,#4211,#2881,.T.);
#5361=EDGE_CURVE('',#4212,#4210,#2092,.T.);
#5362=EDGE_CURVE('',#4213,#4212,#1810,.T.);
#5363=EDGE_CURVE('',#4213,#4211,#2093,.T.);
#5364=EDGE_CURVE('',#4214,#4215,#2882,.T.);
#5365=EDGE_CURVE('',#4215,#4216,#2094,.T.);
#5366=EDGE_CURVE('',#4216,#4217,#1811,.T.);
#5367=EDGE_CURVE('',#4217,#4218,#2095,.T.);
#5368=EDGE_CURVE('',#4218,#4219,#2883,.T.);
#5369=EDGE_CURVE('',#4219,#4219,#1812,.F.);
#5370=EDGE_CURVE('',#4218,#4214,#2096,.T.);
#5371=EDGE_CURVE('',#4220,#4221,#2884,.T.);
#5372=EDGE_CURVE('',#4221,#4215,#2097,.T.);
#5373=EDGE_CURVE('',#4214,#4220,#2098,.T.);
#5374=EDGE_CURVE('',#4222,#4223,#2885,.T.);
#5375=EDGE_CURVE('',#4223,#4221,#2099,.T.);
#5376=EDGE_CURVE('',#4220,#4222,#2100,.T.);
#5377=EDGE_CURVE('',#4224,#4225,#2886,.T.);
#5378=EDGE_CURVE('',#4225,#4223,#2101,.T.);
#5379=EDGE_CURVE('',#4222,#4224,#2102,.T.);
#5380=EDGE_CURVE('',#4226,#4227,#2887,.T.);
#5381=EDGE_CURVE('',#4227,#4225,#2103,.T.);
#5382=EDGE_CURVE('',#4224,#4226,#2104,.T.);
#5383=EDGE_CURVE('',#4228,#4229,#2888,.T.);
#5384=EDGE_CURVE('',#4229,#4227,#2105,.T.);
#5385=EDGE_CURVE('',#4226,#4228,#2106,.T.);
#5386=EDGE_CURVE('',#4230,#4231,#2889,.T.);
#5387=EDGE_CURVE('',#4231,#4229,#2107,.T.);
#5388=EDGE_CURVE('',#4228,#4230,#2108,.T.);
#5389=EDGE_CURVE('',#4232,#4233,#2890,.T.);
#5390=EDGE_CURVE('',#4233,#4231,#2109,.T.);
#5391=EDGE_CURVE('',#4230,#4232,#2110,.T.);
#5392=EDGE_CURVE('',#4234,#4235,#2891,.T.);
#5393=EDGE_CURVE('',#4235,#4233,#2111,.T.);
#5394=EDGE_CURVE('',#4232,#4234,#2112,.T.);
#5395=EDGE_CURVE('',#4236,#4237,#2892,.T.);
#5396=EDGE_CURVE('',#4237,#4235,#2113,.T.);
#5397=EDGE_CURVE('',#4234,#4236,#2114,.T.);
#5398=EDGE_CURVE('',#4238,#4239,#2893,.T.);
#5399=EDGE_CURVE('',#4239,#4237,#2115,.T.);
#5400=EDGE_CURVE('',#4236,#4238,#2116,.T.);
#5401=EDGE_CURVE('',#4240,#4241,#2894,.T.);
#5402=EDGE_CURVE('',#4240,#4242,#2117,.T.);
#5403=EDGE_CURVE('',#4243,#4242,#1813,.T.);
#5404=EDGE_CURVE('',#4243,#4241,#2118,.T.);
#5405=EDGE_CURVE('',#4244,#4245,#2895,.T.);
#5406=EDGE_CURVE('',#4245,#4246,#2119,.T.);
#5407=EDGE_CURVE('',#4247,#4246,#1814,.T.);
#5408=EDGE_CURVE('',#4244,#4247,#2120,.T.);
#5409=EDGE_CURVE('',#4248,#4249,#2896,.T.);
#5410=EDGE_CURVE('',#4249,#4245,#2121,.T.);
#5411=EDGE_CURVE('',#4248,#4244,#2122,.T.);
#5412=EDGE_CURVE('',#4250,#4251,#2897,.T.);
#5413=EDGE_CURVE('',#4251,#4249,#2123,.T.);
#5414=EDGE_CURVE('',#4250,#4248,#2124,.T.);
#5415=EDGE_CURVE('',#4252,#4253,#2898,.T.);
#5416=EDGE_CURVE('',#4253,#4251,#2125,.T.);
#5417=EDGE_CURVE('',#4252,#4250,#2126,.T.);
#5418=EDGE_CURVE('',#4254,#4255,#2899,.T.);
#5419=EDGE_CURVE('',#4255,#4253,#2127,.T.);
#5420=EDGE_CURVE('',#4254,#4252,#2128,.T.);
#5421=EDGE_CURVE('',#4256,#4257,#2900,.T.);
#5422=EDGE_CURVE('',#4257,#4255,#2129,.T.);
#5423=EDGE_CURVE('',#4256,#4254,#2130,.T.);
#5424=EDGE_CURVE('',#4258,#4259,#2901,.T.);
#5425=EDGE_CURVE('',#4259,#4257,#2131,.T.);
#5426=EDGE_CURVE('',#4258,#4256,#2132,.T.);
#5427=EDGE_CURVE('',#4260,#4261,#2902,.T.);
#5428=EDGE_CURVE('',#4261,#4259,#2133,.T.);
#5429=EDGE_CURVE('',#4260,#4258,#2134,.T.);
#5430=EDGE_CURVE('',#4262,#4263,#2903,.T.);
#5431=EDGE_CURVE('',#4263,#4261,#2135,.T.);
#5432=EDGE_CURVE('',#4262,#4260,#2136,.T.);
#5433=EDGE_CURVE('',#4264,#4265,#2904,.T.);
#5434=EDGE_CURVE('',#4265,#4263,#2137,.T.);
#5435=EDGE_CURVE('',#4264,#4262,#2138,.T.);
#5436=EDGE_CURVE('',#4266,#4267,#2905,.T.);
#5437=EDGE_CURVE('',#4267,#4265,#2139,.T.);
#5438=EDGE_CURVE('',#4266,#4264,#2140,.T.);
#5439=EDGE_CURVE('',#4268,#4269,#2906,.T.);
#5440=EDGE_CURVE('',#4269,#4267,#2141,.T.);
#5441=EDGE_CURVE('',#4268,#4266,#2142,.T.);
#5442=EDGE_CURVE('',#4270,#4271,#2907,.T.);
#5443=EDGE_CURVE('',#4272,#4270,#2143,.T.);
#5444=EDGE_CURVE('',#4273,#4272,#1815,.T.);
#5445=EDGE_CURVE('',#4273,#4271,#2144,.T.);
#5446=EDGE_CURVE('',#4274,#4275,#2908,.T.);
#5447=EDGE_CURVE('',#4275,#4276,#2145,.T.);
#5448=EDGE_CURVE('',#4276,#4277,#1816,.T.);
#5449=EDGE_CURVE('',#4277,#4278,#2146,.T.);
#5450=EDGE_CURVE('',#4278,#4279,#2909,.T.);
#5451=EDGE_CURVE('',#4279,#4279,#1817,.F.);
#5452=EDGE_CURVE('',#4278,#4274,#2147,.T.);
#5453=EDGE_CURVE('',#4280,#4281,#2910,.T.);
#5454=EDGE_CURVE('',#4281,#4275,#2148,.T.);
#5455=EDGE_CURVE('',#4274,#4280,#2149,.T.);
#5456=EDGE_CURVE('',#4282,#4283,#2911,.T.);
#5457=EDGE_CURVE('',#4283,#4281,#2150,.T.);
#5458=EDGE_CURVE('',#4280,#4282,#2151,.T.);
#5459=EDGE_CURVE('',#4284,#4285,#2912,.T.);
#5460=EDGE_CURVE('',#4285,#4283,#2152,.T.);
#5461=EDGE_CURVE('',#4282,#4284,#2153,.T.);
#5462=EDGE_CURVE('',#4286,#4287,#2913,.T.);
#5463=EDGE_CURVE('',#4287,#4285,#2154,.T.);
#5464=EDGE_CURVE('',#4284,#4286,#2155,.T.);
#5465=EDGE_CURVE('',#4288,#4289,#2914,.T.);
#5466=EDGE_CURVE('',#4289,#4287,#2156,.T.);
#5467=EDGE_CURVE('',#4286,#4288,#2157,.T.);
#5468=EDGE_CURVE('',#4290,#4291,#2915,.T.);
#5469=EDGE_CURVE('',#4291,#4289,#2158,.T.);
#5470=EDGE_CURVE('',#4288,#4290,#2159,.T.);
#5471=EDGE_CURVE('',#4292,#4293,#2916,.T.);
#5472=EDGE_CURVE('',#4293,#4291,#2160,.T.);
#5473=EDGE_CURVE('',#4290,#4292,#2161,.T.);
#5474=EDGE_CURVE('',#4294,#4295,#2917,.T.);
#5475=EDGE_CURVE('',#4295,#4293,#2162,.T.);
#5476=EDGE_CURVE('',#4292,#4294,#2163,.T.);
#5477=EDGE_CURVE('',#4296,#4297,#2918,.T.);
#5478=EDGE_CURVE('',#4297,#4295,#2164,.T.);
#5479=EDGE_CURVE('',#4294,#4296,#2165,.T.);
#5480=EDGE_CURVE('',#4298,#4299,#2919,.T.);
#5481=EDGE_CURVE('',#4299,#4297,#2166,.T.);
#5482=EDGE_CURVE('',#4296,#4298,#2167,.T.);
#5483=EDGE_CURVE('',#4300,#4301,#2920,.T.);
#5484=EDGE_CURVE('',#4300,#4302,#2168,.T.);
#5485=EDGE_CURVE('',#4303,#4302,#1818,.T.);
#5486=EDGE_CURVE('',#4303,#4301,#2169,.T.);
#5487=EDGE_CURVE('',#4304,#4305,#2921,.T.);
#5488=EDGE_CURVE('',#4305,#4306,#2170,.T.);
#5489=EDGE_CURVE('',#4307,#4306,#1819,.T.);
#5490=EDGE_CURVE('',#4304,#4307,#2171,.T.);
#5491=EDGE_CURVE('',#4308,#4309,#2922,.T.);
#5492=EDGE_CURVE('',#4309,#4305,#2172,.T.);
#5493=EDGE_CURVE('',#4308,#4304,#2173,.T.);
#5494=EDGE_CURVE('',#4310,#4311,#2923,.T.);
#5495=EDGE_CURVE('',#4311,#4309,#2174,.T.);
#5496=EDGE_CURVE('',#4310,#4308,#2175,.T.);
#5497=EDGE_CURVE('',#4312,#4313,#2924,.T.);
#5498=EDGE_CURVE('',#4313,#4311,#2176,.T.);
#5499=EDGE_CURVE('',#4312,#4310,#2177,.T.);
#5500=EDGE_CURVE('',#4314,#4315,#2925,.T.);
#5501=EDGE_CURVE('',#4315,#4313,#2178,.T.);
#5502=EDGE_CURVE('',#4314,#4312,#2179,.T.);
#5503=EDGE_CURVE('',#4316,#4317,#2926,.T.);
#5504=EDGE_CURVE('',#4317,#4315,#2180,.T.);
#5505=EDGE_CURVE('',#4316,#4314,#2181,.T.);
#5506=EDGE_CURVE('',#4318,#4319,#2927,.T.);
#5507=EDGE_CURVE('',#4319,#4317,#2182,.T.);
#5508=EDGE_CURVE('',#4318,#4316,#2183,.T.);
#5509=EDGE_CURVE('',#4320,#4321,#2928,.T.);
#5510=EDGE_CURVE('',#4321,#4319,#2184,.T.);
#5511=EDGE_CURVE('',#4320,#4318,#2185,.T.);
#5512=EDGE_CURVE('',#4322,#4323,#2929,.T.);
#5513=EDGE_CURVE('',#4323,#4321,#2186,.T.);
#5514=EDGE_CURVE('',#4322,#4320,#2187,.T.);
#5515=EDGE_CURVE('',#4324,#4325,#2930,.T.);
#5516=EDGE_CURVE('',#4325,#4323,#2188,.T.);
#5517=EDGE_CURVE('',#4324,#4322,#2189,.T.);
#5518=EDGE_CURVE('',#4326,#4327,#2931,.T.);
#5519=EDGE_CURVE('',#4327,#4325,#2190,.T.);
#5520=EDGE_CURVE('',#4326,#4324,#2191,.T.);
#5521=EDGE_CURVE('',#4328,#4329,#2932,.T.);
#5522=EDGE_CURVE('',#4329,#4327,#2192,.T.);
#5523=EDGE_CURVE('',#4328,#4326,#2193,.T.);
#5524=EDGE_CURVE('',#4330,#4331,#2933,.T.);
#5525=EDGE_CURVE('',#4332,#4330,#2194,.T.);
#5526=EDGE_CURVE('',#4333,#4332,#1820,.T.);
#5527=EDGE_CURVE('',#4333,#4331,#2195,.T.);
#5528=EDGE_CURVE('',#4334,#4334,#1821,.T.);
#5529=EDGE_CURVE('',#4334,#4335,#2934,.T.);
#5530=EDGE_CURVE('',#4335,#4335,#1822,.T.);
#5531=EDGE_CURVE('',#4336,#4336,#1823,.T.);
#5532=EDGE_CURVE('',#4337,#4337,#1824,.T.);
#5533=EDGE_CURVE('',#4338,#4338,#1825,.T.);
#5534=EDGE_CURVE('',#4338,#4336,#2935,.T.);
#5535=EDGE_CURVE('',#4337,#4339,#2936,.T.);
#5536=EDGE_CURVE('',#4339,#4339,#1826,.T.);
#5537=EDGE_CURVE('',#4340,#4340,#1827,.T.);
#5538=EDGE_CURVE('',#4341,#4341,#1828,.T.);
#5539=EDGE_CURVE('',#4342,#4342,#1829,.T.);
#5540=EDGE_CURVE('',#4342,#4340,#2937,.T.);
#5541=EDGE_CURVE('',#4341,#4343,#2938,.T.);
#5542=EDGE_CURVE('',#4343,#4343,#1830,.T.);
#5543=EDGE_CURVE('',#4276,#4307,#2196,.T.);
#5544=EDGE_CURVE('',#4306,#4277,#2197,.T.);
#5545=EDGE_CURVE('',#4331,#4329,#2198,.T.);
#5546=EDGE_CURVE('',#4330,#4328,#2199,.T.);
#5547=EDGE_CURVE('',#4302,#4333,#2200,.T.);
#5548=EDGE_CURVE('',#4298,#4300,#2201,.T.);
#5549=EDGE_CURVE('',#4301,#4299,#2202,.T.);
#5550=EDGE_CURVE('',#4332,#4303,#2203,.T.);
#5551=EDGE_CURVE('',#4216,#4247,#2204,.T.);
#5552=EDGE_CURVE('',#4246,#4217,#2205,.T.);
#5553=EDGE_CURVE('',#4271,#4269,#2206,.T.);
#5554=EDGE_CURVE('',#4270,#4268,#2207,.T.);
#5555=EDGE_CURVE('',#4242,#4273,#2208,.T.);
#5556=EDGE_CURVE('',#4238,#4240,#2209,.T.);
#5557=EDGE_CURVE('',#4241,#4239,#2210,.T.);
#5558=EDGE_CURVE('',#4272,#4243,#2211,.T.);
#5559=EDGE_CURVE('',#4156,#4187,#2212,.T.);
#5560=EDGE_CURVE('',#4186,#4157,#2213,.T.);
#5561=EDGE_CURVE('',#4211,#4209,#2214,.T.);
#5562=EDGE_CURVE('',#4210,#4208,#2215,.T.);
#5563=EDGE_CURVE('',#4182,#4213,#2216,.T.);
#5564=EDGE_CURVE('',#4178,#4180,#2217,.T.);
#5565=EDGE_CURVE('',#4181,#4179,#2218,.T.);
#5566=EDGE_CURVE('',#4212,#4183,#2219,.T.);
#5567=EDGE_CURVE('',#4096,#4127,#2220,.T.);
#5568=EDGE_CURVE('',#4126,#4097,#2221,.T.);
#5569=EDGE_CURVE('',#4151,#4149,#2222,.T.);
#5570=EDGE_CURVE('',#4150,#4148,#2223,.T.);
#5571=EDGE_CURVE('',#4122,#4153,#2224,.T.);
#5572=EDGE_CURVE('',#4118,#4120,#2225,.T.);
#5573=EDGE_CURVE('',#4121,#4119,#2226,.T.);
#5574=EDGE_CURVE('',#4152,#4123,#2227,.T.);
#5575=EDGE_CURVE('',#4344,#4344,#1831,.T.);
#5576=EDGE_CURVE('',#4344,#4345,#2939,.T.);
#5577=EDGE_CURVE('',#4345,#4345,#1832,.T.);
#5578=EDGE_CURVE('',#4346,#4346,#1833,.T.);
#5579=EDGE_CURVE('',#4346,#4347,#2940,.T.);
#5580=EDGE_CURVE('',#4347,#4347,#1834,.T.);
#5581=EDGE_CURVE('',#4348,#4349,#2941,.T.);
#5582=EDGE_CURVE('',#4350,#4349,#2942,.T.);
#5583=EDGE_CURVE('',#4351,#4350,#2943,.T.);
#5584=EDGE_CURVE('',#4348,#4351,#2944,.T.);
#5585=EDGE_CURVE('',#4352,#4348,#2945,.T.);
#5586=EDGE_CURVE('',#4353,#4351,#2946,.T.);
#5587=EDGE_CURVE('',#4352,#4353,#2947,.T.);
#5588=EDGE_CURVE('',#4354,#4352,#2948,.T.);
#5589=EDGE_CURVE('',#4355,#4353,#2949,.T.);
#5590=EDGE_CURVE('',#4354,#4355,#2950,.T.);
#5591=EDGE_CURVE('',#4355,#4350,#2951,.T.);
#5592=EDGE_CURVE('',#4356,#4357,#2952,.T.);
#5593=EDGE_CURVE('',#4357,#4358,#2953,.T.);
#5594=EDGE_CURVE('',#4359,#4358,#2954,.T.);
#5595=EDGE_CURVE('',#4356,#4359,#2955,.T.);
#5596=EDGE_CURVE('',#4360,#4361,#2956,.T.);
#5597=EDGE_CURVE('',#4362,#4361,#2957,.T.);
#5598=EDGE_CURVE('',#4363,#4362,#2958,.T.);
#5599=EDGE_CURVE('',#4360,#4363,#2959,.T.);
#5600=EDGE_CURVE('',#4357,#4360,#2960,.T.);
#5601=EDGE_CURVE('',#4358,#4363,#2961,.T.);
#5602=EDGE_CURVE('',#4359,#4362,#2962,.T.);
#5603=EDGE_CURVE('',#4364,#4364,#1835,.T.);
#5604=EDGE_CURVE('',#4364,#4365,#2963,.T.);
#5605=EDGE_CURVE('',#4365,#4365,#1836,.T.);
#5606=EDGE_CURVE('',#4366,#4366,#1837,.T.);
#5607=EDGE_CURVE('',#4366,#4367,#2964,.T.);
#5608=EDGE_CURVE('',#4367,#4367,#1838,.T.);
#5609=EDGE_CURVE('',#4368,#4369,#1839,.T.);
#5610=EDGE_CURVE('',#4370,#4369,#2965,.T.);
#5611=EDGE_CURVE('',#4370,#4371,#1840,.T.);
#5612=EDGE_CURVE('',#4372,#4371,#2966,.T.);
#5613=EDGE_CURVE('',#4372,#4373,#1841,.T.);
#5614=EDGE_CURVE('',#4374,#4373,#2967,.T.);
#5615=EDGE_CURVE('',#4374,#4375,#1842,.T.);
#5616=EDGE_CURVE('',#4368,#4375,#2968,.T.);
#5617=EDGE_CURVE('',#4368,#4376,#2969,.T.);
#5618=EDGE_CURVE('',#4376,#4377,#1843,.T.);
#5619=EDGE_CURVE('',#4377,#4369,#2970,.T.);
#5620=EDGE_CURVE('',#4378,#4375,#2971,.T.);
#5621=EDGE_CURVE('',#4376,#4378,#2972,.T.);
#5622=EDGE_CURVE('',#4374,#4379,#2973,.T.);
#5623=EDGE_CURVE('',#4379,#4378,#1844,.T.);
#5624=EDGE_CURVE('',#4380,#4373,#2974,.T.);
#5625=EDGE_CURVE('',#4379,#4380,#2975,.T.);
#5626=EDGE_CURVE('',#4370,#4381,#2976,.T.);
#5627=EDGE_CURVE('',#4381,#4382,#1845,.T.);
#5628=EDGE_CURVE('',#4382,#4371,#2977,.T.);
#5629=EDGE_CURVE('',#4383,#4382,#2978,.T.);
#5630=EDGE_CURVE('',#4372,#4383,#2979,.T.);
#5631=EDGE_CURVE('',#4383,#4380,#1846,.T.);
#5632=EDGE_CURVE('',#4381,#4377,#2980,.T.);
#5633=EDGE_CURVE('',#4384,#4385,#2981,.T.);
#5634=EDGE_CURVE('',#4385,#4386,#2982,.T.);
#5635=EDGE_CURVE('',#4387,#4386,#2983,.T.);
#5636=EDGE_CURVE('',#4384,#4387,#2984,.T.);
#5637=EDGE_CURVE('',#4349,#4384,#2985,.T.);
#5638=EDGE_CURVE('',#4388,#4387,#2986,.T.);
#5639=EDGE_CURVE('',#4389,#4388,#2987,.T.);
#5640=EDGE_CURVE('',#4389,#4354,#2988,.T.);
#5641=EDGE_CURVE('',#4390,#4389,#2989,.T.);
#5642=EDGE_CURVE('',#4391,#4388,#2990,.T.);
#5643=EDGE_CURVE('',#4390,#4391,#2991,.T.);
#5644=EDGE_CURVE('',#4361,#4390,#2992,.T.);
#5645=EDGE_CURVE('',#4386,#4391,#2993,.T.);
#5646=EDGE_CURVE('',#4385,#4356,#2994,.T.);
#5647=EDGE_CURVE('',#4392,#4393,#2995,.T.);
#5648=EDGE_CURVE('',#4393,#4394,#2228,.T.);
#5649=EDGE_CURVE('',#4394,#4395,#1847,.F.);
#5650=EDGE_CURVE('',#4395,#4392,#2229,.T.);
#5651=EDGE_CURVE('',#4396,#4397,#2996,.T.);
#5652=EDGE_CURVE('',#4397,#4393,#2230,.T.);
#5653=EDGE_CURVE('',#4392,#4396,#2231,.T.);
#5654=EDGE_CURVE('',#4398,#4399,#2997,.T.);
#5655=EDGE_CURVE('',#4398,#4400,#2232,.T.);
#5656=EDGE_CURVE('',#4401,#4400,#1848,.F.);
#5657=EDGE_CURVE('',#4401,#4399,#2233,.T.);
#5658=EDGE_CURVE('',#4402,#4403,#2998,.T.);
#5659=EDGE_CURVE('',#4403,#4404,#2234,.T.);
#5660=EDGE_CURVE('',#4404,#4405,#1849,.F.);
#5661=EDGE_CURVE('',#4405,#4402,#2235,.T.);
#5662=EDGE_CURVE('',#4406,#4407,#2999,.T.);
#5663=EDGE_CURVE('',#4407,#4403,#2236,.T.);
#5664=EDGE_CURVE('',#4402,#4406,#2237,.T.);
#5665=EDGE_CURVE('',#4408,#4409,#3000,.T.);
#5666=EDGE_CURVE('',#4408,#4410,#2238,.T.);
#5667=EDGE_CURVE('',#4411,#4410,#1850,.T.);
#5668=EDGE_CURVE('',#4411,#4409,#2239,.T.);
#5669=EDGE_CURVE('',#4412,#4413,#3001,.T.);
#5670=EDGE_CURVE('',#4413,#4414,#2240,.T.);
#5671=EDGE_CURVE('',#4415,#4414,#1851,.T.);
#5672=EDGE_CURVE('',#4412,#4415,#2241,.T.);
#5673=EDGE_CURVE('',#4416,#4417,#3002,.T.);
#5674=EDGE_CURVE('',#4417,#4413,#2242,.T.);
#5675=EDGE_CURVE('',#4416,#4412,#2243,.T.);
#5676=EDGE_CURVE('',#4418,#4419,#3003,.T.);
#5677=EDGE_CURVE('',#4419,#4417,#2244,.T.);
#5678=EDGE_CURVE('',#4418,#4416,#2245,.T.);
#5679=EDGE_CURVE('',#4420,#4421,#3004,.T.);
#5680=EDGE_CURVE('',#4422,#4420,#2246,.T.);
#5681=EDGE_CURVE('',#4423,#4422,#1852,.T.);
#5682=EDGE_CURVE('',#4423,#4421,#2247,.T.);
#5683=EDGE_CURVE('',#4424,#4425,#3005,.T.);
#5684=EDGE_CURVE('',#4425,#4426,#2248,.T.);
#5685=EDGE_CURVE('',#4427,#4426,#1853,.T.);
#5686=EDGE_CURVE('',#4424,#4427,#2249,.T.);
#5687=EDGE_CURVE('',#4428,#4429,#3006,.T.);
#5688=EDGE_CURVE('',#4429,#4425,#2250,.T.);
#5689=EDGE_CURVE('',#4428,#4424,#2251,.T.);
#5690=EDGE_CURVE('',#4430,#4431,#3007,.T.);
#5691=EDGE_CURVE('',#4431,#4429,#2252,.T.);
#5692=EDGE_CURVE('',#4430,#4428,#2253,.T.);
#5693=EDGE_CURVE('',#4432,#4433,#3008,.T.);
#5694=EDGE_CURVE('',#4434,#4432,#2254,.T.);
#5695=EDGE_CURVE('',#4435,#4434,#1854,.T.);
#5696=EDGE_CURVE('',#4435,#4433,#2255,.T.);
#5697=EDGE_CURVE('',#4436,#4437,#1855,.T.);
#5698=EDGE_CURVE('',#4436,#4438,#3009,.T.);
#5699=EDGE_CURVE('',#4437,#4438,#3010,.T.);
#5700=EDGE_CURVE('',#4439,#4440,#1856,.T.);
#5701=EDGE_CURVE('',#4441,#4440,#3011,.T.);
#5702=EDGE_CURVE('',#4439,#4441,#3012,.T.);
#5703=EDGE_CURVE('',#4442,#4443,#3013,.T.);
#5704=EDGE_CURVE('',#4443,#4444,#3014,.T.);
#5705=EDGE_CURVE('',#4445,#4444,#3015,.T.);
#5706=EDGE_CURVE('',#4442,#4445,#3016,.T.);
#5707=EDGE_CURVE('',#4446,#4447,#3017,.T.);
#5708=EDGE_CURVE('',#4447,#4448,#3018,.T.);
#5709=EDGE_CURVE('',#4449,#4448,#3019,.T.);
#5710=EDGE_CURVE('',#4446,#4449,#3020,.T.);
#5711=EDGE_CURVE('',#4450,#4446,#1857,.T.);
#5712=EDGE_CURVE('',#4450,#4449,#3021,.T.);
#5713=EDGE_CURVE('',#4451,#4439,#3022,.T.);
#5714=EDGE_CURVE('',#4452,#4441,#3023,.T.);
#5715=EDGE_CURVE('',#4451,#4452,#3024,.T.);
#5716=EDGE_CURVE('',#4436,#4453,#3025,.T.);
#5717=EDGE_CURVE('',#4453,#4454,#3026,.T.);
#5718=EDGE_CURVE('',#4438,#4454,#3027,.T.);
#5719=EDGE_CURVE('',#4455,#4443,#1858,.T.);
#5720=EDGE_CURVE('',#4444,#4455,#3028,.T.);
#5721=EDGE_CURVE('',#4437,#4455,#3029,.T.);
#5722=EDGE_CURVE('',#4454,#4452,#1859,.T.);
#5723=EDGE_CURVE('',#4450,#4440,#3030,.T.);
#5724=EDGE_CURVE('',#4448,#4445,#1860,.T.);
#5725=EDGE_CURVE('',#4456,#4456,#1861,.T.);
#5726=EDGE_CURVE('',#4440,#4450,#1862,.T.);
#5727=EDGE_CURVE('',#4433,#4431,#2256,.T.);
#5728=EDGE_CURVE('',#4432,#4430,#2257,.T.);
#5729=EDGE_CURVE('',#4426,#4405,#2258,.T.);
#5730=EDGE_CURVE('',#4410,#4435,#2259,.T.);
#5731=EDGE_CURVE('',#4406,#4408,#2260,.T.);
#5732=EDGE_CURVE('',#4404,#4427,#2261,.T.);
#5733=EDGE_CURVE('',#4409,#4407,#2262,.T.);
#5734=EDGE_CURVE('',#4434,#4411,#2263,.T.);
#5735=EDGE_CURVE('',#4421,#4419,#2264,.T.);
#5736=EDGE_CURVE('',#4420,#4418,#2265,.T.);
#5737=EDGE_CURVE('',#4414,#4395,#2266,.T.);
#5738=EDGE_CURVE('',#4400,#4423,#2267,.T.);
#5739=EDGE_CURVE('',#4396,#4398,#2268,.T.);
#5740=EDGE_CURVE('',#4394,#4415,#2269,.T.);
#5741=EDGE_CURVE('',#4399,#4397,#2270,.T.);
#5742=EDGE_CURVE('',#4422,#4401,#2271,.T.);
#5743=EDGE_CURVE('',#4457,#4457,#1863,.T.);
#5744=EDGE_CURVE('',#4457,#4458,#3031,.T.);
#5745=EDGE_CURVE('',#4458,#4458,#1864,.T.);
#5746=EDGE_CURVE('',#4459,#4459,#1865,.T.);
#5747=EDGE_CURVE('',#4459,#4460,#3032,.T.);
#5748=EDGE_CURVE('',#4461,#4460,#2272,.T.);
#5749=EDGE_CURVE('',#4460,#4461,#2273,.T.);
#5750=EDGE_CURVE('',#4462,#4463,#3033,.T.);
#5751=EDGE_CURVE('',#4453,#4462,#2274,.T.);
#5752=EDGE_CURVE('',#4437,#4455,#1866,.T.);
#5753=EDGE_CURVE('',#4464,#4442,#2275,.T.);
#5754=EDGE_CURVE('',#4465,#4464,#3034,.T.);
#5755=EDGE_CURVE('',#4463,#4465,#1867,.T.);
#5756=EDGE_CURVE('',#4463,#4465,#3035,.T.);
#5757=EDGE_CURVE('',#4466,#4467,#3036,.T.);
#5758=EDGE_CURVE('',#4467,#4468,#3037,.T.);
#5759=EDGE_CURVE('',#4468,#4469,#3038,.T.);
#5760=EDGE_CURVE('',#4469,#4466,#3039,.T.);
#5761=EDGE_CURVE('',#4470,#4470,#1868,.T.);
#5762=EDGE_CURVE('',#4471,#4471,#1869,.T.);
#5763=EDGE_CURVE('',#4472,#4472,#1870,.T.);
#5764=EDGE_CURVE('',#4473,#4473,#1871,.T.);
#5765=EDGE_CURVE('',#4464,#4474,#1872,.T.);
#5766=EDGE_CURVE('',#4474,#4475,#3040,.T.);
#5767=EDGE_CURVE('',#4475,#4476,#3041,.T.);
#5768=EDGE_CURVE('',#4476,#4477,#3042,.T.);
#5769=EDGE_CURVE('',#4477,#4462,#1873,.T.);
#5770=EDGE_CURVE('',#4447,#4474,#2276,.T.);
#5771=EDGE_CURVE('',#4478,#4478,#1874,.T.);
#5772=EDGE_CURVE('',#4478,#4479,#3043,.T.);
#5773=EDGE_CURVE('',#4479,#4479,#1875,.T.);
#5774=EDGE_CURVE('',#4480,#4480,#1876,.T.);
#5775=EDGE_CURVE('',#4480,#4481,#3044,.T.);
#5776=EDGE_CURVE('',#4482,#4481,#2277,.T.);
#5777=EDGE_CURVE('',#4483,#4482,#2278,.T.);
#5778=EDGE_CURVE('',#4484,#4483,#2279,.T.);
#5779=EDGE_CURVE('',#4481,#4484,#2280,.T.);
#5780=EDGE_CURVE('',#4475,#4476,#1877,.T.);
#5781=EDGE_CURVE('',#4477,#4451,#2281,.T.);
#5782=EDGE_CURVE('',#4470,#4485,#3045,.T.);
#5783=EDGE_CURVE('',#4485,#4485,#1878,.T.);
#5784=EDGE_CURVE('',#4471,#4486,#3046,.T.);
#5785=EDGE_CURVE('',#4486,#4486,#1879,.T.);
#5786=EDGE_CURVE('',#4472,#4487,#3047,.T.);
#5787=EDGE_CURVE('',#4487,#4487,#1880,.T.);
#5788=EDGE_CURVE('',#4473,#4488,#3048,.T.);
#5789=EDGE_CURVE('',#4488,#4488,#1881,.T.);
#5790=EDGE_CURVE('',#4456,#4482,#3049,.T.);
#5791=EDGE_CURVE('',#4484,#4489,#3050,.T.);
#5792=EDGE_CURVE('',#4489,#4489,#1882,.T.);
#5793=EDGE_CURVE('',#4490,#4491,#3051,.T.);
#5794=EDGE_CURVE('',#4491,#4466,#3052,.T.);
#5795=EDGE_CURVE('',#4490,#4469,#3053,.T.);
#5796=EDGE_CURVE('',#4492,#4490,#3054,.T.);
#5797=EDGE_CURVE('',#4492,#4468,#3055,.T.);
#5798=EDGE_CURVE('',#4493,#4492,#3056,.T.);
#5799=EDGE_CURVE('',#4493,#4467,#3057,.T.);
#5800=EDGE_CURVE('',#4491,#4493,#3058,.T.);
#5801=EDGE_CURVE('',#4494,#4494,#1883,.T.);
#5802=EDGE_CURVE('',#4495,#4495,#1884,.T.);
#5803=EDGE_CURVE('',#4494,#4496,#3059,.T.);
#5804=EDGE_CURVE('',#4496,#4496,#1885,.T.);
#5805=EDGE_CURVE('',#4497,#4497,#1886,.T.);
#5806=EDGE_CURVE('',#4498,#4498,#1887,.T.);
#5807=EDGE_CURVE('',#4498,#4497,#3060,.T.);
#5808=EDGE_CURVE('',#4499,#4499,#1888,.T.);
#5809=EDGE_CURVE('',#4499,#4495,#3061,.T.);
#5810=EDGE_CURVE('',#4500,#4501,#3062,.T.);
#5811=EDGE_CURVE('',#4501,#4502,#2282,.T.);
#5812=EDGE_CURVE('',#4502,#4503,#1889,.T.);
#5813=EDGE_CURVE('',#4503,#4504,#2283,.T.);
#5814=EDGE_CURVE('',#4504,#4505,#3063,.T.);
#5815=EDGE_CURVE('',#4505,#4505,#1890,.F.);
#5816=EDGE_CURVE('',#4504,#4500,#2284,.T.);
#5817=EDGE_CURVE('',#4506,#4507,#3064,.T.);
#5818=EDGE_CURVE('',#4507,#4501,#2285,.T.);
#5819=EDGE_CURVE('',#4500,#4506,#2286,.T.);
#5820=EDGE_CURVE('',#4508,#4509,#3065,.T.);
#5821=EDGE_CURVE('',#4509,#4507,#2287,.T.);
#5822=EDGE_CURVE('',#4506,#4508,#2288,.T.);
#5823=EDGE_CURVE('',#4510,#4511,#3066,.T.);
#5824=EDGE_CURVE('',#4511,#4509,#2289,.T.);
#5825=EDGE_CURVE('',#4508,#4510,#2290,.T.);
#5826=EDGE_CURVE('',#4512,#4513,#3067,.T.);
#5827=EDGE_CURVE('',#4513,#4511,#2291,.T.);
#5828=EDGE_CURVE('',#4510,#4512,#2292,.T.);
#5829=EDGE_CURVE('',#4514,#4515,#3068,.T.);
#5830=EDGE_CURVE('',#4515,#4513,#2293,.T.);
#5831=EDGE_CURVE('',#4512,#4514,#2294,.T.);
#5832=EDGE_CURVE('',#4516,#4517,#3069,.T.);
#5833=EDGE_CURVE('',#4517,#4515,#2295,.T.);
#5834=EDGE_CURVE('',#4514,#4516,#2296,.T.);
#5835=EDGE_CURVE('',#4518,#4519,#3070,.T.);
#5836=EDGE_CURVE('',#4519,#4517,#2297,.T.);
#5837=EDGE_CURVE('',#4516,#4518,#2298,.T.);
#5838=EDGE_CURVE('',#4520,#4521,#3071,.T.);
#5839=EDGE_CURVE('',#4521,#4519,#2299,.T.);
#5840=EDGE_CURVE('',#4518,#4520,#2300,.T.);
#5841=EDGE_CURVE('',#4522,#4523,#3072,.T.);
#5842=EDGE_CURVE('',#4523,#4521,#2301,.T.);
#5843=EDGE_CURVE('',#4520,#4522,#2302,.T.);
#5844=EDGE_CURVE('',#4524,#4525,#3073,.T.);
#5845=EDGE_CURVE('',#4525,#4523,#2303,.T.);
#5846=EDGE_CURVE('',#4522,#4524,#2304,.T.);
#5847=EDGE_CURVE('',#4526,#4527,#3074,.T.);
#5848=EDGE_CURVE('',#4526,#4528,#2305,.T.);
#5849=EDGE_CURVE('',#4529,#4528,#1891,.T.);
#5850=EDGE_CURVE('',#4529,#4527,#2306,.T.);
#5851=EDGE_CURVE('',#4530,#4531,#3075,.T.);
#5852=EDGE_CURVE('',#4531,#4532,#2307,.T.);
#5853=EDGE_CURVE('',#4533,#4532,#1892,.T.);
#5854=EDGE_CURVE('',#4530,#4533,#2308,.T.);
#5855=EDGE_CURVE('',#4534,#4535,#3076,.T.);
#5856=EDGE_CURVE('',#4535,#4531,#2309,.T.);
#5857=EDGE_CURVE('',#4534,#4530,#2310,.T.);
#5858=EDGE_CURVE('',#4536,#4537,#3077,.T.);
#5859=EDGE_CURVE('',#4537,#4535,#2311,.T.);
#5860=EDGE_CURVE('',#4536,#4534,#2312,.T.);
#5861=EDGE_CURVE('',#4538,#4539,#3078,.T.);
#5862=EDGE_CURVE('',#4539,#4537,#2313,.T.);
#5863=EDGE_CURVE('',#4538,#4536,#2314,.T.);
#5864=EDGE_CURVE('',#4540,#4541,#3079,.T.);
#5865=EDGE_CURVE('',#4541,#4539,#2315,.T.);
#5866=EDGE_CURVE('',#4540,#4538,#2316,.T.);
#5867=EDGE_CURVE('',#4542,#4543,#3080,.T.);
#5868=EDGE_CURVE('',#4543,#4541,#2317,.T.);
#5869=EDGE_CURVE('',#4542,#4540,#2318,.T.);
#5870=EDGE_CURVE('',#4544,#4545,#3081,.T.);
#5871=EDGE_CURVE('',#4545,#4543,#2319,.T.);
#5872=EDGE_CURVE('',#4544,#4542,#2320,.T.);
#5873=EDGE_CURVE('',#4546,#4547,#3082,.T.);
#5874=EDGE_CURVE('',#4547,#4545,#2321,.T.);
#5875=EDGE_CURVE('',#4546,#4544,#2322,.T.);
#5876=EDGE_CURVE('',#4548,#4549,#3083,.T.);
#5877=EDGE_CURVE('',#4549,#4547,#2323,.T.);
#5878=EDGE_CURVE('',#4548,#4546,#2324,.T.);
#5879=EDGE_CURVE('',#4550,#4551,#3084,.T.);
#5880=EDGE_CURVE('',#4551,#4549,#2325,.T.);
#5881=EDGE_CURVE('',#4550,#4548,#2326,.T.);
#5882=EDGE_CURVE('',#4552,#4553,#3085,.T.);
#5883=EDGE_CURVE('',#4553,#4551,#2327,.T.);
#5884=EDGE_CURVE('',#4552,#4550,#2328,.T.);
#5885=EDGE_CURVE('',#4554,#4555,#3086,.T.);
#5886=EDGE_CURVE('',#4555,#4553,#2329,.T.);
#5887=EDGE_CURVE('',#4554,#4552,#2330,.T.);
#5888=EDGE_CURVE('',#4556,#4557,#3087,.T.);
#5889=EDGE_CURVE('',#4558,#4556,#2331,.T.);
#5890=EDGE_CURVE('',#4559,#4558,#1893,.T.);
#5891=EDGE_CURVE('',#4559,#4557,#2332,.T.);
#5892=EDGE_CURVE('',#4560,#4561,#3088,.T.);
#5893=EDGE_CURVE('',#4561,#4562,#2333,.T.);
#5894=EDGE_CURVE('',#4563,#4562,#1894,.F.);
#5895=EDGE_CURVE('',#4563,#4560,#2334,.T.);
#5896=EDGE_CURVE('',#4564,#4565,#3089,.T.);
#5897=EDGE_CURVE('',#4565,#4561,#2335,.T.);
#5898=EDGE_CURVE('',#4560,#4564,#2336,.T.);
#5899=EDGE_CURVE('',#4566,#4567,#3090,.T.);
#5900=EDGE_CURVE('',#4567,#4565,#2337,.T.);
#5901=EDGE_CURVE('',#4564,#4566,#2338,.T.);
#5902=EDGE_CURVE('',#4568,#4569,#3091,.T.);
#5903=EDGE_CURVE('',#4569,#4567,#2339,.T.);
#5904=EDGE_CURVE('',#4566,#4568,#2340,.T.);
#5905=EDGE_CURVE('',#4570,#4571,#3092,.T.);
#5906=EDGE_CURVE('',#4571,#4569,#2341,.T.);
#5907=EDGE_CURVE('',#4568,#4570,#2342,.T.);
#5908=EDGE_CURVE('',#4572,#4573,#3093,.T.);
#5909=EDGE_CURVE('',#4573,#4571,#2343,.T.);
#5910=EDGE_CURVE('',#4570,#4572,#2344,.T.);
#5911=EDGE_CURVE('',#4574,#4575,#3094,.T.);
#5912=EDGE_CURVE('',#4575,#4573,#2345,.T.);
#5913=EDGE_CURVE('',#4572,#4574,#2346,.T.);
#5914=EDGE_CURVE('',#4576,#4577,#3095,.T.);
#5915=EDGE_CURVE('',#4576,#4578,#2347,.T.);
#5916=EDGE_CURVE('',#4579,#4578,#1895,.T.);
#5917=EDGE_CURVE('',#4579,#4577,#2348,.T.);
#5918=EDGE_CURVE('',#4580,#4581,#3096,.T.);
#5919=EDGE_CURVE('',#4581,#4582,#2349,.T.);
#5920=EDGE_CURVE('',#4583,#4582,#1896,.F.);
#5921=EDGE_CURVE('',#4583,#4580,#2350,.T.);
#5922=EDGE_CURVE('',#4584,#4585,#3097,.T.);
#5923=EDGE_CURVE('',#4585,#4581,#2351,.T.);
#5924=EDGE_CURVE('',#4580,#4584,#2352,.T.);
#5925=EDGE_CURVE('',#4586,#4587,#3098,.T.);
#5926=EDGE_CURVE('',#4587,#4585,#2353,.T.);
#5927=EDGE_CURVE('',#4584,#4586,#2354,.T.);
#5928=EDGE_CURVE('',#4588,#4589,#3099,.T.);
#5929=EDGE_CURVE('',#4589,#4587,#2355,.T.);
#5930=EDGE_CURVE('',#4586,#4588,#2356,.T.);
#5931=EDGE_CURVE('',#4590,#4591,#3100,.T.);
#5932=EDGE_CURVE('',#4591,#4589,#2357,.T.);
#5933=EDGE_CURVE('',#4588,#4590,#2358,.T.);
#5934=EDGE_CURVE('',#4592,#4593,#3101,.T.);
#5935=EDGE_CURVE('',#4593,#4591,#2359,.T.);
#5936=EDGE_CURVE('',#4590,#4592,#2360,.T.);
#5937=EDGE_CURVE('',#4594,#4595,#3102,.T.);
#5938=EDGE_CURVE('',#4595,#4593,#2361,.T.);
#5939=EDGE_CURVE('',#4592,#4594,#2362,.T.);
#5940=EDGE_CURVE('',#4596,#4597,#3103,.T.);
#5941=EDGE_CURVE('',#4596,#4598,#2363,.T.);
#5942=EDGE_CURVE('',#4599,#4598,#1897,.T.);
#5943=EDGE_CURVE('',#4599,#4597,#2364,.T.);
#5944=EDGE_CURVE('',#4600,#4601,#3104,.T.);
#5945=EDGE_CURVE('',#4601,#4602,#2365,.T.);
#5946=EDGE_CURVE('',#4603,#4602,#1898,.T.);
#5947=EDGE_CURVE('',#4600,#4603,#2366,.T.);
#5948=EDGE_CURVE('',#4604,#4605,#3105,.T.);
#5949=EDGE_CURVE('',#4605,#4601,#2367,.T.);
#5950=EDGE_CURVE('',#4604,#4600,#2368,.T.);
#5951=EDGE_CURVE('',#4606,#4607,#3106,.T.);
#5952=EDGE_CURVE('',#4607,#4605,#2369,.T.);
#5953=EDGE_CURVE('',#4606,#4604,#2370,.T.);
#5954=EDGE_CURVE('',#4608,#4609,#3107,.T.);
#5955=EDGE_CURVE('',#4609,#4607,#2371,.T.);
#5956=EDGE_CURVE('',#4608,#4606,#2372,.T.);
#5957=EDGE_CURVE('',#4610,#4611,#3108,.T.);
#5958=EDGE_CURVE('',#4611,#4609,#2373,.T.);
#5959=EDGE_CURVE('',#4610,#4608,#2374,.T.);
#5960=EDGE_CURVE('',#4612,#4613,#3109,.T.);
#5961=EDGE_CURVE('',#4613,#4611,#2375,.T.);
#5962=EDGE_CURVE('',#4612,#4610,#2376,.T.);
#5963=EDGE_CURVE('',#4614,#4615,#3110,.T.);
#5964=EDGE_CURVE('',#4615,#4613,#2377,.T.);
#5965=EDGE_CURVE('',#4614,#4612,#2378,.T.);
#5966=EDGE_CURVE('',#4616,#4617,#3111,.T.);
#5967=EDGE_CURVE('',#4618,#4616,#2379,.T.);
#5968=EDGE_CURVE('',#4619,#4618,#1899,.T.);
#5969=EDGE_CURVE('',#4619,#4617,#2380,.T.);
#5970=EDGE_CURVE('',#4620,#4621,#3112,.T.);
#5971=EDGE_CURVE('',#4621,#4622,#2381,.T.);
#5972=EDGE_CURVE('',#4623,#4622,#1900,.T.);
#5973=EDGE_CURVE('',#4620,#4623,#2382,.T.);
#5974=EDGE_CURVE('',#4624,#4625,#3113,.T.);
#5975=EDGE_CURVE('',#4625,#4621,#2383,.T.);
#5976=EDGE_CURVE('',#4624,#4620,#2384,.T.);
#5977=EDGE_CURVE('',#4626,#4627,#3114,.T.);
#5978=EDGE_CURVE('',#4627,#4625,#2385,.T.);
#5979=EDGE_CURVE('',#4626,#4624,#2386,.T.);
#5980=EDGE_CURVE('',#4628,#4629,#3115,.T.);
#5981=EDGE_CURVE('',#4629,#4627,#2387,.T.);
#5982=EDGE_CURVE('',#4628,#4626,#2388,.T.);
#5983=EDGE_CURVE('',#4630,#4631,#3116,.T.);
#5984=EDGE_CURVE('',#4631,#4629,#2389,.T.);
#5985=EDGE_CURVE('',#4630,#4628,#2390,.T.);
#5986=EDGE_CURVE('',#4632,#4633,#3117,.T.);
#5987=EDGE_CURVE('',#4633,#4631,#2391,.T.);
#5988=EDGE_CURVE('',#4632,#4630,#2392,.T.);
#5989=EDGE_CURVE('',#4634,#4635,#3118,.T.);
#5990=EDGE_CURVE('',#4635,#4633,#2393,.T.);
#5991=EDGE_CURVE('',#4634,#4632,#2394,.T.);
#5992=EDGE_CURVE('',#4636,#4637,#3119,.T.);
#5993=EDGE_CURVE('',#4638,#4636,#2395,.T.);
#5994=EDGE_CURVE('',#4639,#4638,#1901,.T.);
#5995=EDGE_CURVE('',#4639,#4637,#2396,.T.);
#5996=EDGE_CURVE('',#4637,#4635,#2397,.T.);
#5997=EDGE_CURVE('',#4636,#4634,#2398,.T.);
#5998=EDGE_CURVE('',#4622,#4583,#2399,.T.);
#5999=EDGE_CURVE('',#4598,#4639,#2400,.T.);
#6000=EDGE_CURVE('',#4594,#4596,#2401,.T.);
#6001=EDGE_CURVE('',#4582,#4623,#2402,.T.);
#6002=EDGE_CURVE('',#4597,#4595,#2403,.T.);
#6003=EDGE_CURVE('',#4638,#4599,#2404,.T.);
#6004=EDGE_CURVE('',#4640,#4641,#1902,.T.);
#6005=EDGE_CURVE('',#4642,#4640,#3120,.T.);
#6006=EDGE_CURVE('',#4643,#4642,#3121,.T.);
#6007=EDGE_CURVE('',#4644,#4643,#3122,.T.);
#6008=EDGE_CURVE('',#4645,#4644,#3123,.T.);
#6009=EDGE_CURVE('',#4641,#4645,#3124,.T.);
#6010=EDGE_CURVE('',#4562,#4603,#2405,.T.);
#6011=EDGE_CURVE('',#4602,#4563,#2406,.T.);
#6012=EDGE_CURVE('',#4617,#4615,#2407,.T.);
#6013=EDGE_CURVE('',#4616,#4614,#2408,.T.);
#6014=EDGE_CURVE('',#4578,#4619,#2409,.T.);
#6015=EDGE_CURVE('',#4574,#4576,#2410,.T.);
#6016=EDGE_CURVE('',#4577,#4575,#2411,.T.);
#6017=EDGE_CURVE('',#4618,#4579,#2412,.T.);
#6018=EDGE_CURVE('',#4502,#4533,#2413,.T.);
#6019=EDGE_CURVE('',#4532,#4503,#2414,.T.);
#6020=EDGE_CURVE('',#4557,#4555,#2415,.T.);
#6021=EDGE_CURVE('',#4556,#4554,#2416,.T.);
#6022=EDGE_CURVE('',#4528,#4559,#2417,.T.);
#6023=EDGE_CURVE('',#4524,#4526,#2418,.T.);
#6024=EDGE_CURVE('',#4527,#4525,#2419,.T.);
#6025=EDGE_CURVE('',#4558,#4529,#2420,.T.);
#6026=EDGE_CURVE('',#4646,#4646,#1903,.T.);
#6027=EDGE_CURVE('',#4646,#4647,#1904,.T.);
#6028=EDGE_CURVE('',#4647,#4647,#1905,.T.);
#6029=EDGE_CURVE('',#4647,#4648,#3125,.T.);
#6030=EDGE_CURVE('',#4648,#4648,#1906,.T.);
#6031=EDGE_CURVE('',#4648,#4649,#1907,.T.);
#6032=EDGE_CURVE('',#4649,#4649,#1908,.T.);
#6033=EDGE_CURVE('',#4649,#4650,#3126,.T.);
#6034=EDGE_CURVE('',#4650,#4650,#1909,.T.);
#6035=EDGE_CURVE('',#4651,#4651,#1910,.T.);
#6036=EDGE_CURVE('',#4652,#4652,#1911,.T.);
#6037=EDGE_CURVE('',#4653,#4653,#1912,.T.);
#6038=EDGE_CURVE('',#4654,#4654,#1913,.T.);
#6039=EDGE_CURVE('',#4651,#4653,#3127,.T.);
#6040=EDGE_CURVE('',#4654,#4646,#3128,.T.);
#6041=EDGE_CURVE('',#4641,#4655,#3129,.T.);
#6042=EDGE_CURVE('',#4645,#4656,#3130,.T.);
#6043=EDGE_CURVE('',#4655,#4656,#3131,.T.);
#6044=EDGE_CURVE('',#4643,#4657,#3132,.T.);
#6045=EDGE_CURVE('',#4658,#4657,#3133,.T.);
#6046=EDGE_CURVE('',#4644,#4658,#3134,.T.);
#6047=EDGE_CURVE('',#4656,#4658,#3135,.T.);
#6048=EDGE_CURVE('',#4659,#4640,#3136,.T.);
#6049=EDGE_CURVE('',#4660,#4659,#3137,.T.);
#6050=EDGE_CURVE('',#4642,#4660,#3138,.T.);
#6051=EDGE_CURVE('',#4657,#4660,#3139,.T.);
#6052=EDGE_CURVE('',#4659,#4655,#1914,.T.);
#6053=EDGE_CURVE('',#4661,#4661,#1915,.T.);
#6054=EDGE_CURVE('',#4661,#4652,#3140,.T.);
#6055=EDGE_CURVE('',#4662,#4662,#1916,.T.);
#6056=EDGE_CURVE('',#4662,#4663,#1917,.T.);
#6057=EDGE_CURVE('',#4663,#4663,#1918,.T.);
#6058=EDGE_CURVE('',#4663,#4664,#3141,.T.);
#6059=EDGE_CURVE('',#4664,#4664,#1919,.T.);
#6060=EDGE_CURVE('',#4665,#4665,#1920,.T.);
#6061=EDGE_CURVE('',#4664,#4666,#1921,.T.);
#6062=EDGE_CURVE('',#4666,#4666,#1922,.T.);
#6063=EDGE_CURVE('',#4667,#4667,#1923,.T.);
#6064=EDGE_CURVE('',#4668,#4668,#1924,.T.);
#6065=EDGE_CURVE('',#4669,#4669,#1925,.T.);
#6066=EDGE_CURVE('',#4665,#4668,#3142,.T.);
#6067=EDGE_CURVE('',#4670,#4670,#1926,.T.);
#6068=EDGE_CURVE('',#4671,#4671,#1927,.T.);
#6069=EDGE_CURVE('',#4669,#4671,#3143,.T.);
#6070=EDGE_CURVE('',#4670,#4672,#3144,.T.);
#6071=EDGE_CURVE('',#4672,#4672,#1928,.T.);
#6072=EDGE_CURVE('',#4667,#4673,#3145,.T.);
#6073=EDGE_CURVE('',#4673,#4673,#1929,.T.);
#6074=EDGE_CURVE('',#4674,#4674,#1930,.T.);
#6075=EDGE_CURVE('',#4674,#4675,#3146,.T.);
#6076=EDGE_CURVE('',#4675,#4675,#1931,.T.);
#6077=EDGE_CURVE('',#4676,#4676,#1932,.T.);
#6078=EDGE_CURVE('',#4676,#4677,#3147,.T.);
#6079=EDGE_CURVE('',#4677,#4677,#1933,.T.);
#6080=EDGE_CURVE('',#4678,#4679,#3148,.T.);
#6081=EDGE_CURVE('',#4679,#4680,#3149,.T.);
#6082=EDGE_CURVE('',#4681,#4680,#3150,.T.);
#6083=EDGE_CURVE('',#4678,#4681,#3151,.T.);
#6084=EDGE_CURVE('',#4682,#4678,#3152,.T.);
#6085=EDGE_CURVE('',#4683,#4681,#3153,.T.);
#6086=EDGE_CURVE('',#4682,#4683,#3154,.T.);
#6087=EDGE_CURVE('',#4684,#4682,#3155,.T.);
#6088=EDGE_CURVE('',#4685,#4683,#3156,.T.);
#6089=EDGE_CURVE('',#4684,#4685,#3157,.T.);
#6090=EDGE_CURVE('',#4679,#4684,#3158,.T.);
#6091=EDGE_CURVE('',#4680,#4685,#3159,.T.);
#6092=EDGE_CURVE('',#4686,#4686,#1934,.T.);
#6093=EDGE_CURVE('',#4686,#4687,#2421,.T.);
#6094=EDGE_CURVE('',#4687,#4687,#1935,.T.);
#6095=EDGE_CURVE('',#4688,#4689,#3160,.T.);
#6096=EDGE_CURVE('',#4689,#4690,#2422,.T.);
#6097=EDGE_CURVE('',#4690,#4691,#1936,.T.);
#6098=EDGE_CURVE('',#4691,#4692,#2423,.T.);
#6099=EDGE_CURVE('',#4692,#4693,#3161,.T.);
#6100=EDGE_CURVE('',#4693,#4693,#1937,.F.);
#6101=EDGE_CURVE('',#4692,#4688,#2424,.T.);
#6102=EDGE_CURVE('',#4694,#4695,#3162,.T.);
#6103=EDGE_CURVE('',#4695,#4689,#2425,.T.);
#6104=EDGE_CURVE('',#4688,#4694,#2426,.T.);
#6105=EDGE_CURVE('',#4696,#4697,#3163,.T.);
#6106=EDGE_CURVE('',#4697,#4695,#2427,.T.);
#6107=EDGE_CURVE('',#4694,#4696,#2428,.T.);
#6108=EDGE_CURVE('',#4698,#4699,#3164,.T.);
#6109=EDGE_CURVE('',#4699,#4697,#2429,.T.);
#6110=EDGE_CURVE('',#4696,#4698,#2430,.T.);
#6111=EDGE_CURVE('',#4700,#4701,#3165,.T.);
#6112=EDGE_CURVE('',#4701,#4699,#2431,.T.);
#6113=EDGE_CURVE('',#4698,#4700,#2432,.T.);
#6114=EDGE_CURVE('',#4702,#4703,#3166,.T.);
#6115=EDGE_CURVE('',#4703,#4701,#2433,.T.);
#6116=EDGE_CURVE('',#4700,#4702,#2434,.T.);
#6117=EDGE_CURVE('',#4704,#4705,#3167,.T.);
#6118=EDGE_CURVE('',#4705,#4703,#2435,.T.);
#6119=EDGE_CURVE('',#4702,#4704,#2436,.T.);
#6120=EDGE_CURVE('',#4706,#4707,#3168,.T.);
#6121=EDGE_CURVE('',#4707,#4705,#2437,.T.);
#6122=EDGE_CURVE('',#4704,#4706,#2438,.T.);
#6123=EDGE_CURVE('',#4708,#4709,#3169,.T.);
#6124=EDGE_CURVE('',#4709,#4707,#2439,.T.);
#6125=EDGE_CURVE('',#4706,#4708,#2440,.T.);
#6126=EDGE_CURVE('',#4710,#4711,#3170,.T.);
#6127=EDGE_CURVE('',#4711,#4709,#2441,.T.);
#6128=EDGE_CURVE('',#4708,#4710,#2442,.T.);
#6129=EDGE_CURVE('',#4712,#4713,#3171,.T.);
#6130=EDGE_CURVE('',#4713,#4711,#2443,.T.);
#6131=EDGE_CURVE('',#4710,#4712,#2444,.T.);
#6132=EDGE_CURVE('',#4714,#4715,#3172,.T.);
#6133=EDGE_CURVE('',#4714,#4716,#2445,.T.);
#6134=EDGE_CURVE('',#4717,#4716,#1938,.F.);
#6135=EDGE_CURVE('',#4717,#4715,#2446,.T.);
#6136=EDGE_CURVE('',#4718,#4719,#3173,.T.);
#6137=EDGE_CURVE('',#4719,#4720,#2447,.T.);
#6138=EDGE_CURVE('',#4721,#4720,#1939,.T.);
#6139=EDGE_CURVE('',#4718,#4721,#2448,.T.);
#6140=EDGE_CURVE('',#4722,#4723,#3174,.T.);
#6141=EDGE_CURVE('',#4723,#4719,#2449,.T.);
#6142=EDGE_CURVE('',#4722,#4718,#2450,.T.);
#6143=EDGE_CURVE('',#4724,#4725,#3175,.T.);
#6144=EDGE_CURVE('',#4725,#4723,#2451,.T.);
#6145=EDGE_CURVE('',#4724,#4722,#2452,.T.);
#6146=EDGE_CURVE('',#4726,#4727,#3176,.T.);
#6147=EDGE_CURVE('',#4727,#4725,#2453,.T.);
#6148=EDGE_CURVE('',#4726,#4724,#2454,.T.);
#6149=EDGE_CURVE('',#4728,#4729,#3177,.T.);
#6150=EDGE_CURVE('',#4729,#4727,#2455,.T.);
#6151=EDGE_CURVE('',#4728,#4726,#2456,.T.);
#6152=EDGE_CURVE('',#4730,#4731,#3178,.T.);
#6153=EDGE_CURVE('',#4731,#4729,#2457,.T.);
#6154=EDGE_CURVE('',#4730,#4728,#2458,.T.);
#6155=EDGE_CURVE('',#4732,#4733,#3179,.T.);
#6156=EDGE_CURVE('',#4733,#4731,#2459,.T.);
#6157=EDGE_CURVE('',#4732,#4730,#2460,.T.);
#6158=EDGE_CURVE('',#4734,#4735,#3180,.T.);
#6159=EDGE_CURVE('',#4735,#4733,#2461,.T.);
#6160=EDGE_CURVE('',#4734,#4732,#2462,.T.);
#6161=EDGE_CURVE('',#4736,#4737,#3181,.T.);
#6162=EDGE_CURVE('',#4737,#4735,#2463,.T.);
#6163=EDGE_CURVE('',#4736,#4734,#2464,.T.);
#6164=EDGE_CURVE('',#4738,#4739,#3182,.T.);
#6165=EDGE_CURVE('',#4739,#4737,#2465,.T.);
#6166=EDGE_CURVE('',#4738,#4736,#2466,.T.);
#6167=EDGE_CURVE('',#4740,#4741,#3183,.T.);
#6168=EDGE_CURVE('',#4741,#4739,#2467,.T.);
#6169=EDGE_CURVE('',#4740,#4738,#2468,.T.);
#6170=EDGE_CURVE('',#4742,#4743,#3184,.T.);
#6171=EDGE_CURVE('',#4743,#4741,#2469,.T.);
#6172=EDGE_CURVE('',#4742,#4740,#2470,.T.);
#6173=EDGE_CURVE('',#4744,#4745,#3185,.T.);
#6174=EDGE_CURVE('',#4746,#4744,#2471,.T.);
#6175=EDGE_CURVE('',#4747,#4746,#1940,.T.);
#6176=EDGE_CURVE('',#4747,#4745,#2472,.T.);
#6177=EDGE_CURVE('',#4748,#4749,#3186,.T.);
#6178=EDGE_CURVE('',#4749,#4750,#2473,.T.);
#6179=EDGE_CURVE('',#4750,#4751,#1941,.T.);
#6180=EDGE_CURVE('',#4751,#4752,#3187,.T.);
#6181=EDGE_CURVE('',#4752,#4752,#1942,.F.);
#6182=EDGE_CURVE('',#4751,#4753,#1943,.T.);
#6183=EDGE_CURVE('',#4753,#4748,#2474,.T.);
#6184=EDGE_CURVE('',#4754,#4755,#3188,.T.);
#6185=EDGE_CURVE('',#4755,#4749,#2475,.T.);
#6186=EDGE_CURVE('',#4748,#4754,#2476,.T.);
#6187=EDGE_CURVE('',#4756,#4757,#3189,.T.);
#6188=EDGE_CURVE('',#4757,#4755,#2477,.T.);
#6189=EDGE_CURVE('',#4754,#4756,#2478,.T.);
#6190=EDGE_CURVE('',#4758,#4759,#3190,.T.);
#6191=EDGE_CURVE('',#4759,#4757,#2479,.T.);
#6192=EDGE_CURVE('',#4756,#4758,#2480,.T.);
#6193=EDGE_CURVE('',#4760,#4761,#3191,.T.);
#6194=EDGE_CURVE('',#4761,#4759,#2481,.T.);
#6195=EDGE_CURVE('',#4758,#4760,#2482,.T.);
#6196=EDGE_CURVE('',#4762,#4763,#3192,.T.);
#6197=EDGE_CURVE('',#4763,#4761,#2483,.T.);
#6198=EDGE_CURVE('',#4760,#4762,#2484,.T.);
#6199=EDGE_CURVE('',#4764,#4765,#3193,.T.);
#6200=EDGE_CURVE('',#4765,#4763,#2485,.T.);
#6201=EDGE_CURVE('',#4762,#4764,#2486,.T.);
#6202=EDGE_CURVE('',#4766,#4767,#3194,.T.);
#6203=EDGE_CURVE('',#4767,#4765,#2487,.T.);
#6204=EDGE_CURVE('',#4764,#4766,#2488,.T.);
#6205=EDGE_CURVE('',#4768,#4769,#3195,.T.);
#6206=EDGE_CURVE('',#4769,#4767,#2489,.T.);
#6207=EDGE_CURVE('',#4766,#4768,#2490,.T.);
#6208=EDGE_CURVE('',#4770,#4771,#3196,.T.);
#6209=EDGE_CURVE('',#4771,#4769,#2491,.T.);
#6210=EDGE_CURVE('',#4768,#4770,#2492,.T.);
#6211=EDGE_CURVE('',#4772,#4773,#3197,.T.);
#6212=EDGE_CURVE('',#4773,#4771,#2493,.T.);
#6213=EDGE_CURVE('',#4770,#4772,#2494,.T.);
#6214=EDGE_CURVE('',#4774,#4775,#3198,.T.);
#6215=EDGE_CURVE('',#4775,#4773,#2495,.T.);
#6216=EDGE_CURVE('',#4772,#4774,#2496,.T.);
#6217=EDGE_CURVE('',#4776,#4777,#3199,.T.);
#6218=EDGE_CURVE('',#4777,#4775,#2497,.T.);
#6219=EDGE_CURVE('',#4774,#4776,#2498,.T.);
#6220=EDGE_CURVE('',#4778,#4779,#3200,.T.);
#6221=EDGE_CURVE('',#4779,#4777,#2499,.T.);
#6222=EDGE_CURVE('',#4776,#4778,#2500,.T.);
#6223=EDGE_CURVE('',#4780,#4781,#3201,.T.);
#6224=EDGE_CURVE('',#4781,#4779,#2501,.T.);
#6225=EDGE_CURVE('',#4778,#4780,#2502,.T.);
#6226=EDGE_CURVE('',#4782,#4783,#3202,.T.);
#6227=EDGE_CURVE('',#4783,#4781,#2503,.T.);
#6228=EDGE_CURVE('',#4780,#4782,#2504,.T.);
#6229=EDGE_CURVE('',#4784,#4785,#3203,.T.);
#6230=EDGE_CURVE('',#4785,#4783,#2505,.T.);
#6231=EDGE_CURVE('',#4782,#4784,#2506,.T.);
#6232=EDGE_CURVE('',#4786,#4787,#3204,.T.);
#6233=EDGE_CURVE('',#4786,#4788,#2507,.T.);
#6234=EDGE_CURVE('',#4789,#4788,#1944,.T.);
#6235=EDGE_CURVE('',#4789,#4787,#2508,.T.);
#6236=EDGE_CURVE('',#4790,#4791,#3205,.T.);
#6237=EDGE_CURVE('',#4791,#4792,#2509,.T.);
#6238=EDGE_CURVE('',#4793,#4792,#1945,.T.);
#6239=EDGE_CURVE('',#4790,#4793,#2510,.T.);
#6240=EDGE_CURVE('',#4794,#4795,#3206,.T.);
#6241=EDGE_CURVE('',#4795,#4791,#2511,.T.);
#6242=EDGE_CURVE('',#4794,#4790,#2512,.T.);
#6243=EDGE_CURVE('',#4796,#4797,#3207,.T.);
#6244=EDGE_CURVE('',#4797,#4795,#2513,.T.);
#6245=EDGE_CURVE('',#4796,#4794,#2514,.T.);
#6246=EDGE_CURVE('',#4798,#4799,#3208,.T.);
#6247=EDGE_CURVE('',#4799,#4797,#2515,.T.);
#6248=EDGE_CURVE('',#4798,#4796,#2516,.T.);
#6249=EDGE_CURVE('',#4800,#4801,#3209,.T.);
#6250=EDGE_CURVE('',#4801,#4799,#2517,.T.);
#6251=EDGE_CURVE('',#4800,#4798,#2518,.T.);
#6252=EDGE_CURVE('',#4802,#4803,#3210,.T.);
#6253=EDGE_CURVE('',#4803,#4801,#2519,.T.);
#6254=EDGE_CURVE('',#4802,#4800,#2520,.T.);
#6255=EDGE_CURVE('',#4804,#4805,#3211,.T.);
#6256=EDGE_CURVE('',#4805,#4803,#2521,.T.);
#6257=EDGE_CURVE('',#4804,#4802,#2522,.T.);
#6258=EDGE_CURVE('',#4806,#4807,#3212,.T.);
#6259=EDGE_CURVE('',#4807,#4805,#2523,.T.);
#6260=EDGE_CURVE('',#4806,#4804,#2524,.T.);
#6261=EDGE_CURVE('',#4808,#4809,#3213,.T.);
#6262=EDGE_CURVE('',#4809,#4807,#2525,.T.);
#6263=EDGE_CURVE('',#4808,#4806,#2526,.T.);
#6264=EDGE_CURVE('',#4810,#4811,#3214,.T.);
#6265=EDGE_CURVE('',#4811,#4809,#2527,.T.);
#6266=EDGE_CURVE('',#4810,#4808,#2528,.T.);
#6267=EDGE_CURVE('',#4812,#4813,#3215,.T.);
#6268=EDGE_CURVE('',#4813,#4811,#2529,.T.);
#6269=EDGE_CURVE('',#4812,#4810,#2530,.T.);
#6270=EDGE_CURVE('',#4814,#4815,#3216,.T.);
#6271=EDGE_CURVE('',#4815,#4813,#2531,.T.);
#6272=EDGE_CURVE('',#4814,#4812,#2532,.T.);
#6273=EDGE_CURVE('',#4816,#4817,#3217,.T.);
#6274=EDGE_CURVE('',#4817,#4815,#2533,.T.);
#6275=EDGE_CURVE('',#4816,#4814,#2534,.T.);
#6276=EDGE_CURVE('',#4818,#4819,#3218,.T.);
#6277=EDGE_CURVE('',#4819,#4817,#2535,.T.);
#6278=EDGE_CURVE('',#4818,#4816,#2536,.T.);
#6279=EDGE_CURVE('',#4820,#4821,#3219,.T.);
#6280=EDGE_CURVE('',#4821,#4819,#2537,.T.);
#6281=EDGE_CURVE('',#4820,#4818,#2538,.T.);
#6282=EDGE_CURVE('',#4822,#4823,#3220,.T.);
#6283=EDGE_CURVE('',#4823,#4821,#2539,.T.);
#6284=EDGE_CURVE('',#4822,#4820,#2540,.T.);
#6285=EDGE_CURVE('',#4824,#4825,#3221,.T.);
#6286=EDGE_CURVE('',#4825,#4823,#2541,.T.);
#6287=EDGE_CURVE('',#4824,#4822,#2542,.T.);
#6288=EDGE_CURVE('',#4826,#4827,#3222,.T.);
#6289=EDGE_CURVE('',#4828,#4826,#2543,.T.);
#6290=EDGE_CURVE('',#4829,#4828,#1946,.T.);
#6291=EDGE_CURVE('',#4829,#4827,#2544,.T.);
#6292=EDGE_CURVE('',#4750,#4793,#2545,.T.);
#6293=EDGE_CURVE('',#4792,#4753,#2546,.T.);
#6294=EDGE_CURVE('',#4827,#4825,#2547,.T.);
#6295=EDGE_CURVE('',#4826,#4824,#2548,.T.);
#6296=EDGE_CURVE('',#4788,#4829,#2549,.T.);
#6297=EDGE_CURVE('',#4784,#4786,#2550,.T.);
#6298=EDGE_CURVE('',#4787,#4785,#2551,.T.);
#6299=EDGE_CURVE('',#4828,#4789,#2552,.T.);
#6300=EDGE_CURVE('',#4690,#4721,#2553,.T.);
#6301=EDGE_CURVE('',#4720,#4691,#2554,.T.);
#6302=EDGE_CURVE('',#4745,#4743,#2555,.T.);
#6303=EDGE_CURVE('',#4744,#4742,#2556,.T.);
#6304=EDGE_CURVE('',#4716,#4747,#2557,.T.);
#6305=EDGE_CURVE('',#4712,#4714,#2558,.T.);
#6306=EDGE_CURVE('',#4715,#4713,#2559,.T.);
#6307=EDGE_CURVE('',#4746,#4717,#2560,.T.);
#6308=EDGE_CURVE('',#4830,#4831,#3223,.T.);
#6309=EDGE_CURVE('',#4831,#4832,#3224,.T.);
#6310=EDGE_CURVE('',#4833,#4832,#3225,.T.);
#6311=EDGE_CURVE('',#4830,#4833,#3226,.T.);
#6312=EDGE_CURVE('',#4834,#4830,#3227,.T.);
#6313=EDGE_CURVE('',#4835,#4833,#3228,.T.);
#6314=EDGE_CURVE('',#4834,#4835,#3229,.T.);
#6315=EDGE_CURVE('',#4836,#4834,#3230,.T.);
#6316=EDGE_CURVE('',#4837,#4835,#3231,.T.);
#6317=EDGE_CURVE('',#4836,#4837,#3232,.T.);
#6318=EDGE_CURVE('',#4831,#4836,#3233,.T.);
#6319=EDGE_CURVE('',#4832,#4837,#3234,.T.);
#6320=EDGE_CURVE('',#4838,#4839,#3235,.T.);
#6321=EDGE_CURVE('',#4839,#4840,#2561,.T.);
#6322=EDGE_CURVE('',#4840,#4841,#1947,.T.);
#6323=EDGE_CURVE('',#4841,#4842,#3236,.T.);
#6324=EDGE_CURVE('',#4842,#4842,#1948,.F.);
#6325=EDGE_CURVE('',#4841,#4843,#1949,.T.);
#6326=EDGE_CURVE('',#4843,#4838,#2562,.T.);
#6327=EDGE_CURVE('',#4844,#4845,#3237,.T.);
#6328=EDGE_CURVE('',#4845,#4839,#2563,.T.);
#6329=EDGE_CURVE('',#4838,#4844,#2564,.T.);
#6330=EDGE_CURVE('',#4846,#4847,#3238,.T.);
#6331=EDGE_CURVE('',#4847,#4845,#2565,.T.);
#6332=EDGE_CURVE('',#4844,#4846,#2566,.T.);
#6333=EDGE_CURVE('',#4848,#4849,#3239,.T.);
#6334=EDGE_CURVE('',#4849,#4847,#2567,.T.);
#6335=EDGE_CURVE('',#4846,#4848,#2568,.T.);
#6336=EDGE_CURVE('',#4850,#4851,#3240,.T.);
#6337=EDGE_CURVE('',#4851,#4849,#2569,.T.);
#6338=EDGE_CURVE('',#4848,#4850,#2570,.T.);
#6339=EDGE_CURVE('',#4852,#4853,#3241,.T.);
#6340=EDGE_CURVE('',#4853,#4851,#2571,.T.);
#6341=EDGE_CURVE('',#4850,#4852,#2572,.T.);
#6342=EDGE_CURVE('',#4854,#4855,#3242,.T.);
#6343=EDGE_CURVE('',#4855,#4853,#2573,.T.);
#6344=EDGE_CURVE('',#4852,#4854,#2574,.T.);
#6345=EDGE_CURVE('',#4856,#4857,#3243,.T.);
#6346=EDGE_CURVE('',#4857,#4855,#2575,.T.);
#6347=EDGE_CURVE('',#4854,#4856,#2576,.T.);
#6348=EDGE_CURVE('',#4858,#4859,#3244,.T.);
#6349=EDGE_CURVE('',#4859,#4857,#2577,.T.);
#6350=EDGE_CURVE('',#4856,#4858,#2578,.T.);
#6351=EDGE_CURVE('',#4860,#4861,#3245,.T.);
#6352=EDGE_CURVE('',#4860,#4862,#2579,.T.);
#6353=EDGE_CURVE('',#4863,#4862,#1950,.T.);
#6354=EDGE_CURVE('',#4863,#4861,#2580,.T.);
#6355=EDGE_CURVE('',#4864,#4865,#3246,.T.);
#6356=EDGE_CURVE('',#4865,#4866,#2581,.T.);
#6357=EDGE_CURVE('',#4867,#4866,#1951,.T.);
#6358=EDGE_CURVE('',#4864,#4867,#2582,.T.);
#6359=EDGE_CURVE('',#4868,#4869,#3247,.T.);
#6360=EDGE_CURVE('',#4869,#4865,#2583,.T.);
#6361=EDGE_CURVE('',#4868,#4864,#2584,.T.);
#6362=EDGE_CURVE('',#4870,#4871,#3248,.T.);
#6363=EDGE_CURVE('',#4871,#4869,#2585,.T.);
#6364=EDGE_CURVE('',#4870,#4868,#2586,.T.);
#6365=EDGE_CURVE('',#4872,#4873,#3249,.T.);
#6366=EDGE_CURVE('',#4873,#4871,#2587,.T.);
#6367=EDGE_CURVE('',#4872,#4870,#2588,.T.);
#6368=EDGE_CURVE('',#4874,#4875,#3250,.T.);
#6369=EDGE_CURVE('',#4875,#4873,#2589,.T.);
#6370=EDGE_CURVE('',#4874,#4872,#2590,.T.);
#6371=EDGE_CURVE('',#4876,#4877,#3251,.T.);
#6372=EDGE_CURVE('',#4877,#4875,#2591,.T.);
#6373=EDGE_CURVE('',#4876,#4874,#2592,.T.);
#6374=EDGE_CURVE('',#4878,#4879,#3252,.T.);
#6375=EDGE_CURVE('',#4879,#4877,#2593,.T.);
#6376=EDGE_CURVE('',#4878,#4876,#2594,.T.);
#6377=EDGE_CURVE('',#4880,#4881,#3253,.T.);
#6378=EDGE_CURVE('',#4881,#4879,#2595,.T.);
#6379=EDGE_CURVE('',#4880,#4878,#2596,.T.);
#6380=EDGE_CURVE('',#4882,#4883,#3254,.T.);
#6381=EDGE_CURVE('',#4883,#4881,#2597,.T.);
#6382=EDGE_CURVE('',#4882,#4880,#2598,.T.);
#6383=EDGE_CURVE('',#4884,#4885,#3255,.T.);
#6384=EDGE_CURVE('',#4886,#4884,#2599,.T.);
#6385=EDGE_CURVE('',#4887,#4886,#1952,.T.);
#6386=EDGE_CURVE('',#4887,#4885,#2600,.T.);
#6387=EDGE_CURVE('',#4840,#4867,#2601,.T.);
#6388=EDGE_CURVE('',#4866,#4843,#2602,.T.);
#6389=EDGE_CURVE('',#4885,#4883,#2603,.T.);
#6390=EDGE_CURVE('',#4884,#4882,#2604,.T.);
#6391=EDGE_CURVE('',#4862,#4887,#2605,.T.);
#6392=EDGE_CURVE('',#4858,#4860,#2606,.T.);
#6393=EDGE_CURVE('',#4861,#4859,#2607,.T.);
#6394=EDGE_CURVE('',#4886,#4863,#2608,.T.);
#6395=EDGE_CURVE('',#4888,#4888,#1953,.T.);
#6396=EDGE_CURVE('',#4888,#4889,#3256,.T.);
#6397=EDGE_CURVE('',#4889,#4889,#1954,.T.);
#6398=EDGE_CURVE('',#4890,#4891,#3257,.T.);
#6399=EDGE_CURVE('',#4891,#4892,#3258,.T.);
#6400=EDGE_CURVE('',#4893,#4892,#3259,.T.);
#6401=EDGE_CURVE('',#4890,#4893,#3260,.T.);
#6402=EDGE_CURVE('',#4894,#4895,#3261,.T.);
#6403=EDGE_CURVE('',#4891,#4894,#3262,.T.);
#6404=EDGE_CURVE('',#4895,#4890,#3263,.T.);
#6405=EDGE_CURVE('',#4892,#4896,#3264,.T.);
#6406=EDGE_CURVE('',#4897,#4894,#3265,.T.);
#6407=EDGE_CURVE('',#4897,#4898,#3266,.T.);
#6408=EDGE_CURVE('',#4898,#4896,#3267,.T.);
#6409=EDGE_CURVE('',#4899,#4895,#3268,.T.);
#6410=EDGE_CURVE('',#4899,#4897,#3269,.T.);
#6411=EDGE_CURVE('',#4900,#4893,#3270,.T.);
#6412=EDGE_CURVE('',#4901,#4900,#3271,.T.);
#6413=EDGE_CURVE('',#4901,#4899,#3272,.T.);
#6414=EDGE_CURVE('',#4898,#4901,#3273,.T.);
#6415=EDGE_CURVE('',#4896,#4900,#3274,.T.);
#6416=EDGE_CURVE('',#4902,#4902,#1955,.T.);
#6417=EDGE_CURVE('',#4902,#4903,#3275,.T.);
#6418=EDGE_CURVE('',#4903,#4903,#1956,.T.);
#6419=EDGE_CURVE('',#4904,#4905,#3276,.T.);
#6420=EDGE_CURVE('',#4905,#4906,#3277,.T.);
#6421=EDGE_CURVE('',#4907,#4906,#3278,.T.);
#6422=EDGE_CURVE('',#4904,#4907,#3279,.T.);
#6423=EDGE_CURVE('',#4908,#4904,#3280,.T.);
#6424=EDGE_CURVE('',#4909,#4907,#3281,.T.);
#6425=EDGE_CURVE('',#4908,#4909,#3282,.T.);
#6426=EDGE_CURVE('',#4910,#4908,#3283,.T.);
#6427=EDGE_CURVE('',#4911,#4909,#3284,.T.);
#6428=EDGE_CURVE('',#4910,#4911,#3285,.T.);
#6429=EDGE_CURVE('',#4905,#4910,#3286,.T.);
#6430=EDGE_CURVE('',#4906,#4911,#3287,.T.);
#6431=EDGE_CURVE('',#4912,#4913,#1957,.T.);
#6432=EDGE_CURVE('',#4914,#4914,#1958,.T.);
#6433=EDGE_CURVE('',#4915,#4915,#1959,.T.);
#6434=EDGE_CURVE('',#4916,#4916,#1960,.T.);
#6435=EDGE_CURVE('',#4916,#4914,#3288,.T.);
#6436=EDGE_CURVE('',#4915,#4917,#3289,.T.);
#6437=EDGE_CURVE('',#4917,#4917,#1961,.T.);
#6438=EDGE_CURVE('',#4918,#4918,#1962,.T.);
#6439=EDGE_CURVE('',#4918,#4919,#2609,.T.);
#6440=EDGE_CURVE('',#4919,#4919,#1963,.T.);
#6441=EDGE_CURVE('',#4920,#4921,#3290,.T.);
#6442=EDGE_CURVE('',#4920,#4922,#2610,.T.);
#6443=EDGE_CURVE('',#4922,#4923,#1964,.F.);
#6444=EDGE_CURVE('',#4923,#4921,#2611,.T.);
#6445=EDGE_CURVE('',#4924,#4925,#3291,.T.);
#6446=EDGE_CURVE('',#4924,#4920,#2612,.T.);
#6447=EDGE_CURVE('',#4921,#4925,#2613,.T.);
#6448=EDGE_CURVE('',#4926,#4927,#3292,.T.);
#6449=EDGE_CURVE('',#4926,#4924,#2614,.T.);
#6450=EDGE_CURVE('',#4925,#4927,#2615,.T.);
#6451=EDGE_CURVE('',#4928,#4929,#3293,.T.);
#6452=EDGE_CURVE('',#4928,#4926,#2616,.T.);
#6453=EDGE_CURVE('',#4927,#4929,#2617,.T.);
#6454=EDGE_CURVE('',#4930,#4931,#3294,.T.);
#6455=EDGE_CURVE('',#4930,#4928,#2618,.T.);
#6456=EDGE_CURVE('',#4929,#4931,#2619,.T.);
#6457=EDGE_CURVE('',#4932,#4933,#3295,.T.);
#6458=EDGE_CURVE('',#4932,#4930,#2620,.T.);
#6459=EDGE_CURVE('',#4931,#4933,#2621,.T.);
#6460=EDGE_CURVE('',#4934,#4935,#3296,.T.);
#6461=EDGE_CURVE('',#4934,#4932,#2622,.T.);
#6462=EDGE_CURVE('',#4933,#4935,#2623,.T.);
#6463=EDGE_CURVE('',#4936,#4937,#3297,.T.);
#6464=EDGE_CURVE('',#4936,#4934,#2624,.T.);
#6465=EDGE_CURVE('',#4935,#4937,#2625,.T.);
#6466=EDGE_CURVE('',#4938,#4939,#3298,.T.);
#6467=EDGE_CURVE('',#4938,#4936,#2626,.T.);
#6468=EDGE_CURVE('',#4937,#4939,#2627,.T.);
#6469=EDGE_CURVE('',#4940,#4941,#3299,.T.);
#6470=EDGE_CURVE('',#4940,#4938,#2628,.T.);
#6471=EDGE_CURVE('',#4939,#4941,#2629,.T.);
#6472=EDGE_CURVE('',#4942,#4943,#3300,.T.);
#6473=EDGE_CURVE('',#4942,#4940,#2630,.T.);
#6474=EDGE_CURVE('',#4941,#4943,#2631,.T.);
#6475=EDGE_CURVE('',#4944,#4945,#3301,.T.);
#6476=EDGE_CURVE('',#4944,#4942,#2632,.T.);
#6477=EDGE_CURVE('',#4943,#4945,#2633,.T.);
#6478=EDGE_CURVE('',#4946,#4947,#3302,.T.);
#6479=EDGE_CURVE('',#4946,#4944,#2634,.T.);
#6480=EDGE_CURVE('',#4945,#4947,#2635,.T.);
#6481=EDGE_CURVE('',#4948,#4949,#3303,.T.);
#6482=EDGE_CURVE('',#4948,#4946,#2636,.T.);
#6483=EDGE_CURVE('',#4947,#4949,#2637,.T.);
#6484=EDGE_CURVE('',#4950,#4951,#3304,.T.);
#6485=EDGE_CURVE('',#4950,#4948,#2638,.T.);
#6486=EDGE_CURVE('',#4949,#4951,#2639,.T.);
#6487=EDGE_CURVE('',#4952,#4953,#3305,.T.);
#6488=EDGE_CURVE('',#4952,#4950,#2640,.T.);
#6489=EDGE_CURVE('',#4951,#4953,#2641,.T.);
#6490=EDGE_CURVE('',#4954,#4955,#3306,.T.);
#6491=EDGE_CURVE('',#4954,#4956,#2642,.T.);
#6492=EDGE_CURVE('',#4956,#4957,#1965,.T.);
#6493=EDGE_CURVE('',#4955,#4957,#2643,.T.);
#6494=EDGE_CURVE('',#4958,#4959,#3307,.T.);
#6495=EDGE_CURVE('',#4958,#4954,#2644,.T.);
#6496=EDGE_CURVE('',#4959,#4955,#2645,.T.);
#6497=EDGE_CURVE('',#4960,#4961,#3308,.T.);
#6498=EDGE_CURVE('',#4960,#4958,#2646,.T.);
#6499=EDGE_CURVE('',#4961,#4959,#2647,.T.);
#6500=EDGE_CURVE('',#4962,#4963,#3309,.T.);
#6501=EDGE_CURVE('',#4962,#4960,#2648,.T.);
#6502=EDGE_CURVE('',#4963,#4961,#2649,.T.);
#6503=EDGE_CURVE('',#4964,#4965,#3310,.T.);
#6504=EDGE_CURVE('',#4964,#4962,#2650,.T.);
#6505=EDGE_CURVE('',#4965,#4963,#2651,.T.);
#6506=EDGE_CURVE('',#4966,#4967,#3311,.T.);
#6507=EDGE_CURVE('',#4966,#4964,#2652,.T.);
#6508=EDGE_CURVE('',#4967,#4965,#2653,.T.);
#6509=EDGE_CURVE('',#4968,#4969,#3312,.T.);
#6510=EDGE_CURVE('',#4968,#4966,#2654,.T.);
#6511=EDGE_CURVE('',#4969,#4967,#2655,.T.);
#6512=EDGE_CURVE('',#4970,#4971,#3313,.T.);
#6513=EDGE_CURVE('',#4970,#4968,#2656,.T.);
#6514=EDGE_CURVE('',#4971,#4969,#2657,.T.);
#6515=EDGE_CURVE('',#4972,#4973,#3314,.T.);
#6516=EDGE_CURVE('',#4972,#4970,#2658,.T.);
#6517=EDGE_CURVE('',#4973,#4971,#2659,.T.);
#6518=EDGE_CURVE('',#4974,#4975,#3315,.T.);
#6519=EDGE_CURVE('',#4974,#4972,#2660,.T.);
#6520=EDGE_CURVE('',#4975,#4973,#2661,.T.);
#6521=EDGE_CURVE('',#4976,#4977,#3316,.T.);
#6522=EDGE_CURVE('',#4976,#4974,#2662,.T.);
#6523=EDGE_CURVE('',#4977,#4975,#2663,.T.);
#6524=EDGE_CURVE('',#4978,#4979,#3317,.T.);
#6525=EDGE_CURVE('',#4978,#4976,#2664,.T.);
#6526=EDGE_CURVE('',#4979,#4977,#2665,.T.);
#6527=EDGE_CURVE('',#4980,#4981,#3318,.T.);
#6528=EDGE_CURVE('',#4980,#4978,#2666,.T.);
#6529=EDGE_CURVE('',#4981,#4979,#2667,.T.);
#6530=EDGE_CURVE('',#4982,#4983,#3319,.T.);
#6531=EDGE_CURVE('',#4982,#4980,#2668,.T.);
#6532=EDGE_CURVE('',#4983,#4981,#2669,.T.);
#6533=EDGE_CURVE('',#4984,#4985,#3320,.T.);
#6534=EDGE_CURVE('',#4984,#4982,#2670,.T.);
#6535=EDGE_CURVE('',#4985,#4983,#2671,.T.);
#6536=EDGE_CURVE('',#4986,#4987,#3321,.T.);
#6537=EDGE_CURVE('',#4986,#4984,#2672,.T.);
#6538=EDGE_CURVE('',#4987,#4985,#2673,.T.);
#6539=EDGE_CURVE('',#4957,#4988,#2674,.T.);
#6540=EDGE_CURVE('',#4989,#4956,#2675,.T.);
#6541=EDGE_CURVE('',#4990,#4989,#1966,.T.);
#6542=EDGE_CURVE('',#4988,#4990,#2676,.T.);
#6543=EDGE_CURVE('',#4988,#4991,#3322,.T.);
#6544=EDGE_CURVE('',#4991,#4991,#1967,.T.);
#6545=EDGE_CURVE('',#4992,#4986,#2677,.T.);
#6546=EDGE_CURVE('',#4922,#4992,#2678,.T.);
#6547=EDGE_CURVE('',#4989,#4952,#2679,.T.);
#6548=EDGE_CURVE('',#4993,#4987,#2680,.T.);
#6549=EDGE_CURVE('',#4992,#4993,#1968,.T.);
#6550=EDGE_CURVE('',#4953,#4990,#2681,.T.);
#6551=EDGE_CURVE('',#4993,#4923,#2682,.T.);
#6552=EDGE_CURVE('',#4994,#4995,#3323,.T.);
#6553=EDGE_CURVE('',#4994,#4996,#3324,.T.);
#6554=EDGE_CURVE('',#4996,#4997,#3325,.T.);
#6555=EDGE_CURVE('',#4995,#4997,#3326,.T.);
#6556=EDGE_CURVE('',#4998,#4994,#3327,.T.);
#6557=EDGE_CURVE('',#4998,#4999,#3328,.T.);
#6558=EDGE_CURVE('',#4999,#4996,#3329,.T.);
#6559=EDGE_CURVE('',#5000,#4998,#3330,.T.);
#6560=EDGE_CURVE('',#5000,#5001,#3331,.T.);
#6561=EDGE_CURVE('',#5001,#4999,#3332,.T.);
#6562=EDGE_CURVE('',#5002,#5000,#3333,.T.);
#6563=EDGE_CURVE('',#5002,#5003,#3334,.T.);
#6564=EDGE_CURVE('',#5003,#5001,#3335,.T.);
#6565=EDGE_CURVE('',#5004,#5002,#3336,.T.);
#6566=EDGE_CURVE('',#5004,#5005,#3337,.T.);
#6567=EDGE_CURVE('',#5005,#5003,#3338,.T.);
#6568=EDGE_CURVE('',#4995,#5004,#3339,.T.);
#6569=EDGE_CURVE('',#4997,#5005,#3340,.T.);
#6570=EDGE_CURVE('',#5006,#5006,#1969,.T.);
#6571=EDGE_CURVE('',#5006,#5007,#3341,.T.);
#6572=EDGE_CURVE('',#5007,#5007,#1970,.T.);
#6573=EDGE_CURVE('',#5008,#5009,#3342,.T.);
#6574=EDGE_CURVE('',#5008,#5010,#2683,.T.);
#6575=EDGE_CURVE('',#5010,#5011,#1971,.F.);
#6576=EDGE_CURVE('',#5011,#5009,#2684,.T.);
#6577=EDGE_CURVE('',#5012,#5013,#3343,.T.);
#6578=EDGE_CURVE('',#5012,#5008,#2685,.T.);
#6579=EDGE_CURVE('',#5009,#5013,#2686,.T.);
#6580=EDGE_CURVE('',#5014,#5015,#3344,.T.);
#6581=EDGE_CURVE('',#5014,#5012,#2687,.T.);
#6582=EDGE_CURVE('',#5013,#5015,#2688,.T.);
#6583=EDGE_CURVE('',#5016,#5017,#3345,.T.);
#6584=EDGE_CURVE('',#5016,#5014,#2689,.T.);
#6585=EDGE_CURVE('',#5015,#5017,#2690,.T.);
#6586=EDGE_CURVE('',#5018,#5019,#3346,.T.);
#6587=EDGE_CURVE('',#5018,#5016,#2691,.T.);
#6588=EDGE_CURVE('',#5017,#5019,#2692,.T.);
#6589=EDGE_CURVE('',#5020,#5021,#3347,.T.);
#6590=EDGE_CURVE('',#5020,#5018,#2693,.T.);
#6591=EDGE_CURVE('',#5019,#5021,#2694,.T.);
#6592=EDGE_CURVE('',#5022,#5023,#3348,.T.);
#6593=EDGE_CURVE('',#5022,#5020,#2695,.T.);
#6594=EDGE_CURVE('',#5021,#5023,#2696,.T.);
#6595=EDGE_CURVE('',#5024,#5025,#3349,.T.);
#6596=EDGE_CURVE('',#5024,#5022,#2697,.T.);
#6597=EDGE_CURVE('',#5023,#5025,#2698,.T.);
#6598=EDGE_CURVE('',#5026,#5027,#3350,.T.);
#6599=EDGE_CURVE('',#5026,#5024,#2699,.T.);
#6600=EDGE_CURVE('',#5025,#5027,#2700,.T.);
#6601=EDGE_CURVE('',#5028,#5029,#3351,.T.);
#6602=EDGE_CURVE('',#5028,#5026,#2701,.T.);
#6603=EDGE_CURVE('',#5027,#5029,#2702,.T.);
#6604=EDGE_CURVE('',#5030,#5031,#3352,.T.);
#6605=EDGE_CURVE('',#5030,#5032,#2703,.T.);
#6606=EDGE_CURVE('',#5032,#5033,#1972,.T.);
#6607=EDGE_CURVE('',#5031,#5033,#2704,.T.);
#6608=EDGE_CURVE('',#5034,#5035,#3353,.T.);
#6609=EDGE_CURVE('',#5034,#5030,#2705,.T.);
#6610=EDGE_CURVE('',#5035,#5031,#2706,.T.);
#6611=EDGE_CURVE('',#5036,#5037,#3354,.T.);
#6612=EDGE_CURVE('',#5036,#5034,#2707,.T.);
#6613=EDGE_CURVE('',#5037,#5035,#2708,.T.);
#6614=EDGE_CURVE('',#5038,#5039,#3355,.T.);
#6615=EDGE_CURVE('',#5038,#5036,#2709,.T.);
#6616=EDGE_CURVE('',#5039,#5037,#2710,.T.);
#6617=EDGE_CURVE('',#5040,#5041,#3356,.T.);
#6618=EDGE_CURVE('',#5040,#5038,#2711,.T.);
#6619=EDGE_CURVE('',#5041,#5039,#2712,.T.);
#6620=EDGE_CURVE('',#5042,#5043,#3357,.T.);
#6621=EDGE_CURVE('',#5042,#5040,#2713,.T.);
#6622=EDGE_CURVE('',#5043,#5041,#2714,.T.);
#6623=EDGE_CURVE('',#5044,#5045,#3358,.T.);
#6624=EDGE_CURVE('',#5044,#5042,#2715,.T.);
#6625=EDGE_CURVE('',#5045,#5043,#2716,.T.);
#6626=EDGE_CURVE('',#5046,#5047,#3359,.T.);
#6627=EDGE_CURVE('',#5046,#5044,#2717,.T.);
#6628=EDGE_CURVE('',#5047,#5045,#2718,.T.);
#6629=EDGE_CURVE('',#5048,#5049,#3360,.T.);
#6630=EDGE_CURVE('',#5048,#5046,#2719,.T.);
#6631=EDGE_CURVE('',#5049,#5047,#2720,.T.);
#6632=EDGE_CURVE('',#5050,#5051,#3361,.T.);
#6633=EDGE_CURVE('',#5050,#5048,#2721,.T.);
#6634=EDGE_CURVE('',#5051,#5049,#2722,.T.);
#6635=EDGE_CURVE('',#5033,#5052,#2723,.T.);
#6636=EDGE_CURVE('',#5053,#5032,#2724,.T.);
#6637=EDGE_CURVE('',#5054,#5053,#1973,.T.);
#6638=EDGE_CURVE('',#5052,#5054,#2725,.T.);
#6639=EDGE_CURVE('',#5052,#5055,#3362,.T.);
#6640=EDGE_CURVE('',#5055,#5055,#1974,.T.);
#6641=EDGE_CURVE('',#5056,#5050,#2726,.T.);
#6642=EDGE_CURVE('',#5010,#5056,#2727,.T.);
#6643=EDGE_CURVE('',#5053,#5028,#2728,.T.);
#6644=EDGE_CURVE('',#5057,#5051,#2729,.T.);
#6645=EDGE_CURVE('',#5056,#5057,#1975,.T.);
#6646=EDGE_CURVE('',#5029,#5054,#2730,.T.);
#6647=EDGE_CURVE('',#5057,#5011,#2731,.T.);
#6648=EDGE_CURVE('',#5058,#5059,#3363,.T.);
#6649=EDGE_CURVE('',#5058,#5060,#3364,.T.);
#6650=EDGE_CURVE('',#5060,#5061,#3365,.T.);
#6651=EDGE_CURVE('',#5059,#5061,#3366,.T.);
#6652=EDGE_CURVE('',#5062,#5058,#3367,.T.);
#6653=EDGE_CURVE('',#5062,#5063,#3368,.T.);
#6654=EDGE_CURVE('',#5063,#5060,#3369,.T.);
#6655=EDGE_CURVE('',#5064,#5062,#3370,.T.);
#6656=EDGE_CURVE('',#5064,#5065,#3371,.T.);
#6657=EDGE_CURVE('',#5065,#5063,#3372,.T.);
#6658=EDGE_CURVE('',#5066,#5064,#3373,.T.);
#6659=EDGE_CURVE('',#5066,#5067,#3374,.T.);
#6660=EDGE_CURVE('',#5067,#5065,#3375,.T.);
#6661=EDGE_CURVE('',#5068,#5066,#3376,.T.);
#6662=EDGE_CURVE('',#5068,#5069,#3377,.T.);
#6663=EDGE_CURVE('',#5069,#5067,#3378,.T.);
#6664=EDGE_CURVE('',#5059,#5068,#3379,.T.);
#6665=EDGE_CURVE('',#5061,#5069,#3380,.T.);
#6666=EDGE_CURVE('',#5070,#5070,#1976,.T.);
#6667=EDGE_CURVE('',#5070,#5071,#3381,.T.);
#6668=EDGE_CURVE('',#5071,#5071,#1977,.T.);
#6669=EDGE_CURVE('',#5072,#5073,#3382,.T.);
#6670=EDGE_CURVE('',#5072,#5074,#2732,.T.);
#6671=EDGE_CURVE('',#5074,#5075,#1978,.F.);
#6672=EDGE_CURVE('',#5075,#5073,#2733,.T.);
#6673=EDGE_CURVE('',#5076,#5077,#3383,.T.);
#6674=EDGE_CURVE('',#5076,#5072,#2734,.T.);
#6675=EDGE_CURVE('',#5073,#5077,#2735,.T.);
#6676=EDGE_CURVE('',#5078,#5079,#3384,.T.);
#6677=EDGE_CURVE('',#5078,#5076,#2736,.T.);
#6678=EDGE_CURVE('',#5077,#5079,#2737,.T.);
#6679=EDGE_CURVE('',#5080,#5081,#3385,.T.);
#6680=EDGE_CURVE('',#5080,#5078,#2738,.T.);
#6681=EDGE_CURVE('',#5079,#5081,#2739,.T.);
#6682=EDGE_CURVE('',#5082,#5083,#3386,.T.);
#6683=EDGE_CURVE('',#5082,#5080,#2740,.T.);
#6684=EDGE_CURVE('',#5081,#5083,#2741,.T.);
#6685=EDGE_CURVE('',#5084,#5085,#3387,.T.);
#6686=EDGE_CURVE('',#5084,#5082,#2742,.T.);
#6687=EDGE_CURVE('',#5083,#5085,#2743,.T.);
#6688=EDGE_CURVE('',#5086,#5087,#3388,.T.);
#6689=EDGE_CURVE('',#5086,#5084,#2744,.T.);
#6690=EDGE_CURVE('',#5085,#5087,#2745,.T.);
#6691=EDGE_CURVE('',#5088,#5089,#3389,.T.);
#6692=EDGE_CURVE('',#5088,#5086,#2746,.T.);
#6693=EDGE_CURVE('',#5087,#5089,#2747,.T.);
#6694=EDGE_CURVE('',#5090,#5091,#3390,.T.);
#6695=EDGE_CURVE('',#5090,#5088,#2748,.T.);
#6696=EDGE_CURVE('',#5089,#5091,#2749,.T.);
#6697=EDGE_CURVE('',#5092,#5093,#3391,.T.);
#6698=EDGE_CURVE('',#5092,#5090,#2750,.T.);
#6699=EDGE_CURVE('',#5091,#5093,#2751,.T.);
#6700=EDGE_CURVE('',#5094,#5095,#3392,.T.);
#6701=EDGE_CURVE('',#5094,#5092,#2752,.T.);
#6702=EDGE_CURVE('',#5093,#5095,#2753,.T.);
#6703=EDGE_CURVE('',#5096,#5097,#3393,.T.);
#6704=EDGE_CURVE('',#5096,#5094,#2754,.T.);
#6705=EDGE_CURVE('',#5095,#5097,#2755,.T.);
#6706=EDGE_CURVE('',#5098,#5099,#3394,.T.);
#6707=EDGE_CURVE('',#5098,#5096,#2756,.T.);
#6708=EDGE_CURVE('',#5097,#5099,#2757,.T.);
#6709=EDGE_CURVE('',#5100,#5101,#3395,.T.);
#6710=EDGE_CURVE('',#5100,#5098,#2758,.T.);
#6711=EDGE_CURVE('',#5099,#5101,#2759,.T.);
#6712=EDGE_CURVE('',#5102,#5103,#3396,.T.);
#6713=EDGE_CURVE('',#5102,#5100,#2760,.T.);
#6714=EDGE_CURVE('',#5101,#5103,#2761,.T.);
#6715=EDGE_CURVE('',#5104,#5105,#3397,.T.);
#6716=EDGE_CURVE('',#5104,#5102,#2762,.T.);
#6717=EDGE_CURVE('',#5103,#5105,#2763,.T.);
#6718=EDGE_CURVE('',#5106,#5107,#3398,.T.);
#6719=EDGE_CURVE('',#5106,#5104,#2764,.T.);
#6720=EDGE_CURVE('',#5105,#5107,#2765,.T.);
#6721=EDGE_CURVE('',#5108,#5109,#3399,.T.);
#6722=EDGE_CURVE('',#5108,#5106,#2766,.T.);
#6723=EDGE_CURVE('',#5107,#5109,#2767,.T.);
#6724=EDGE_CURVE('',#5110,#5111,#3400,.T.);
#6725=EDGE_CURVE('',#5110,#5112,#2768,.T.);
#6726=EDGE_CURVE('',#5112,#5113,#1979,.T.);
#6727=EDGE_CURVE('',#5111,#5113,#2769,.T.);
#6728=EDGE_CURVE('',#5114,#5115,#3401,.T.);
#6729=EDGE_CURVE('',#5114,#5110,#2770,.T.);
#6730=EDGE_CURVE('',#5115,#5111,#2771,.T.);
#6731=EDGE_CURVE('',#5116,#5117,#3402,.T.);
#6732=EDGE_CURVE('',#5116,#5114,#2772,.T.);
#6733=EDGE_CURVE('',#5117,#5115,#2773,.T.);
#6734=EDGE_CURVE('',#5118,#5119,#3403,.T.);
#6735=EDGE_CURVE('',#5118,#5116,#2774,.T.);
#6736=EDGE_CURVE('',#5119,#5117,#2775,.T.);
#6737=EDGE_CURVE('',#5120,#5121,#3404,.T.);
#6738=EDGE_CURVE('',#5120,#5118,#2776,.T.);
#6739=EDGE_CURVE('',#5121,#5119,#2777,.T.);
#6740=EDGE_CURVE('',#5122,#5123,#3405,.T.);
#6741=EDGE_CURVE('',#5122,#5120,#2778,.T.);
#6742=EDGE_CURVE('',#5123,#5121,#2779,.T.);
#6743=EDGE_CURVE('',#5124,#5125,#3406,.T.);
#6744=EDGE_CURVE('',#5124,#5122,#2780,.T.);
#6745=EDGE_CURVE('',#5125,#5123,#2781,.T.);
#6746=EDGE_CURVE('',#5126,#5127,#3407,.T.);
#6747=EDGE_CURVE('',#5126,#5124,#2782,.T.);
#6748=EDGE_CURVE('',#5127,#5125,#2783,.T.);
#6749=EDGE_CURVE('',#5128,#5129,#3408,.T.);
#6750=EDGE_CURVE('',#5128,#5126,#2784,.T.);
#6751=EDGE_CURVE('',#5129,#5127,#2785,.T.);
#6752=EDGE_CURVE('',#5130,#5131,#3409,.T.);
#6753=EDGE_CURVE('',#5130,#5128,#2786,.T.);
#6754=EDGE_CURVE('',#5131,#5129,#2787,.T.);
#6755=EDGE_CURVE('',#5132,#5133,#3410,.T.);
#6756=EDGE_CURVE('',#5132,#5130,#2788,.T.);
#6757=EDGE_CURVE('',#5133,#5131,#2789,.T.);
#6758=EDGE_CURVE('',#5134,#5135,#3411,.T.);
#6759=EDGE_CURVE('',#5134,#5132,#2790,.T.);
#6760=EDGE_CURVE('',#5135,#5133,#2791,.T.);
#6761=EDGE_CURVE('',#5136,#5137,#3412,.T.);
#6762=EDGE_CURVE('',#5136,#5134,#2792,.T.);
#6763=EDGE_CURVE('',#5137,#5135,#2793,.T.);
#6764=EDGE_CURVE('',#5138,#5139,#3413,.T.);
#6765=EDGE_CURVE('',#5138,#5136,#2794,.T.);
#6766=EDGE_CURVE('',#5139,#5137,#2795,.T.);
#6767=EDGE_CURVE('',#5140,#5141,#3414,.T.);
#6768=EDGE_CURVE('',#5140,#5138,#2796,.T.);
#6769=EDGE_CURVE('',#5141,#5139,#2797,.T.);
#6770=EDGE_CURVE('',#5142,#5143,#3415,.T.);
#6771=EDGE_CURVE('',#5142,#5140,#2798,.T.);
#6772=EDGE_CURVE('',#5143,#5141,#2799,.T.);
#6773=EDGE_CURVE('',#5144,#5145,#3416,.T.);
#6774=EDGE_CURVE('',#5144,#5142,#2800,.T.);
#6775=EDGE_CURVE('',#5145,#5143,#2801,.T.);
#6776=EDGE_CURVE('',#5146,#5147,#3417,.T.);
#6777=EDGE_CURVE('',#5146,#5144,#2802,.T.);
#6778=EDGE_CURVE('',#5147,#5145,#2803,.T.);
#6779=EDGE_CURVE('',#5113,#5148,#2804,.T.);
#6780=EDGE_CURVE('',#5149,#5112,#2805,.T.);
#6781=EDGE_CURVE('',#5150,#5149,#1980,.T.);
#6782=EDGE_CURVE('',#5148,#5150,#2806,.T.);
#6783=EDGE_CURVE('',#5148,#5151,#3418,.T.);
#6784=EDGE_CURVE('',#5151,#5151,#1981,.T.);
#6785=EDGE_CURVE('',#5152,#5146,#2807,.T.);
#6786=EDGE_CURVE('',#5074,#5152,#2808,.T.);
#6787=EDGE_CURVE('',#5149,#5108,#2809,.T.);
#6788=EDGE_CURVE('',#5153,#5147,#2810,.T.);
#6789=EDGE_CURVE('',#5152,#5153,#1982,.T.);
#6790=EDGE_CURVE('',#5109,#5150,#2811,.T.);
#6791=EDGE_CURVE('',#5153,#5075,#2812,.T.);
#6792=EDGE_CURVE('',#5154,#5155,#3419,.T.);
#6793=EDGE_CURVE('',#5154,#5156,#3420,.T.);
#6794=EDGE_CURVE('',#5156,#5157,#3421,.T.);
#6795=EDGE_CURVE('',#5155,#5157,#3422,.T.);
#6796=EDGE_CURVE('',#5158,#5154,#3423,.T.);
#6797=EDGE_CURVE('',#5158,#5159,#3424,.T.);
#6798=EDGE_CURVE('',#5159,#5156,#3425,.T.);
#6799=EDGE_CURVE('',#5160,#5158,#3426,.T.);
#6800=EDGE_CURVE('',#5160,#5161,#3427,.T.);
#6801=EDGE_CURVE('',#5161,#5159,#3428,.T.);
#6802=EDGE_CURVE('',#5162,#5160,#3429,.T.);
#6803=EDGE_CURVE('',#5162,#5163,#3430,.T.);
#6804=EDGE_CURVE('',#5163,#5161,#3431,.T.);
#6805=EDGE_CURVE('',#5164,#5162,#3432,.T.);
#6806=EDGE_CURVE('',#5164,#5165,#3433,.T.);
#6807=EDGE_CURVE('',#5165,#5163,#3434,.T.);
#6808=EDGE_CURVE('',#5155,#5164,#3435,.T.);
#6809=EDGE_CURVE('',#5157,#5165,#3436,.T.);
#6810=EDGE_CURVE('',#5166,#5166,#1983,.T.);
#6811=EDGE_CURVE('',#5166,#5167,#3437,.T.);
#6812=EDGE_CURVE('',#5167,#5167,#1984,.T.);
#6813=EDGE_CURVE('',#5168,#5169,#3438,.T.);
#6814=EDGE_CURVE('',#5168,#5170,#2813,.T.);
#6815=EDGE_CURVE('',#5170,#5171,#1985,.F.);
#6816=EDGE_CURVE('',#5171,#5169,#2814,.T.);
#6817=EDGE_CURVE('',#5172,#5173,#3439,.T.);
#6818=EDGE_CURVE('',#5172,#5168,#2815,.T.);
#6819=EDGE_CURVE('',#5169,#5173,#2816,.T.);
#6820=EDGE_CURVE('',#5174,#5175,#3440,.T.);
#6821=EDGE_CURVE('',#5174,#5176,#2817,.T.);
#6822=EDGE_CURVE('',#5176,#5177,#1986,.T.);
#6823=EDGE_CURVE('',#5175,#5177,#2818,.T.);
#6824=EDGE_CURVE('',#5178,#5179,#3441,.T.);
#6825=EDGE_CURVE('',#5178,#5174,#2819,.T.);
#6826=EDGE_CURVE('',#5179,#5175,#2820,.T.);
#6827=EDGE_CURVE('',#5177,#5180,#2821,.T.);
#6828=EDGE_CURVE('',#5181,#5176,#2822,.T.);
#6829=EDGE_CURVE('',#5182,#5181,#1987,.T.);
#6830=EDGE_CURVE('',#5180,#5182,#2823,.T.);
#6831=EDGE_CURVE('',#5180,#5183,#3442,.T.);
#6832=EDGE_CURVE('',#5183,#5183,#1988,.T.);
#6833=EDGE_CURVE('',#5184,#5178,#2824,.T.);
#6834=EDGE_CURVE('',#5170,#5184,#2825,.T.);
#6835=EDGE_CURVE('',#5181,#5172,#2826,.T.);
#6836=EDGE_CURVE('',#5185,#5179,#2827,.T.);
#6837=EDGE_CURVE('',#5184,#5185,#1989,.T.);
#6838=EDGE_CURVE('',#5173,#5182,#2828,.T.);
#6839=EDGE_CURVE('',#5185,#5171,#2829,.T.);
#6840=EDGE_CURVE('',#5186,#5187,#3443,.T.);
#6841=EDGE_CURVE('',#5186,#5188,#3444,.T.);
#6842=EDGE_CURVE('',#5188,#5189,#3445,.T.);
#6843=EDGE_CURVE('',#5187,#5189,#3446,.T.);
#6844=EDGE_CURVE('',#5190,#5186,#3447,.T.);
#6845=EDGE_CURVE('',#5190,#5191,#3448,.T.);
#6846=EDGE_CURVE('',#5191,#5188,#3449,.T.);
#6847=EDGE_CURVE('',#5192,#5190,#3450,.T.);
#6848=EDGE_CURVE('',#5192,#5193,#3451,.T.);
#6849=EDGE_CURVE('',#5193,#5191,#3452,.T.);
#6850=EDGE_CURVE('',#5194,#5192,#3453,.T.);
#6851=EDGE_CURVE('',#5194,#5195,#3454,.T.);
#6852=EDGE_CURVE('',#5195,#5193,#3455,.T.);
#6853=EDGE_CURVE('',#5196,#5194,#3456,.T.);
#6854=EDGE_CURVE('',#5196,#5197,#3457,.T.);
#6855=EDGE_CURVE('',#5197,#5195,#3458,.T.);
#6856=EDGE_CURVE('',#5187,#5196,#3459,.T.);
#6857=EDGE_CURVE('',#5189,#5197,#3460,.T.);
#6858=EDGE_CURVE('',#5198,#5198,#1990,.T.);
#6859=EDGE_CURVE('',#5198,#5199,#3461,.T.);
#6860=EDGE_CURVE('',#5199,#5199,#1991,.T.);
#6861=ORIENTED_EDGE('',*,*,#5200,.T.);
#6862=ORIENTED_EDGE('',*,*,#5201,.T.);
#6863=ORIENTED_EDGE('',*,*,#5202,.T.);
#6864=ORIENTED_EDGE('',*,*,#5203,.T.);
#6865=ORIENTED_EDGE('',*,*,#5204,.T.);
#6866=ORIENTED_EDGE('',*,*,#5205,.T.);
#6867=ORIENTED_EDGE('',*,*,#5204,.F.);
#6868=ORIENTED_EDGE('',*,*,#5206,.T.);
#6869=ORIENTED_EDGE('',*,*,#5207,.T.);
#6870=ORIENTED_EDGE('',*,*,#5208,.T.);
#6871=ORIENTED_EDGE('',*,*,#5200,.F.);
#6872=ORIENTED_EDGE('',*,*,#5209,.T.);
#6873=ORIENTED_EDGE('',*,*,#5210,.T.);
#6874=ORIENTED_EDGE('',*,*,#5211,.T.);
#6875=ORIENTED_EDGE('',*,*,#5207,.F.);
#6876=ORIENTED_EDGE('',*,*,#5212,.T.);
#6877=ORIENTED_EDGE('',*,*,#5213,.T.);
#6878=ORIENTED_EDGE('',*,*,#5214,.T.);
#6879=ORIENTED_EDGE('',*,*,#5210,.F.);
#6880=ORIENTED_EDGE('',*,*,#5215,.T.);
#6881=ORIENTED_EDGE('',*,*,#5216,.T.);
#6882=ORIENTED_EDGE('',*,*,#5217,.T.);
#6883=ORIENTED_EDGE('',*,*,#5213,.F.);
#6884=ORIENTED_EDGE('',*,*,#5218,.T.);
#6885=ORIENTED_EDGE('',*,*,#5219,.T.);
#6886=ORIENTED_EDGE('',*,*,#5220,.T.);
#6887=ORIENTED_EDGE('',*,*,#5216,.F.);
#6888=ORIENTED_EDGE('',*,*,#5221,.T.);
#6889=ORIENTED_EDGE('',*,*,#5222,.T.);
#6890=ORIENTED_EDGE('',*,*,#5223,.T.);
#6891=ORIENTED_EDGE('',*,*,#5219,.F.);
#6892=ORIENTED_EDGE('',*,*,#5224,.T.);
#6893=ORIENTED_EDGE('',*,*,#5225,.T.);
#6894=ORIENTED_EDGE('',*,*,#5226,.T.);
#6895=ORIENTED_EDGE('',*,*,#5222,.F.);
#6896=ORIENTED_EDGE('',*,*,#5227,.T.);
#6897=ORIENTED_EDGE('',*,*,#5228,.T.);
#6898=ORIENTED_EDGE('',*,*,#5229,.T.);
#6899=ORIENTED_EDGE('',*,*,#5225,.F.);
#6900=ORIENTED_EDGE('',*,*,#5230,.T.);
#6901=ORIENTED_EDGE('',*,*,#5231,.T.);
#6902=ORIENTED_EDGE('',*,*,#5232,.T.);
#6903=ORIENTED_EDGE('',*,*,#5228,.F.);
#6904=ORIENTED_EDGE('',*,*,#5233,.T.);
#6905=ORIENTED_EDGE('',*,*,#5234,.T.);
#6906=ORIENTED_EDGE('',*,*,#5235,.T.);
#6907=ORIENTED_EDGE('',*,*,#5231,.F.);
#6908=ORIENTED_EDGE('',*,*,#5236,.T.);
#6909=ORIENTED_EDGE('',*,*,#5237,.F.);
#6910=ORIENTED_EDGE('',*,*,#5238,.T.);
#6911=ORIENTED_EDGE('',*,*,#5239,.F.);
#6912=ORIENTED_EDGE('',*,*,#5240,.T.);
#6913=ORIENTED_EDGE('',*,*,#5241,.T.);
#6914=ORIENTED_EDGE('',*,*,#5242,.T.);
#6915=ORIENTED_EDGE('',*,*,#5243,.F.);
#6916=ORIENTED_EDGE('',*,*,#5244,.F.);
#6917=ORIENTED_EDGE('',*,*,#5245,.T.);
#6918=ORIENTED_EDGE('',*,*,#5246,.T.);
#6919=ORIENTED_EDGE('',*,*,#5241,.F.);
#6920=ORIENTED_EDGE('',*,*,#5247,.F.);
#6921=ORIENTED_EDGE('',*,*,#5248,.T.);
#6922=ORIENTED_EDGE('',*,*,#5249,.T.);
#6923=ORIENTED_EDGE('',*,*,#5245,.F.);
#6924=ORIENTED_EDGE('',*,*,#5250,.F.);
#6925=ORIENTED_EDGE('',*,*,#5251,.T.);
#6926=ORIENTED_EDGE('',*,*,#5252,.T.);
#6927=ORIENTED_EDGE('',*,*,#5248,.F.);
#6928=ORIENTED_EDGE('',*,*,#5253,.F.);
#6929=ORIENTED_EDGE('',*,*,#5254,.T.);
#6930=ORIENTED_EDGE('',*,*,#5255,.T.);
#6931=ORIENTED_EDGE('',*,*,#5251,.F.);
#6932=ORIENTED_EDGE('',*,*,#5256,.F.);
#6933=ORIENTED_EDGE('',*,*,#5257,.T.);
#6934=ORIENTED_EDGE('',*,*,#5258,.T.);
#6935=ORIENTED_EDGE('',*,*,#5254,.F.);
#6936=ORIENTED_EDGE('',*,*,#5259,.F.);
#6937=ORIENTED_EDGE('',*,*,#5260,.T.);
#6938=ORIENTED_EDGE('',*,*,#5261,.T.);
#6939=ORIENTED_EDGE('',*,*,#5257,.F.);
#6940=ORIENTED_EDGE('',*,*,#5262,.F.);
#6941=ORIENTED_EDGE('',*,*,#5263,.T.);
#6942=ORIENTED_EDGE('',*,*,#5264,.T.);
#6943=ORIENTED_EDGE('',*,*,#5260,.F.);
#6944=ORIENTED_EDGE('',*,*,#5265,.F.);
#6945=ORIENTED_EDGE('',*,*,#5266,.T.);
#6946=ORIENTED_EDGE('',*,*,#5267,.T.);
#6947=ORIENTED_EDGE('',*,*,#5263,.F.);
#6948=ORIENTED_EDGE('',*,*,#5268,.F.);
#6949=ORIENTED_EDGE('',*,*,#5269,.T.);
#6950=ORIENTED_EDGE('',*,*,#5270,.T.);
#6951=ORIENTED_EDGE('',*,*,#5266,.F.);
#6952=ORIENTED_EDGE('',*,*,#5271,.F.);
#6953=ORIENTED_EDGE('',*,*,#5272,.T.);
#6954=ORIENTED_EDGE('',*,*,#5273,.T.);
#6955=ORIENTED_EDGE('',*,*,#5269,.F.);
#6956=ORIENTED_EDGE('',*,*,#5274,.F.);
#6957=ORIENTED_EDGE('',*,*,#5275,.T.);
#6958=ORIENTED_EDGE('',*,*,#5276,.T.);
#6959=ORIENTED_EDGE('',*,*,#5272,.F.);
#6960=ORIENTED_EDGE('',*,*,#5277,.F.);
#6961=ORIENTED_EDGE('',*,*,#5278,.F.);
#6962=ORIENTED_EDGE('',*,*,#5279,.F.);
#6963=ORIENTED_EDGE('',*,*,#5280,.F.);
#6964=ORIENTED_EDGE('',*,*,#5281,.T.);
#6965=ORIENTED_EDGE('',*,*,#5282,.T.);
#6966=ORIENTED_EDGE('',*,*,#5283,.T.);
#6967=ORIENTED_EDGE('',*,*,#5284,.T.);
#6968=ORIENTED_EDGE('',*,*,#5285,.T.);
#6969=ORIENTED_EDGE('',*,*,#5286,.T.);
#6970=ORIENTED_EDGE('',*,*,#5287,.T.);
#6971=ORIENTED_EDGE('',*,*,#5286,.F.);
#6972=ORIENTED_EDGE('',*,*,#5288,.T.);
#6973=ORIENTED_EDGE('',*,*,#5289,.T.);
#6974=ORIENTED_EDGE('',*,*,#5290,.T.);
#6975=ORIENTED_EDGE('',*,*,#5282,.F.);
#6976=ORIENTED_EDGE('',*,*,#5291,.T.);
#6977=ORIENTED_EDGE('',*,*,#5292,.T.);
#6978=ORIENTED_EDGE('',*,*,#5293,.T.);
#6979=ORIENTED_EDGE('',*,*,#5289,.F.);
#6980=ORIENTED_EDGE('',*,*,#5294,.T.);
#6981=ORIENTED_EDGE('',*,*,#5295,.T.);
#6982=ORIENTED_EDGE('',*,*,#5296,.T.);
#6983=ORIENTED_EDGE('',*,*,#5292,.F.);
#6984=ORIENTED_EDGE('',*,*,#5297,.T.);
#6985=ORIENTED_EDGE('',*,*,#5298,.T.);
#6986=ORIENTED_EDGE('',*,*,#5299,.T.);
#6987=ORIENTED_EDGE('',*,*,#5295,.F.);
#6988=ORIENTED_EDGE('',*,*,#5300,.T.);
#6989=ORIENTED_EDGE('',*,*,#5301,.T.);
#6990=ORIENTED_EDGE('',*,*,#5302,.T.);
#6991=ORIENTED_EDGE('',*,*,#5298,.F.);
#6992=ORIENTED_EDGE('',*,*,#5303,.T.);
#6993=ORIENTED_EDGE('',*,*,#5304,.T.);
#6994=ORIENTED_EDGE('',*,*,#5305,.T.);
#6995=ORIENTED_EDGE('',*,*,#5301,.F.);
#6996=ORIENTED_EDGE('',*,*,#5306,.T.);
#6997=ORIENTED_EDGE('',*,*,#5307,.T.);
#6998=ORIENTED_EDGE('',*,*,#5308,.T.);
#6999=ORIENTED_EDGE('',*,*,#5304,.F.);
#7000=ORIENTED_EDGE('',*,*,#5309,.T.);
#7001=ORIENTED_EDGE('',*,*,#5310,.T.);
#7002=ORIENTED_EDGE('',*,*,#5311,.T.);
#7003=ORIENTED_EDGE('',*,*,#5307,.F.);
#7004=ORIENTED_EDGE('',*,*,#5312,.T.);
#7005=ORIENTED_EDGE('',*,*,#5313,.T.);
#7006=ORIENTED_EDGE('',*,*,#5314,.T.);
#7007=ORIENTED_EDGE('',*,*,#5310,.F.);
#7008=ORIENTED_EDGE('',*,*,#5315,.T.);
#7009=ORIENTED_EDGE('',*,*,#5316,.T.);
#7010=ORIENTED_EDGE('',*,*,#5317,.T.);
#7011=ORIENTED_EDGE('',*,*,#5313,.F.);
#7012=ORIENTED_EDGE('',*,*,#5318,.T.);
#7013=ORIENTED_EDGE('',*,*,#5319,.F.);
#7014=ORIENTED_EDGE('',*,*,#5320,.T.);
#7015=ORIENTED_EDGE('',*,*,#5321,.F.);
#7016=ORIENTED_EDGE('',*,*,#5322,.T.);
#7017=ORIENTED_EDGE('',*,*,#5323,.T.);
#7018=ORIENTED_EDGE('',*,*,#5324,.T.);
#7019=ORIENTED_EDGE('',*,*,#5325,.F.);
#7020=ORIENTED_EDGE('',*,*,#5326,.F.);
#7021=ORIENTED_EDGE('',*,*,#5327,.T.);
#7022=ORIENTED_EDGE('',*,*,#5328,.T.);
#7023=ORIENTED_EDGE('',*,*,#5323,.F.);
#7024=ORIENTED_EDGE('',*,*,#5329,.F.);
#7025=ORIENTED_EDGE('',*,*,#5330,.T.);
#7026=ORIENTED_EDGE('',*,*,#5331,.T.);
#7027=ORIENTED_EDGE('',*,*,#5327,.F.);
#7028=ORIENTED_EDGE('',*,*,#5332,.F.);
#7029=ORIENTED_EDGE('',*,*,#5333,.T.);
#7030=ORIENTED_EDGE('',*,*,#5334,.T.);
#7031=ORIENTED_EDGE('',*,*,#5330,.F.);
#7032=ORIENTED_EDGE('',*,*,#5335,.F.);
#7033=ORIENTED_EDGE('',*,*,#5336,.T.);
#7034=ORIENTED_EDGE('',*,*,#5337,.T.);
#7035=ORIENTED_EDGE('',*,*,#5333,.F.);
#7036=ORIENTED_EDGE('',*,*,#5338,.F.);
#7037=ORIENTED_EDGE('',*,*,#5339,.T.);
#7038=ORIENTED_EDGE('',*,*,#5340,.T.);
#7039=ORIENTED_EDGE('',*,*,#5336,.F.);
#7040=ORIENTED_EDGE('',*,*,#5341,.F.);
#7041=ORIENTED_EDGE('',*,*,#5342,.T.);
#7042=ORIENTED_EDGE('',*,*,#5343,.T.);
#7043=ORIENTED_EDGE('',*,*,#5339,.F.);
#7044=ORIENTED_EDGE('',*,*,#5344,.F.);
#7045=ORIENTED_EDGE('',*,*,#5345,.T.);
#7046=ORIENTED_EDGE('',*,*,#5346,.T.);
#7047=ORIENTED_EDGE('',*,*,#5342,.F.);
#7048=ORIENTED_EDGE('',*,*,#5347,.F.);
#7049=ORIENTED_EDGE('',*,*,#5348,.T.);
#7050=ORIENTED_EDGE('',*,*,#5349,.T.);
#7051=ORIENTED_EDGE('',*,*,#5345,.F.);
#7052=ORIENTED_EDGE('',*,*,#5350,.F.);
#7053=ORIENTED_EDGE('',*,*,#5351,.T.);
#7054=ORIENTED_EDGE('',*,*,#5352,.T.);
#7055=ORIENTED_EDGE('',*,*,#5348,.F.);
#7056=ORIENTED_EDGE('',*,*,#5353,.F.);
#7057=ORIENTED_EDGE('',*,*,#5354,.T.);
#7058=ORIENTED_EDGE('',*,*,#5355,.T.);
#7059=ORIENTED_EDGE('',*,*,#5351,.F.);
#7060=ORIENTED_EDGE('',*,*,#5356,.F.);
#7061=ORIENTED_EDGE('',*,*,#5357,.T.);
#7062=ORIENTED_EDGE('',*,*,#5358,.T.);
#7063=ORIENTED_EDGE('',*,*,#5354,.F.);
#7064=ORIENTED_EDGE('',*,*,#5359,.F.);
#7065=ORIENTED_EDGE('',*,*,#5360,.F.);
#7066=ORIENTED_EDGE('',*,*,#5361,.F.);
#7067=ORIENTED_EDGE('',*,*,#5362,.F.);
#7068=ORIENTED_EDGE('',*,*,#5363,.T.);
#7069=ORIENTED_EDGE('',*,*,#5364,.T.);
#7070=ORIENTED_EDGE('',*,*,#5365,.T.);
#7071=ORIENTED_EDGE('',*,*,#5366,.T.);
#7072=ORIENTED_EDGE('',*,*,#5367,.T.);
#7073=ORIENTED_EDGE('',*,*,#5368,.T.);
#7074=ORIENTED_EDGE('',*,*,#5369,.T.);
#7075=ORIENTED_EDGE('',*,*,#5368,.F.);
#7076=ORIENTED_EDGE('',*,*,#5370,.T.);
#7077=ORIENTED_EDGE('',*,*,#5371,.T.);
#7078=ORIENTED_EDGE('',*,*,#5372,.T.);
#7079=ORIENTED_EDGE('',*,*,#5364,.F.);
#7080=ORIENTED_EDGE('',*,*,#5373,.T.);
#7081=ORIENTED_EDGE('',*,*,#5374,.T.);
#7082=ORIENTED_EDGE('',*,*,#5375,.T.);
#7083=ORIENTED_EDGE('',*,*,#5371,.F.);
#7084=ORIENTED_EDGE('',*,*,#5376,.T.);
#7085=ORIENTED_EDGE('',*,*,#5377,.T.);
#7086=ORIENTED_EDGE('',*,*,#5378,.T.);
#7087=ORIENTED_EDGE('',*,*,#5374,.F.);
#7088=ORIENTED_EDGE('',*,*,#5379,.T.);
#7089=ORIENTED_EDGE('',*,*,#5380,.T.);
#7090=ORIENTED_EDGE('',*,*,#5381,.T.);
#7091=ORIENTED_EDGE('',*,*,#5377,.F.);
#7092=ORIENTED_EDGE('',*,*,#5382,.T.);
#7093=ORIENTED_EDGE('',*,*,#5383,.T.);
#7094=ORIENTED_EDGE('',*,*,#5384,.T.);
#7095=ORIENTED_EDGE('',*,*,#5380,.F.);
#7096=ORIENTED_EDGE('',*,*,#5385,.T.);
#7097=ORIENTED_EDGE('',*,*,#5386,.T.);
#7098=ORIENTED_EDGE('',*,*,#5387,.T.);
#7099=ORIENTED_EDGE('',*,*,#5383,.F.);
#7100=ORIENTED_EDGE('',*,*,#5388,.T.);
#7101=ORIENTED_EDGE('',*,*,#5389,.T.);
#7102=ORIENTED_EDGE('',*,*,#5390,.T.);
#7103=ORIENTED_EDGE('',*,*,#5386,.F.);
#7104=ORIENTED_EDGE('',*,*,#5391,.T.);
#7105=ORIENTED_EDGE('',*,*,#5392,.T.);
#7106=ORIENTED_EDGE('',*,*,#5393,.T.);
#7107=ORIENTED_EDGE('',*,*,#5389,.F.);
#7108=ORIENTED_EDGE('',*,*,#5394,.T.);
#7109=ORIENTED_EDGE('',*,*,#5395,.T.);
#7110=ORIENTED_EDGE('',*,*,#5396,.T.);
#7111=ORIENTED_EDGE('',*,*,#5392,.F.);
#7112=ORIENTED_EDGE('',*,*,#5397,.T.);
#7113=ORIENTED_EDGE('',*,*,#5398,.T.);
#7114=ORIENTED_EDGE('',*,*,#5399,.T.);
#7115=ORIENTED_EDGE('',*,*,#5395,.F.);
#7116=ORIENTED_EDGE('',*,*,#5400,.T.);
#7117=ORIENTED_EDGE('',*,*,#5401,.F.);
#7118=ORIENTED_EDGE('',*,*,#5402,.T.);
#7119=ORIENTED_EDGE('',*,*,#5403,.F.);
#7120=ORIENTED_EDGE('',*,*,#5404,.T.);
#7121=ORIENTED_EDGE('',*,*,#5405,.T.);
#7122=ORIENTED_EDGE('',*,*,#5406,.T.);
#7123=ORIENTED_EDGE('',*,*,#5407,.F.);
#7124=ORIENTED_EDGE('',*,*,#5408,.F.);
#7125=ORIENTED_EDGE('',*,*,#5409,.T.);
#7126=ORIENTED_EDGE('',*,*,#5410,.T.);
#7127=ORIENTED_EDGE('',*,*,#5405,.F.);
#7128=ORIENTED_EDGE('',*,*,#5411,.F.);
#7129=ORIENTED_EDGE('',*,*,#5412,.T.);
#7130=ORIENTED_EDGE('',*,*,#5413,.T.);
#7131=ORIENTED_EDGE('',*,*,#5409,.F.);
#7132=ORIENTED_EDGE('',*,*,#5414,.F.);
#7133=ORIENTED_EDGE('',*,*,#5415,.T.);
#7134=ORIENTED_EDGE('',*,*,#5416,.T.);
#7135=ORIENTED_EDGE('',*,*,#5412,.F.);
#7136=ORIENTED_EDGE('',*,*,#5417,.F.);
#7137=ORIENTED_EDGE('',*,*,#5418,.T.);
#7138=ORIENTED_EDGE('',*,*,#5419,.T.);
#7139=ORIENTED_EDGE('',*,*,#5415,.F.);
#7140=ORIENTED_EDGE('',*,*,#5420,.F.);
#7141=ORIENTED_EDGE('',*,*,#5421,.T.);
#7142=ORIENTED_EDGE('',*,*,#5422,.T.);
#7143=ORIENTED_EDGE('',*,*,#5418,.F.);
#7144=ORIENTED_EDGE('',*,*,#5423,.F.);
#7145=ORIENTED_EDGE('',*,*,#5424,.T.);
#7146=ORIENTED_EDGE('',*,*,#5425,.T.);
#7147=ORIENTED_EDGE('',*,*,#5421,.F.);
#7148=ORIENTED_EDGE('',*,*,#5426,.F.);
#7149=ORIENTED_EDGE('',*,*,#5427,.T.);
#7150=ORIENTED_EDGE('',*,*,#5428,.T.);
#7151=ORIENTED_EDGE('',*,*,#5424,.F.);
#7152=ORIENTED_EDGE('',*,*,#5429,.F.);
#7153=ORIENTED_EDGE('',*,*,#5430,.T.);
#7154=ORIENTED_EDGE('',*,*,#5431,.T.);
#7155=ORIENTED_EDGE('',*,*,#5427,.F.);
#7156=ORIENTED_EDGE('',*,*,#5432,.F.);
#7157=ORIENTED_EDGE('',*,*,#5433,.T.);
#7158=ORIENTED_EDGE('',*,*,#5434,.T.);
#7159=ORIENTED_EDGE('',*,*,#5430,.F.);
#7160=ORIENTED_EDGE('',*,*,#5435,.F.);
#7161=ORIENTED_EDGE('',*,*,#5436,.T.);
#7162=ORIENTED_EDGE('',*,*,#5437,.T.);
#7163=ORIENTED_EDGE('',*,*,#5433,.F.);
#7164=ORIENTED_EDGE('',*,*,#5438,.F.);
#7165=ORIENTED_EDGE('',*,*,#5439,.T.);
#7166=ORIENTED_EDGE('',*,*,#5440,.T.);
#7167=ORIENTED_EDGE('',*,*,#5436,.F.);
#7168=ORIENTED_EDGE('',*,*,#5441,.F.);
#7169=ORIENTED_EDGE('',*,*,#5442,.F.);
#7170=ORIENTED_EDGE('',*,*,#5443,.F.);
#7171=ORIENTED_EDGE('',*,*,#5444,.F.);
#7172=ORIENTED_EDGE('',*,*,#5445,.T.);
#7173=ORIENTED_EDGE('',*,*,#5446,.T.);
#7174=ORIENTED_EDGE('',*,*,#5447,.T.);
#7175=ORIENTED_EDGE('',*,*,#5448,.T.);
#7176=ORIENTED_EDGE('',*,*,#5449,.T.);
#7177=ORIENTED_EDGE('',*,*,#5450,.T.);
#7178=ORIENTED_EDGE('',*,*,#5451,.T.);
#7179=ORIENTED_EDGE('',*,*,#5450,.F.);
#7180=ORIENTED_EDGE('',*,*,#5452,.T.);
#7181=ORIENTED_EDGE('',*,*,#5453,.T.);
#7182=ORIENTED_EDGE('',*,*,#5454,.T.);
#7183=ORIENTED_EDGE('',*,*,#5446,.F.);
#7184=ORIENTED_EDGE('',*,*,#5455,.T.);
#7185=ORIENTED_EDGE('',*,*,#5456,.T.);
#7186=ORIENTED_EDGE('',*,*,#5457,.T.);
#7187=ORIENTED_EDGE('',*,*,#5453,.F.);
#7188=ORIENTED_EDGE('',*,*,#5458,.T.);
#7189=ORIENTED_EDGE('',*,*,#5459,.T.);
#7190=ORIENTED_EDGE('',*,*,#5460,.T.);
#7191=ORIENTED_EDGE('',*,*,#5456,.F.);
#7192=ORIENTED_EDGE('',*,*,#5461,.T.);
#7193=ORIENTED_EDGE('',*,*,#5462,.T.);
#7194=ORIENTED_EDGE('',*,*,#5463,.T.);
#7195=ORIENTED_EDGE('',*,*,#5459,.F.);
#7196=ORIENTED_EDGE('',*,*,#5464,.T.);
#7197=ORIENTED_EDGE('',*,*,#5465,.T.);
#7198=ORIENTED_EDGE('',*,*,#5466,.T.);
#7199=ORIENTED_EDGE('',*,*,#5462,.F.);
#7200=ORIENTED_EDGE('',*,*,#5467,.T.);
#7201=ORIENTED_EDGE('',*,*,#5468,.T.);
#7202=ORIENTED_EDGE('',*,*,#5469,.T.);
#7203=ORIENTED_EDGE('',*,*,#5465,.F.);
#7204=ORIENTED_EDGE('',*,*,#5470,.T.);
#7205=ORIENTED_EDGE('',*,*,#5471,.T.);
#7206=ORIENTED_EDGE('',*,*,#5472,.T.);
#7207=ORIENTED_EDGE('',*,*,#5468,.F.);
#7208=ORIENTED_EDGE('',*,*,#5473,.T.);
#7209=ORIENTED_EDGE('',*,*,#5474,.T.);
#7210=ORIENTED_EDGE('',*,*,#5475,.T.);
#7211=ORIENTED_EDGE('',*,*,#5471,.F.);
#7212=ORIENTED_EDGE('',*,*,#5476,.T.);
#7213=ORIENTED_EDGE('',*,*,#5477,.T.);
#7214=ORIENTED_EDGE('',*,*,#5478,.T.);
#7215=ORIENTED_EDGE('',*,*,#5474,.F.);
#7216=ORIENTED_EDGE('',*,*,#5479,.T.);
#7217=ORIENTED_EDGE('',*,*,#5480,.T.);
#7218=ORIENTED_EDGE('',*,*,#5481,.T.);
#7219=ORIENTED_EDGE('',*,*,#5477,.F.);
#7220=ORIENTED_EDGE('',*,*,#5482,.T.);
#7221=ORIENTED_EDGE('',*,*,#5483,.F.);
#7222=ORIENTED_EDGE('',*,*,#5484,.T.);
#7223=ORIENTED_EDGE('',*,*,#5485,.F.);
#7224=ORIENTED_EDGE('',*,*,#5486,.T.);
#7225=ORIENTED_EDGE('',*,*,#5487,.T.);
#7226=ORIENTED_EDGE('',*,*,#5488,.T.);
#7227=ORIENTED_EDGE('',*,*,#5489,.F.);
#7228=ORIENTED_EDGE('',*,*,#5490,.F.);
#7229=ORIENTED_EDGE('',*,*,#5491,.T.);
#7230=ORIENTED_EDGE('',*,*,#5492,.T.);
#7231=ORIENTED_EDGE('',*,*,#5487,.F.);
#7232=ORIENTED_EDGE('',*,*,#5493,.F.);
#7233=ORIENTED_EDGE('',*,*,#5494,.T.);
#7234=ORIENTED_EDGE('',*,*,#5495,.T.);
#7235=ORIENTED_EDGE('',*,*,#5491,.F.);
#7236=ORIENTED_EDGE('',*,*,#5496,.F.);
#7237=ORIENTED_EDGE('',*,*,#5497,.T.);
#7238=ORIENTED_EDGE('',*,*,#5498,.T.);
#7239=ORIENTED_EDGE('',*,*,#5494,.F.);
#7240=ORIENTED_EDGE('',*,*,#5499,.F.);
#7241=ORIENTED_EDGE('',*,*,#5500,.T.);
#7242=ORIENTED_EDGE('',*,*,#5501,.T.);
#7243=ORIENTED_EDGE('',*,*,#5497,.F.);
#7244=ORIENTED_EDGE('',*,*,#5502,.F.);
#7245=ORIENTED_EDGE('',*,*,#5503,.T.);
#7246=ORIENTED_EDGE('',*,*,#5504,.T.);
#7247=ORIENTED_EDGE('',*,*,#5500,.F.);
#7248=ORIENTED_EDGE('',*,*,#5505,.F.);
#7249=ORIENTED_EDGE('',*,*,#5506,.T.);
#7250=ORIENTED_EDGE('',*,*,#5507,.T.);
#7251=ORIENTED_EDGE('',*,*,#5503,.F.);
#7252=ORIENTED_EDGE('',*,*,#5508,.F.);
#7253=ORIENTED_EDGE('',*,*,#5509,.T.);
#7254=ORIENTED_EDGE('',*,*,#5510,.T.);
#7255=ORIENTED_EDGE('',*,*,#5506,.F.);
#7256=ORIENTED_EDGE('',*,*,#5511,.F.);
#7257=ORIENTED_EDGE('',*,*,#5512,.T.);
#7258=ORIENTED_EDGE('',*,*,#5513,.T.);
#7259=ORIENTED_EDGE('',*,*,#5509,.F.);
#7260=ORIENTED_EDGE('',*,*,#5514,.F.);
#7261=ORIENTED_EDGE('',*,*,#5515,.T.);
#7262=ORIENTED_EDGE('',*,*,#5516,.T.);
#7263=ORIENTED_EDGE('',*,*,#5512,.F.);
#7264=ORIENTED_EDGE('',*,*,#5517,.F.);
#7265=ORIENTED_EDGE('',*,*,#5518,.T.);
#7266=ORIENTED_EDGE('',*,*,#5519,.T.);
#7267=ORIENTED_EDGE('',*,*,#5515,.F.);
#7268=ORIENTED_EDGE('',*,*,#5520,.F.);
#7269=ORIENTED_EDGE('',*,*,#5521,.T.);
#7270=ORIENTED_EDGE('',*,*,#5522,.T.);
#7271=ORIENTED_EDGE('',*,*,#5518,.F.);
#7272=ORIENTED_EDGE('',*,*,#5523,.F.);
#7273=ORIENTED_EDGE('',*,*,#5524,.F.);
#7274=ORIENTED_EDGE('',*,*,#5525,.F.);
#7275=ORIENTED_EDGE('',*,*,#5526,.F.);
#7276=ORIENTED_EDGE('',*,*,#5527,.T.);
#7277=ORIENTED_EDGE('',*,*,#5528,.F.);
#7278=ORIENTED_EDGE('',*,*,#5529,.T.);
#7279=ORIENTED_EDGE('',*,*,#5530,.F.);
#7280=ORIENTED_EDGE('',*,*,#5529,.F.);
#7281=ORIENTED_EDGE('',*,*,#5531,.F.);
#7282=ORIENTED_EDGE('',*,*,#5532,.T.);
#7283=ORIENTED_EDGE('',*,*,#5533,.F.);
#7284=ORIENTED_EDGE('',*,*,#5534,.T.);
#7285=ORIENTED_EDGE('',*,*,#5531,.T.);
#7286=ORIENTED_EDGE('',*,*,#5534,.F.);
#7287=ORIENTED_EDGE('',*,*,#5532,.F.);
#7288=ORIENTED_EDGE('',*,*,#5535,.T.);
#7289=ORIENTED_EDGE('',*,*,#5536,.F.);
#7290=ORIENTED_EDGE('',*,*,#5535,.F.);
#7291=ORIENTED_EDGE('',*,*,#5537,.F.);
#7292=ORIENTED_EDGE('',*,*,#5538,.T.);
#7293=ORIENTED_EDGE('',*,*,#5539,.F.);
#7294=ORIENTED_EDGE('',*,*,#5540,.T.);
#7295=ORIENTED_EDGE('',*,*,#5537,.T.);
#7296=ORIENTED_EDGE('',*,*,#5540,.F.);
#7297=ORIENTED_EDGE('',*,*,#5538,.F.);
#7298=ORIENTED_EDGE('',*,*,#5541,.T.);
#7299=ORIENTED_EDGE('',*,*,#5542,.F.);
#7300=ORIENTED_EDGE('',*,*,#5541,.F.);
#7301=ORIENTED_EDGE('',*,*,#5448,.F.);
#7302=ORIENTED_EDGE('',*,*,#5543,.T.);
#7303=ORIENTED_EDGE('',*,*,#5489,.T.);
#7304=ORIENTED_EDGE('',*,*,#5544,.T.);
#7305=ORIENTED_EDGE('',*,*,#5524,.T.);
#7306=ORIENTED_EDGE('',*,*,#5545,.T.);
#7307=ORIENTED_EDGE('',*,*,#5521,.F.);
#7308=ORIENTED_EDGE('',*,*,#5546,.F.);
#7309=ORIENTED_EDGE('',*,*,#5544,.F.);
#7310=ORIENTED_EDGE('',*,*,#5488,.F.);
#7311=ORIENTED_EDGE('',*,*,#5492,.F.);
#7312=ORIENTED_EDGE('',*,*,#5495,.F.);
#7313=ORIENTED_EDGE('',*,*,#5498,.F.);
#7314=ORIENTED_EDGE('',*,*,#5501,.F.);
#7315=ORIENTED_EDGE('',*,*,#5504,.F.);
#7316=ORIENTED_EDGE('',*,*,#5507,.F.);
#7317=ORIENTED_EDGE('',*,*,#5510,.F.);
#7318=ORIENTED_EDGE('',*,*,#5513,.F.);
#7319=ORIENTED_EDGE('',*,*,#5516,.F.);
#7320=ORIENTED_EDGE('',*,*,#5519,.F.);
#7321=ORIENTED_EDGE('',*,*,#5522,.F.);
#7322=ORIENTED_EDGE('',*,*,#5545,.F.);
#7323=ORIENTED_EDGE('',*,*,#5527,.F.);
#7324=ORIENTED_EDGE('',*,*,#5547,.F.);
#7325=ORIENTED_EDGE('',*,*,#5484,.F.);
#7326=ORIENTED_EDGE('',*,*,#5548,.F.);
#7327=ORIENTED_EDGE('',*,*,#5482,.F.);
#7328=ORIENTED_EDGE('',*,*,#5479,.F.);
#7329=ORIENTED_EDGE('',*,*,#5476,.F.);
#7330=ORIENTED_EDGE('',*,*,#5473,.F.);
#7331=ORIENTED_EDGE('',*,*,#5470,.F.);
#7332=ORIENTED_EDGE('',*,*,#5467,.F.);
#7333=ORIENTED_EDGE('',*,*,#5464,.F.);
#7334=ORIENTED_EDGE('',*,*,#5461,.F.);
#7335=ORIENTED_EDGE('',*,*,#5458,.F.);
#7336=ORIENTED_EDGE('',*,*,#5455,.F.);
#7337=ORIENTED_EDGE('',*,*,#5452,.F.);
#7338=ORIENTED_EDGE('',*,*,#5449,.F.);
#7339=ORIENTED_EDGE('',*,*,#5543,.F.);
#7340=ORIENTED_EDGE('',*,*,#5447,.F.);
#7341=ORIENTED_EDGE('',*,*,#5454,.F.);
#7342=ORIENTED_EDGE('',*,*,#5457,.F.);
#7343=ORIENTED_EDGE('',*,*,#5460,.F.);
#7344=ORIENTED_EDGE('',*,*,#5463,.F.);
#7345=ORIENTED_EDGE('',*,*,#5466,.F.);
#7346=ORIENTED_EDGE('',*,*,#5469,.F.);
#7347=ORIENTED_EDGE('',*,*,#5472,.F.);
#7348=ORIENTED_EDGE('',*,*,#5475,.F.);
#7349=ORIENTED_EDGE('',*,*,#5478,.F.);
#7350=ORIENTED_EDGE('',*,*,#5481,.F.);
#7351=ORIENTED_EDGE('',*,*,#5549,.F.);
#7352=ORIENTED_EDGE('',*,*,#5486,.F.);
#7353=ORIENTED_EDGE('',*,*,#5550,.F.);
#7354=ORIENTED_EDGE('',*,*,#5525,.T.);
#7355=ORIENTED_EDGE('',*,*,#5546,.T.);
#7356=ORIENTED_EDGE('',*,*,#5523,.T.);
#7357=ORIENTED_EDGE('',*,*,#5520,.T.);
#7358=ORIENTED_EDGE('',*,*,#5517,.T.);
#7359=ORIENTED_EDGE('',*,*,#5514,.T.);
#7360=ORIENTED_EDGE('',*,*,#5511,.T.);
#7361=ORIENTED_EDGE('',*,*,#5508,.T.);
#7362=ORIENTED_EDGE('',*,*,#5505,.T.);
#7363=ORIENTED_EDGE('',*,*,#5502,.T.);
#7364=ORIENTED_EDGE('',*,*,#5499,.T.);
#7365=ORIENTED_EDGE('',*,*,#5496,.T.);
#7366=ORIENTED_EDGE('',*,*,#5493,.T.);
#7367=ORIENTED_EDGE('',*,*,#5490,.T.);
#7368=ORIENTED_EDGE('',*,*,#5483,.T.);
#7369=ORIENTED_EDGE('',*,*,#5549,.T.);
#7370=ORIENTED_EDGE('',*,*,#5480,.F.);
#7371=ORIENTED_EDGE('',*,*,#5548,.T.);
#7372=ORIENTED_EDGE('',*,*,#5366,.F.);
#7373=ORIENTED_EDGE('',*,*,#5551,.T.);
#7374=ORIENTED_EDGE('',*,*,#5407,.T.);
#7375=ORIENTED_EDGE('',*,*,#5552,.T.);
#7376=ORIENTED_EDGE('',*,*,#5442,.T.);
#7377=ORIENTED_EDGE('',*,*,#5553,.T.);
#7378=ORIENTED_EDGE('',*,*,#5439,.F.);
#7379=ORIENTED_EDGE('',*,*,#5554,.F.);
#7380=ORIENTED_EDGE('',*,*,#5552,.F.);
#7381=ORIENTED_EDGE('',*,*,#5406,.F.);
#7382=ORIENTED_EDGE('',*,*,#5410,.F.);
#7383=ORIENTED_EDGE('',*,*,#5413,.F.);
#7384=ORIENTED_EDGE('',*,*,#5416,.F.);
#7385=ORIENTED_EDGE('',*,*,#5419,.F.);
#7386=ORIENTED_EDGE('',*,*,#5422,.F.);
#7387=ORIENTED_EDGE('',*,*,#5425,.F.);
#7388=ORIENTED_EDGE('',*,*,#5428,.F.);
#7389=ORIENTED_EDGE('',*,*,#5431,.F.);
#7390=ORIENTED_EDGE('',*,*,#5434,.F.);
#7391=ORIENTED_EDGE('',*,*,#5437,.F.);
#7392=ORIENTED_EDGE('',*,*,#5440,.F.);
#7393=ORIENTED_EDGE('',*,*,#5553,.F.);
#7394=ORIENTED_EDGE('',*,*,#5445,.F.);
#7395=ORIENTED_EDGE('',*,*,#5555,.F.);
#7396=ORIENTED_EDGE('',*,*,#5402,.F.);
#7397=ORIENTED_EDGE('',*,*,#5556,.F.);
#7398=ORIENTED_EDGE('',*,*,#5400,.F.);
#7399=ORIENTED_EDGE('',*,*,#5397,.F.);
#7400=ORIENTED_EDGE('',*,*,#5394,.F.);
#7401=ORIENTED_EDGE('',*,*,#5391,.F.);
#7402=ORIENTED_EDGE('',*,*,#5388,.F.);
#7403=ORIENTED_EDGE('',*,*,#5385,.F.);
#7404=ORIENTED_EDGE('',*,*,#5382,.F.);
#7405=ORIENTED_EDGE('',*,*,#5379,.F.);
#7406=ORIENTED_EDGE('',*,*,#5376,.F.);
#7407=ORIENTED_EDGE('',*,*,#5373,.F.);
#7408=ORIENTED_EDGE('',*,*,#5370,.F.);
#7409=ORIENTED_EDGE('',*,*,#5367,.F.);
#7410=ORIENTED_EDGE('',*,*,#5551,.F.);
#7411=ORIENTED_EDGE('',*,*,#5365,.F.);
#7412=ORIENTED_EDGE('',*,*,#5372,.F.);
#7413=ORIENTED_EDGE('',*,*,#5375,.F.);
#7414=ORIENTED_EDGE('',*,*,#5378,.F.);
#7415=ORIENTED_EDGE('',*,*,#5381,.F.);
#7416=ORIENTED_EDGE('',*,*,#5384,.F.);
#7417=ORIENTED_EDGE('',*,*,#5387,.F.);
#7418=ORIENTED_EDGE('',*,*,#5390,.F.);
#7419=ORIENTED_EDGE('',*,*,#5393,.F.);
#7420=ORIENTED_EDGE('',*,*,#5396,.F.);
#7421=ORIENTED_EDGE('',*,*,#5399,.F.);
#7422=ORIENTED_EDGE('',*,*,#5557,.F.);
#7423=ORIENTED_EDGE('',*,*,#5404,.F.);
#7424=ORIENTED_EDGE('',*,*,#5558,.F.);
#7425=ORIENTED_EDGE('',*,*,#5443,.T.);
#7426=ORIENTED_EDGE('',*,*,#5554,.T.);
#7427=ORIENTED_EDGE('',*,*,#5441,.T.);
#7428=ORIENTED_EDGE('',*,*,#5438,.T.);
#7429=ORIENTED_EDGE('',*,*,#5435,.T.);
#7430=ORIENTED_EDGE('',*,*,#5432,.T.);
#7431=ORIENTED_EDGE('',*,*,#5429,.T.);
#7432=ORIENTED_EDGE('',*,*,#5426,.T.);
#7433=ORIENTED_EDGE('',*,*,#5423,.T.);
#7434=ORIENTED_EDGE('',*,*,#5420,.T.);
#7435=ORIENTED_EDGE('',*,*,#5417,.T.);
#7436=ORIENTED_EDGE('',*,*,#5414,.T.);
#7437=ORIENTED_EDGE('',*,*,#5411,.T.);
#7438=ORIENTED_EDGE('',*,*,#5408,.T.);
#7439=ORIENTED_EDGE('',*,*,#5401,.T.);
#7440=ORIENTED_EDGE('',*,*,#5557,.T.);
#7441=ORIENTED_EDGE('',*,*,#5398,.F.);
#7442=ORIENTED_EDGE('',*,*,#5556,.T.);
#7443=ORIENTED_EDGE('',*,*,#5284,.F.);
#7444=ORIENTED_EDGE('',*,*,#5559,.T.);
#7445=ORIENTED_EDGE('',*,*,#5325,.T.);
#7446=ORIENTED_EDGE('',*,*,#5560,.T.);
#7447=ORIENTED_EDGE('',*,*,#5360,.T.);
#7448=ORIENTED_EDGE('',*,*,#5561,.T.);
#7449=ORIENTED_EDGE('',*,*,#5357,.F.);
#7450=ORIENTED_EDGE('',*,*,#5562,.F.);
#7451=ORIENTED_EDGE('',*,*,#5560,.F.);
#7452=ORIENTED_EDGE('',*,*,#5324,.F.);
#7453=ORIENTED_EDGE('',*,*,#5328,.F.);
#7454=ORIENTED_EDGE('',*,*,#5331,.F.);
#7455=ORIENTED_EDGE('',*,*,#5334,.F.);
#7456=ORIENTED_EDGE('',*,*,#5337,.F.);
#7457=ORIENTED_EDGE('',*,*,#5340,.F.);
#7458=ORIENTED_EDGE('',*,*,#5343,.F.);
#7459=ORIENTED_EDGE('',*,*,#5346,.F.);
#7460=ORIENTED_EDGE('',*,*,#5349,.F.);
#7461=ORIENTED_EDGE('',*,*,#5352,.F.);
#7462=ORIENTED_EDGE('',*,*,#5355,.F.);
#7463=ORIENTED_EDGE('',*,*,#5358,.F.);
#7464=ORIENTED_EDGE('',*,*,#5561,.F.);
#7465=ORIENTED_EDGE('',*,*,#5363,.F.);
#7466=ORIENTED_EDGE('',*,*,#5563,.F.);
#7467=ORIENTED_EDGE('',*,*,#5320,.F.);
#7468=ORIENTED_EDGE('',*,*,#5564,.F.);
#7469=ORIENTED_EDGE('',*,*,#5318,.F.);
#7470=ORIENTED_EDGE('',*,*,#5315,.F.);
#7471=ORIENTED_EDGE('',*,*,#5312,.F.);
#7472=ORIENTED_EDGE('',*,*,#5309,.F.);
#7473=ORIENTED_EDGE('',*,*,#5306,.F.);
#7474=ORIENTED_EDGE('',*,*,#5303,.F.);
#7475=ORIENTED_EDGE('',*,*,#5300,.F.);
#7476=ORIENTED_EDGE('',*,*,#5297,.F.);
#7477=ORIENTED_EDGE('',*,*,#5294,.F.);
#7478=ORIENTED_EDGE('',*,*,#5291,.F.);
#7479=ORIENTED_EDGE('',*,*,#5288,.F.);
#7480=ORIENTED_EDGE('',*,*,#5285,.F.);
#7481=ORIENTED_EDGE('',*,*,#5559,.F.);
#7482=ORIENTED_EDGE('',*,*,#5283,.F.);
#7483=ORIENTED_EDGE('',*,*,#5290,.F.);
#7484=ORIENTED_EDGE('',*,*,#5293,.F.);
#7485=ORIENTED_EDGE('',*,*,#5296,.F.);
#7486=ORIENTED_EDGE('',*,*,#5299,.F.);
#7487=ORIENTED_EDGE('',*,*,#5302,.F.);
#7488=ORIENTED_EDGE('',*,*,#5305,.F.);
#7489=ORIENTED_EDGE('',*,*,#5308,.F.);
#7490=ORIENTED_EDGE('',*,*,#5311,.F.);
#7491=ORIENTED_EDGE('',*,*,#5314,.F.);
#7492=ORIENTED_EDGE('',*,*,#5317,.F.);
#7493=ORIENTED_EDGE('',*,*,#5565,.F.);
#7494=ORIENTED_EDGE('',*,*,#5322,.F.);
#7495=ORIENTED_EDGE('',*,*,#5566,.F.);
#7496=ORIENTED_EDGE('',*,*,#5361,.T.);
#7497=ORIENTED_EDGE('',*,*,#5562,.T.);
#7498=ORIENTED_EDGE('',*,*,#5359,.T.);
#7499=ORIENTED_EDGE('',*,*,#5356,.T.);
#7500=ORIENTED_EDGE('',*,*,#5353,.T.);
#7501=ORIENTED_EDGE('',*,*,#5350,.T.);
#7502=ORIENTED_EDGE('',*,*,#5347,.T.);
#7503=ORIENTED_EDGE('',*,*,#5344,.T.);
#7504=ORIENTED_EDGE('',*,*,#5341,.T.);
#7505=ORIENTED_EDGE('',*,*,#5338,.T.);
#7506=ORIENTED_EDGE('',*,*,#5335,.T.);
#7507=ORIENTED_EDGE('',*,*,#5332,.T.);
#7508=ORIENTED_EDGE('',*,*,#5329,.T.);
#7509=ORIENTED_EDGE('',*,*,#5326,.T.);
#7510=ORIENTED_EDGE('',*,*,#5319,.T.);
#7511=ORIENTED_EDGE('',*,*,#5565,.T.);
#7512=ORIENTED_EDGE('',*,*,#5316,.F.);
#7513=ORIENTED_EDGE('',*,*,#5564,.T.);
#7514=ORIENTED_EDGE('',*,*,#5202,.F.);
#7515=ORIENTED_EDGE('',*,*,#5567,.T.);
#7516=ORIENTED_EDGE('',*,*,#5243,.T.);
#7517=ORIENTED_EDGE('',*,*,#5568,.T.);
#7518=ORIENTED_EDGE('',*,*,#5278,.T.);
#7519=ORIENTED_EDGE('',*,*,#5569,.T.);
#7520=ORIENTED_EDGE('',*,*,#5275,.F.);
#7521=ORIENTED_EDGE('',*,*,#5570,.F.);
#7522=ORIENTED_EDGE('',*,*,#5568,.F.);
#7523=ORIENTED_EDGE('',*,*,#5242,.F.);
#7524=ORIENTED_EDGE('',*,*,#5246,.F.);
#7525=ORIENTED_EDGE('',*,*,#5249,.F.);
#7526=ORIENTED_EDGE('',*,*,#5252,.F.);
#7527=ORIENTED_EDGE('',*,*,#5255,.F.);
#7528=ORIENTED_EDGE('',*,*,#5258,.F.);
#7529=ORIENTED_EDGE('',*,*,#5261,.F.);
#7530=ORIENTED_EDGE('',*,*,#5264,.F.);
#7531=ORIENTED_EDGE('',*,*,#5267,.F.);
#7532=ORIENTED_EDGE('',*,*,#5270,.F.);
#7533=ORIENTED_EDGE('',*,*,#5273,.F.);
#7534=ORIENTED_EDGE('',*,*,#5276,.F.);
#7535=ORIENTED_EDGE('',*,*,#5569,.F.);
#7536=ORIENTED_EDGE('',*,*,#5281,.F.);
#7537=ORIENTED_EDGE('',*,*,#5571,.F.);
#7538=ORIENTED_EDGE('',*,*,#5238,.F.);
#7539=ORIENTED_EDGE('',*,*,#5572,.F.);
#7540=ORIENTED_EDGE('',*,*,#5236,.F.);
#7541=ORIENTED_EDGE('',*,*,#5233,.F.);
#7542=ORIENTED_EDGE('',*,*,#5230,.F.);
#7543=ORIENTED_EDGE('',*,*,#5227,.F.);
#7544=ORIENTED_EDGE('',*,*,#5224,.F.);
#7545=ORIENTED_EDGE('',*,*,#5221,.F.);
#7546=ORIENTED_EDGE('',*,*,#5218,.F.);
#7547=ORIENTED_EDGE('',*,*,#5215,.F.);
#7548=ORIENTED_EDGE('',*,*,#5212,.F.);
#7549=ORIENTED_EDGE('',*,*,#5209,.F.);
#7550=ORIENTED_EDGE('',*,*,#5206,.F.);
#7551=ORIENTED_EDGE('',*,*,#5203,.F.);
#7552=ORIENTED_EDGE('',*,*,#5567,.F.);
#7553=ORIENTED_EDGE('',*,*,#5201,.F.);
#7554=ORIENTED_EDGE('',*,*,#5208,.F.);
#7555=ORIENTED_EDGE('',*,*,#5211,.F.);
#7556=ORIENTED_EDGE('',*,*,#5214,.F.);
#7557=ORIENTED_EDGE('',*,*,#5217,.F.);
#7558=ORIENTED_EDGE('',*,*,#5220,.F.);
#7559=ORIENTED_EDGE('',*,*,#5223,.F.);
#7560=ORIENTED_EDGE('',*,*,#5226,.F.);
#7561=ORIENTED_EDGE('',*,*,#5229,.F.);
#7562=ORIENTED_EDGE('',*,*,#5232,.F.);
#7563=ORIENTED_EDGE('',*,*,#5235,.F.);
#7564=ORIENTED_EDGE('',*,*,#5573,.F.);
#7565=ORIENTED_EDGE('',*,*,#5240,.F.);
#7566=ORIENTED_EDGE('',*,*,#5574,.F.);
#7567=ORIENTED_EDGE('',*,*,#5279,.T.);
#7568=ORIENTED_EDGE('',*,*,#5570,.T.);
#7569=ORIENTED_EDGE('',*,*,#5277,.T.);
#7570=ORIENTED_EDGE('',*,*,#5274,.T.);
#7571=ORIENTED_EDGE('',*,*,#5271,.T.);
#7572=ORIENTED_EDGE('',*,*,#5268,.T.);
#7573=ORIENTED_EDGE('',*,*,#5265,.T.);
#7574=ORIENTED_EDGE('',*,*,#5262,.T.);
#7575=ORIENTED_EDGE('',*,*,#5259,.T.);
#7576=ORIENTED_EDGE('',*,*,#5256,.T.);
#7577=ORIENTED_EDGE('',*,*,#5253,.T.);
#7578=ORIENTED_EDGE('',*,*,#5250,.T.);
#7579=ORIENTED_EDGE('',*,*,#5247,.T.);
#7580=ORIENTED_EDGE('',*,*,#5244,.T.);
#7581=ORIENTED_EDGE('',*,*,#5237,.T.);
#7582=ORIENTED_EDGE('',*,*,#5573,.T.);
#7583=ORIENTED_EDGE('',*,*,#5234,.F.);
#7584=ORIENTED_EDGE('',*,*,#5572,.T.);
#7585=ORIENTED_EDGE('',*,*,#5287,.F.);
#7586=ORIENTED_EDGE('',*,*,#5205,.F.);
#7587=ORIENTED_EDGE('',*,*,#5451,.F.);
#7588=ORIENTED_EDGE('',*,*,#5369,.F.);
#7589=ORIENTED_EDGE('',*,*,#5575,.F.);
#7590=ORIENTED_EDGE('',*,*,#5576,.T.);
#7591=ORIENTED_EDGE('',*,*,#5577,.F.);
#7592=ORIENTED_EDGE('',*,*,#5576,.F.);
#7593=ORIENTED_EDGE('',*,*,#5578,.F.);
#7594=ORIENTED_EDGE('',*,*,#5579,.T.);
#7595=ORIENTED_EDGE('',*,*,#5580,.F.);
#7596=ORIENTED_EDGE('',*,*,#5579,.F.);
#7597=ORIENTED_EDGE('',*,*,#5581,.T.);
#7598=ORIENTED_EDGE('',*,*,#5582,.F.);
#7599=ORIENTED_EDGE('',*,*,#5583,.F.);
#7600=ORIENTED_EDGE('',*,*,#5584,.F.);
#7601=ORIENTED_EDGE('',*,*,#5585,.T.);
#7602=ORIENTED_EDGE('',*,*,#5584,.T.);
#7603=ORIENTED_EDGE('',*,*,#5586,.F.);
#7604=ORIENTED_EDGE('',*,*,#5587,.F.);
#7605=ORIENTED_EDGE('',*,*,#5588,.T.);
#7606=ORIENTED_EDGE('',*,*,#5587,.T.);
#7607=ORIENTED_EDGE('',*,*,#5589,.F.);
#7608=ORIENTED_EDGE('',*,*,#5590,.F.);
#7609=ORIENTED_EDGE('',*,*,#5591,.F.);
#7610=ORIENTED_EDGE('',*,*,#5589,.T.);
#7611=ORIENTED_EDGE('',*,*,#5586,.T.);
#7612=ORIENTED_EDGE('',*,*,#5583,.T.);
#7613=ORIENTED_EDGE('',*,*,#5578,.T.);
#7614=ORIENTED_EDGE('',*,*,#5592,.T.);
#7615=ORIENTED_EDGE('',*,*,#5593,.T.);
#7616=ORIENTED_EDGE('',*,*,#5594,.F.);
#7617=ORIENTED_EDGE('',*,*,#5595,.F.);
#7618=ORIENTED_EDGE('',*,*,#5596,.T.);
#7619=ORIENTED_EDGE('',*,*,#5597,.F.);
#7620=ORIENTED_EDGE('',*,*,#5598,.F.);
#7621=ORIENTED_EDGE('',*,*,#5599,.F.);
#7622=ORIENTED_EDGE('',*,*,#5600,.T.);
#7623=ORIENTED_EDGE('',*,*,#5599,.T.);
#7624=ORIENTED_EDGE('',*,*,#5601,.F.);
#7625=ORIENTED_EDGE('',*,*,#5593,.F.);
#7626=ORIENTED_EDGE('',*,*,#5601,.T.);
#7627=ORIENTED_EDGE('',*,*,#5598,.T.);
#7628=ORIENTED_EDGE('',*,*,#5602,.F.);
#7629=ORIENTED_EDGE('',*,*,#5594,.T.);
#7630=ORIENTED_EDGE('',*,*,#5575,.T.);
#7631=ORIENTED_EDGE('',*,*,#5603,.F.);
#7632=ORIENTED_EDGE('',*,*,#5604,.T.);
#7633=ORIENTED_EDGE('',*,*,#5605,.F.);
#7634=ORIENTED_EDGE('',*,*,#5604,.F.);
#7635=ORIENTED_EDGE('',*,*,#5606,.F.);
#7636=ORIENTED_EDGE('',*,*,#5607,.T.);
#7637=ORIENTED_EDGE('',*,*,#5608,.F.);
#7638=ORIENTED_EDGE('',*,*,#5607,.F.);
#7639=ORIENTED_EDGE('',*,*,#5606,.T.);
#7640=ORIENTED_EDGE('',*,*,#5603,.T.);
#7641=ORIENTED_EDGE('',*,*,#5609,.T.);
#7642=ORIENTED_EDGE('',*,*,#5610,.F.);
#7643=ORIENTED_EDGE('',*,*,#5611,.T.);
#7644=ORIENTED_EDGE('',*,*,#5612,.F.);
#7645=ORIENTED_EDGE('',*,*,#5613,.T.);
#7646=ORIENTED_EDGE('',*,*,#5614,.F.);
#7647=ORIENTED_EDGE('',*,*,#5615,.T.);
#7648=ORIENTED_EDGE('',*,*,#5616,.F.);
#7649=ORIENTED_EDGE('',*,*,#5536,.T.);
#7650=ORIENTED_EDGE('',*,*,#5542,.T.);
#7651=ORIENTED_EDGE('',*,*,#5608,.T.);
#7652=ORIENTED_EDGE('',*,*,#5609,.F.);
#7653=ORIENTED_EDGE('',*,*,#5617,.T.);
#7654=ORIENTED_EDGE('',*,*,#5618,.T.);
#7655=ORIENTED_EDGE('',*,*,#5619,.T.);
#7656=ORIENTED_EDGE('',*,*,#5617,.F.);
#7657=ORIENTED_EDGE('',*,*,#5616,.T.);
#7658=ORIENTED_EDGE('',*,*,#5620,.F.);
#7659=ORIENTED_EDGE('',*,*,#5621,.F.);
#7660=ORIENTED_EDGE('',*,*,#5615,.F.);
#7661=ORIENTED_EDGE('',*,*,#5622,.T.);
#7662=ORIENTED_EDGE('',*,*,#5623,.T.);
#7663=ORIENTED_EDGE('',*,*,#5620,.T.);
#7664=ORIENTED_EDGE('',*,*,#5622,.F.);
#7665=ORIENTED_EDGE('',*,*,#5614,.T.);
#7666=ORIENTED_EDGE('',*,*,#5624,.F.);
#7667=ORIENTED_EDGE('',*,*,#5625,.F.);
#7668=ORIENTED_EDGE('',*,*,#5611,.F.);
#7669=ORIENTED_EDGE('',*,*,#5626,.T.);
#7670=ORIENTED_EDGE('',*,*,#5627,.T.);
#7671=ORIENTED_EDGE('',*,*,#5628,.T.);
#7672=ORIENTED_EDGE('',*,*,#5605,.T.);
#7673=ORIENTED_EDGE('',*,*,#5628,.F.);
#7674=ORIENTED_EDGE('',*,*,#5629,.F.);
#7675=ORIENTED_EDGE('',*,*,#5630,.F.);
#7676=ORIENTED_EDGE('',*,*,#5612,.T.);
#7677=ORIENTED_EDGE('',*,*,#5530,.T.);
#7678=ORIENTED_EDGE('',*,*,#5613,.F.);
#7679=ORIENTED_EDGE('',*,*,#5630,.T.);
#7680=ORIENTED_EDGE('',*,*,#5631,.T.);
#7681=ORIENTED_EDGE('',*,*,#5624,.T.);
#7682=ORIENTED_EDGE('',*,*,#5619,.F.);
#7683=ORIENTED_EDGE('',*,*,#5632,.F.);
#7684=ORIENTED_EDGE('',*,*,#5626,.F.);
#7685=ORIENTED_EDGE('',*,*,#5610,.T.);
#7686=ORIENTED_EDGE('',*,*,#5633,.T.);
#7687=ORIENTED_EDGE('',*,*,#5634,.T.);
#7688=ORIENTED_EDGE('',*,*,#5635,.F.);
#7689=ORIENTED_EDGE('',*,*,#5636,.F.);
#7690=ORIENTED_EDGE('',*,*,#5582,.T.);
#7691=ORIENTED_EDGE('',*,*,#5637,.T.);
#7692=ORIENTED_EDGE('',*,*,#5636,.T.);
#7693=ORIENTED_EDGE('',*,*,#5638,.F.);
#7694=ORIENTED_EDGE('',*,*,#5639,.F.);
#7695=ORIENTED_EDGE('',*,*,#5640,.T.);
#7696=ORIENTED_EDGE('',*,*,#5590,.T.);
#7697=ORIENTED_EDGE('',*,*,#5591,.T.);
#7698=ORIENTED_EDGE('',*,*,#5641,.T.);
#7699=ORIENTED_EDGE('',*,*,#5639,.T.);
#7700=ORIENTED_EDGE('',*,*,#5642,.F.);
#7701=ORIENTED_EDGE('',*,*,#5643,.F.);
#7702=ORIENTED_EDGE('',*,*,#5528,.T.);
#7703=ORIENTED_EDGE('',*,*,#5597,.T.);
#7704=ORIENTED_EDGE('',*,*,#5644,.T.);
#7705=ORIENTED_EDGE('',*,*,#5643,.T.);
#7706=ORIENTED_EDGE('',*,*,#5645,.F.);
#7707=ORIENTED_EDGE('',*,*,#5634,.F.);
#7708=ORIENTED_EDGE('',*,*,#5646,.T.);
#7709=ORIENTED_EDGE('',*,*,#5595,.T.);
#7710=ORIENTED_EDGE('',*,*,#5602,.T.);
#7711=ORIENTED_EDGE('',*,*,#5645,.T.);
#7712=ORIENTED_EDGE('',*,*,#5642,.T.);
#7713=ORIENTED_EDGE('',*,*,#5638,.T.);
#7714=ORIENTED_EDGE('',*,*,#5635,.T.);
#7715=ORIENTED_EDGE('',*,*,#5550,.T.);
#7716=ORIENTED_EDGE('',*,*,#5485,.T.);
#7717=ORIENTED_EDGE('',*,*,#5547,.T.);
#7718=ORIENTED_EDGE('',*,*,#5526,.T.);
#7719=ORIENTED_EDGE('',*,*,#5558,.T.);
#7720=ORIENTED_EDGE('',*,*,#5403,.T.);
#7721=ORIENTED_EDGE('',*,*,#5555,.T.);
#7722=ORIENTED_EDGE('',*,*,#5444,.T.);
#7723=ORIENTED_EDGE('',*,*,#5566,.T.);
#7724=ORIENTED_EDGE('',*,*,#5321,.T.);
#7725=ORIENTED_EDGE('',*,*,#5563,.T.);
#7726=ORIENTED_EDGE('',*,*,#5362,.T.);
#7727=ORIENTED_EDGE('',*,*,#5574,.T.);
#7728=ORIENTED_EDGE('',*,*,#5239,.T.);
#7729=ORIENTED_EDGE('',*,*,#5571,.T.);
#7730=ORIENTED_EDGE('',*,*,#5280,.T.);
#7731=ORIENTED_EDGE('',*,*,#5629,.T.);
#7732=ORIENTED_EDGE('',*,*,#5627,.F.);
#7733=ORIENTED_EDGE('',*,*,#5632,.T.);
#7734=ORIENTED_EDGE('',*,*,#5618,.F.);
#7735=ORIENTED_EDGE('',*,*,#5621,.T.);
#7736=ORIENTED_EDGE('',*,*,#5623,.F.);
#7737=ORIENTED_EDGE('',*,*,#5625,.T.);
#7738=ORIENTED_EDGE('',*,*,#5631,.F.);
#7739=ORIENTED_EDGE('',*,*,#5646,.F.);
#7740=ORIENTED_EDGE('',*,*,#5633,.F.);
#7741=ORIENTED_EDGE('',*,*,#5637,.F.);
#7742=ORIENTED_EDGE('',*,*,#5581,.F.);
#7743=ORIENTED_EDGE('',*,*,#5585,.F.);
#7744=ORIENTED_EDGE('',*,*,#5588,.F.);
#7745=ORIENTED_EDGE('',*,*,#5640,.F.);
#7746=ORIENTED_EDGE('',*,*,#5641,.F.);
#7747=ORIENTED_EDGE('',*,*,#5644,.F.);
#7748=ORIENTED_EDGE('',*,*,#5596,.F.);
#7749=ORIENTED_EDGE('',*,*,#5600,.F.);
#7750=ORIENTED_EDGE('',*,*,#5592,.F.);
#7751=ORIENTED_EDGE('',*,*,#5533,.T.);
#7752=ORIENTED_EDGE('',*,*,#5539,.T.);
#7753=ORIENTED_EDGE('',*,*,#5577,.T.);
#7754=ORIENTED_EDGE('',*,*,#5580,.T.);
#7755=ORIENTED_EDGE('',*,*,#5647,.T.);
#7756=ORIENTED_EDGE('',*,*,#5648,.T.);
#7757=ORIENTED_EDGE('',*,*,#5649,.T.);
#7758=ORIENTED_EDGE('',*,*,#5650,.T.);
#7759=ORIENTED_EDGE('',*,*,#5651,.T.);
#7760=ORIENTED_EDGE('',*,*,#5652,.T.);
#7761=ORIENTED_EDGE('',*,*,#5647,.F.);
#7762=ORIENTED_EDGE('',*,*,#5653,.T.);
#7763=ORIENTED_EDGE('',*,*,#5654,.F.);
#7764=ORIENTED_EDGE('',*,*,#5655,.T.);
#7765=ORIENTED_EDGE('',*,*,#5656,.F.);
#7766=ORIENTED_EDGE('',*,*,#5657,.T.);
#7767=ORIENTED_EDGE('',*,*,#5658,.T.);
#7768=ORIENTED_EDGE('',*,*,#5659,.T.);
#7769=ORIENTED_EDGE('',*,*,#5660,.T.);
#7770=ORIENTED_EDGE('',*,*,#5661,.T.);
#7771=ORIENTED_EDGE('',*,*,#5662,.T.);
#7772=ORIENTED_EDGE('',*,*,#5663,.T.);
#7773=ORIENTED_EDGE('',*,*,#5658,.F.);
#7774=ORIENTED_EDGE('',*,*,#5664,.T.);
#7775=ORIENTED_EDGE('',*,*,#5665,.F.);
#7776=ORIENTED_EDGE('',*,*,#5666,.T.);
#7777=ORIENTED_EDGE('',*,*,#5667,.F.);
#7778=ORIENTED_EDGE('',*,*,#5668,.T.);
#7779=ORIENTED_EDGE('',*,*,#5669,.T.);
#7780=ORIENTED_EDGE('',*,*,#5670,.T.);
#7781=ORIENTED_EDGE('',*,*,#5671,.F.);
#7782=ORIENTED_EDGE('',*,*,#5672,.F.);
#7783=ORIENTED_EDGE('',*,*,#5673,.T.);
#7784=ORIENTED_EDGE('',*,*,#5674,.T.);
#7785=ORIENTED_EDGE('',*,*,#5669,.F.);
#7786=ORIENTED_EDGE('',*,*,#5675,.F.);
#7787=ORIENTED_EDGE('',*,*,#5676,.T.);
#7788=ORIENTED_EDGE('',*,*,#5677,.T.);
#7789=ORIENTED_EDGE('',*,*,#5673,.F.);
#7790=ORIENTED_EDGE('',*,*,#5678,.F.);
#7791=ORIENTED_EDGE('',*,*,#5679,.F.);
#7792=ORIENTED_EDGE('',*,*,#5680,.F.);
#7793=ORIENTED_EDGE('',*,*,#5681,.F.);
#7794=ORIENTED_EDGE('',*,*,#5682,.T.);
#7795=ORIENTED_EDGE('',*,*,#5683,.T.);
#7796=ORIENTED_EDGE('',*,*,#5684,.T.);
#7797=ORIENTED_EDGE('',*,*,#5685,.F.);
#7798=ORIENTED_EDGE('',*,*,#5686,.F.);
#7799=ORIENTED_EDGE('',*,*,#5687,.T.);
#7800=ORIENTED_EDGE('',*,*,#5688,.T.);
#7801=ORIENTED_EDGE('',*,*,#5683,.F.);
#7802=ORIENTED_EDGE('',*,*,#5689,.F.);
#7803=ORIENTED_EDGE('',*,*,#5690,.T.);
#7804=ORIENTED_EDGE('',*,*,#5691,.T.);
#7805=ORIENTED_EDGE('',*,*,#5687,.F.);
#7806=ORIENTED_EDGE('',*,*,#5692,.F.);
#7807=ORIENTED_EDGE('',*,*,#5693,.F.);
#7808=ORIENTED_EDGE('',*,*,#5694,.F.);
#7809=ORIENTED_EDGE('',*,*,#5695,.F.);
#7810=ORIENTED_EDGE('',*,*,#5696,.T.);
#7811=ORIENTED_EDGE('',*,*,#5697,.F.);
#7812=ORIENTED_EDGE('',*,*,#5698,.T.);
#7813=ORIENTED_EDGE('',*,*,#5699,.F.);
#7814=ORIENTED_EDGE('',*,*,#5700,.T.);
#7815=ORIENTED_EDGE('',*,*,#5701,.F.);
#7816=ORIENTED_EDGE('',*,*,#5702,.F.);
#7817=ORIENTED_EDGE('',*,*,#5703,.T.);
#7818=ORIENTED_EDGE('',*,*,#5704,.T.);
#7819=ORIENTED_EDGE('',*,*,#5705,.F.);
#7820=ORIENTED_EDGE('',*,*,#5706,.F.);
#7821=ORIENTED_EDGE('',*,*,#5707,.T.);
#7822=ORIENTED_EDGE('',*,*,#5708,.T.);
#7823=ORIENTED_EDGE('',*,*,#5709,.F.);
#7824=ORIENTED_EDGE('',*,*,#5710,.F.);
#7825=ORIENTED_EDGE('',*,*,#5711,.T.);
#7826=ORIENTED_EDGE('',*,*,#5710,.T.);
#7827=ORIENTED_EDGE('',*,*,#5712,.F.);
#7828=ORIENTED_EDGE('',*,*,#5713,.T.);
#7829=ORIENTED_EDGE('',*,*,#5702,.T.);
#7830=ORIENTED_EDGE('',*,*,#5714,.F.);
#7831=ORIENTED_EDGE('',*,*,#5715,.F.);
#7832=ORIENTED_EDGE('',*,*,#5716,.T.);
#7833=ORIENTED_EDGE('',*,*,#5717,.T.);
#7834=ORIENTED_EDGE('',*,*,#5718,.F.);
#7835=ORIENTED_EDGE('',*,*,#5698,.F.);
#7836=ORIENTED_EDGE('',*,*,#5719,.F.);
#7837=ORIENTED_EDGE('',*,*,#5720,.F.);
#7838=ORIENTED_EDGE('',*,*,#5704,.F.);
#7839=ORIENTED_EDGE('',*,*,#5720,.T.);
#7840=ORIENTED_EDGE('',*,*,#5721,.F.);
#7841=ORIENTED_EDGE('',*,*,#5699,.T.);
#7842=ORIENTED_EDGE('',*,*,#5718,.T.);
#7843=ORIENTED_EDGE('',*,*,#5722,.T.);
#7844=ORIENTED_EDGE('',*,*,#5714,.T.);
#7845=ORIENTED_EDGE('',*,*,#5701,.T.);
#7846=ORIENTED_EDGE('',*,*,#5723,.F.);
#7847=ORIENTED_EDGE('',*,*,#5712,.T.);
#7848=ORIENTED_EDGE('',*,*,#5709,.T.);
#7849=ORIENTED_EDGE('',*,*,#5724,.T.);
#7850=ORIENTED_EDGE('',*,*,#5705,.T.);
#7851=ORIENTED_EDGE('',*,*,#5725,.T.);
#7852=ORIENTED_EDGE('',*,*,#5723,.T.);
#7853=ORIENTED_EDGE('',*,*,#5726,.T.);
#7854=ORIENTED_EDGE('',*,*,#5693,.T.);
#7855=ORIENTED_EDGE('',*,*,#5727,.T.);
#7856=ORIENTED_EDGE('',*,*,#5690,.F.);
#7857=ORIENTED_EDGE('',*,*,#5728,.F.);
#7858=ORIENTED_EDGE('',*,*,#5729,.F.);
#7859=ORIENTED_EDGE('',*,*,#5684,.F.);
#7860=ORIENTED_EDGE('',*,*,#5688,.F.);
#7861=ORIENTED_EDGE('',*,*,#5691,.F.);
#7862=ORIENTED_EDGE('',*,*,#5727,.F.);
#7863=ORIENTED_EDGE('',*,*,#5696,.F.);
#7864=ORIENTED_EDGE('',*,*,#5730,.F.);
#7865=ORIENTED_EDGE('',*,*,#5666,.F.);
#7866=ORIENTED_EDGE('',*,*,#5731,.F.);
#7867=ORIENTED_EDGE('',*,*,#5664,.F.);
#7868=ORIENTED_EDGE('',*,*,#5661,.F.);
#7869=ORIENTED_EDGE('',*,*,#5732,.F.);
#7870=ORIENTED_EDGE('',*,*,#5659,.F.);
#7871=ORIENTED_EDGE('',*,*,#5663,.F.);
#7872=ORIENTED_EDGE('',*,*,#5733,.F.);
#7873=ORIENTED_EDGE('',*,*,#5668,.F.);
#7874=ORIENTED_EDGE('',*,*,#5734,.F.);
#7875=ORIENTED_EDGE('',*,*,#5694,.T.);
#7876=ORIENTED_EDGE('',*,*,#5728,.T.);
#7877=ORIENTED_EDGE('',*,*,#5692,.T.);
#7878=ORIENTED_EDGE('',*,*,#5689,.T.);
#7879=ORIENTED_EDGE('',*,*,#5686,.T.);
#7880=ORIENTED_EDGE('',*,*,#5679,.T.);
#7881=ORIENTED_EDGE('',*,*,#5735,.T.);
#7882=ORIENTED_EDGE('',*,*,#5676,.F.);
#7883=ORIENTED_EDGE('',*,*,#5736,.F.);
#7884=ORIENTED_EDGE('',*,*,#5737,.F.);
#7885=ORIENTED_EDGE('',*,*,#5670,.F.);
#7886=ORIENTED_EDGE('',*,*,#5674,.F.);
#7887=ORIENTED_EDGE('',*,*,#5677,.F.);
#7888=ORIENTED_EDGE('',*,*,#5735,.F.);
#7889=ORIENTED_EDGE('',*,*,#5682,.F.);
#7890=ORIENTED_EDGE('',*,*,#5738,.F.);
#7891=ORIENTED_EDGE('',*,*,#5655,.F.);
#7892=ORIENTED_EDGE('',*,*,#5739,.F.);
#7893=ORIENTED_EDGE('',*,*,#5653,.F.);
#7894=ORIENTED_EDGE('',*,*,#5650,.F.);
#7895=ORIENTED_EDGE('',*,*,#5740,.F.);
#7896=ORIENTED_EDGE('',*,*,#5648,.F.);
#7897=ORIENTED_EDGE('',*,*,#5652,.F.);
#7898=ORIENTED_EDGE('',*,*,#5741,.F.);
#7899=ORIENTED_EDGE('',*,*,#5657,.F.);
#7900=ORIENTED_EDGE('',*,*,#5742,.F.);
#7901=ORIENTED_EDGE('',*,*,#5680,.T.);
#7902=ORIENTED_EDGE('',*,*,#5736,.T.);
#7903=ORIENTED_EDGE('',*,*,#5678,.T.);
#7904=ORIENTED_EDGE('',*,*,#5675,.T.);
#7905=ORIENTED_EDGE('',*,*,#5672,.T.);
#7906=ORIENTED_EDGE('',*,*,#5665,.T.);
#7907=ORIENTED_EDGE('',*,*,#5733,.T.);
#7908=ORIENTED_EDGE('',*,*,#5662,.F.);
#7909=ORIENTED_EDGE('',*,*,#5731,.T.);
#7910=ORIENTED_EDGE('',*,*,#5732,.T.);
#7911=ORIENTED_EDGE('',*,*,#5685,.T.);
#7912=ORIENTED_EDGE('',*,*,#5729,.T.);
#7913=ORIENTED_EDGE('',*,*,#5660,.F.);
#7914=ORIENTED_EDGE('',*,*,#5743,.F.);
#7915=ORIENTED_EDGE('',*,*,#5743,.T.);
#7916=ORIENTED_EDGE('',*,*,#5744,.T.);
#7917=ORIENTED_EDGE('',*,*,#5745,.T.);
#7918=ORIENTED_EDGE('',*,*,#5744,.F.);
#7919=ORIENTED_EDGE('',*,*,#5745,.F.);
#7920=ORIENTED_EDGE('',*,*,#5746,.F.);
#7921=ORIENTED_EDGE('',*,*,#5746,.T.);
#7922=ORIENTED_EDGE('',*,*,#5747,.T.);
#7923=ORIENTED_EDGE('',*,*,#5748,.F.);
#7924=ORIENTED_EDGE('',*,*,#5749,.F.);
#7925=ORIENTED_EDGE('',*,*,#5747,.F.);
#7926=ORIENTED_EDGE('',*,*,#5750,.F.);
#7927=ORIENTED_EDGE('',*,*,#5751,.F.);
#7928=ORIENTED_EDGE('',*,*,#5716,.F.);
#7929=ORIENTED_EDGE('',*,*,#5697,.T.);
#7930=ORIENTED_EDGE('',*,*,#5752,.T.);
#7931=ORIENTED_EDGE('',*,*,#5719,.T.);
#7932=ORIENTED_EDGE('',*,*,#5703,.F.);
#7933=ORIENTED_EDGE('',*,*,#5753,.F.);
#7934=ORIENTED_EDGE('',*,*,#5754,.F.);
#7935=ORIENTED_EDGE('',*,*,#5755,.F.);
#7936=ORIENTED_EDGE('',*,*,#5721,.T.);
#7937=ORIENTED_EDGE('',*,*,#5752,.F.);
#7938=ORIENTED_EDGE('',*,*,#5756,.F.);
#7939=ORIENTED_EDGE('',*,*,#5755,.T.);
#7940=ORIENTED_EDGE('',*,*,#5734,.T.);
#7941=ORIENTED_EDGE('',*,*,#5667,.T.);
#7942=ORIENTED_EDGE('',*,*,#5730,.T.);
#7943=ORIENTED_EDGE('',*,*,#5695,.T.);
#7944=ORIENTED_EDGE('',*,*,#5757,.T.);
#7945=ORIENTED_EDGE('',*,*,#5758,.T.);
#7946=ORIENTED_EDGE('',*,*,#5759,.T.);
#7947=ORIENTED_EDGE('',*,*,#5760,.T.);
#7948=ORIENTED_EDGE('',*,*,#5761,.T.);
#7949=ORIENTED_EDGE('',*,*,#5762,.T.);
#7950=ORIENTED_EDGE('',*,*,#5763,.T.);
#7951=ORIENTED_EDGE('',*,*,#5764,.T.);
#7952=ORIENTED_EDGE('',*,*,#5750,.T.);
#7953=ORIENTED_EDGE('',*,*,#5756,.T.);
#7954=ORIENTED_EDGE('',*,*,#5754,.T.);
#7955=ORIENTED_EDGE('',*,*,#5765,.T.);
#7956=ORIENTED_EDGE('',*,*,#5766,.T.);
#7957=ORIENTED_EDGE('',*,*,#5767,.T.);
#7958=ORIENTED_EDGE('',*,*,#5768,.T.);
#7959=ORIENTED_EDGE('',*,*,#5769,.T.);
#7960=ORIENTED_EDGE('',*,*,#5753,.T.);
#7961=ORIENTED_EDGE('',*,*,#5706,.T.);
#7962=ORIENTED_EDGE('',*,*,#5724,.F.);
#7963=ORIENTED_EDGE('',*,*,#5708,.F.);
#7964=ORIENTED_EDGE('',*,*,#5770,.T.);
#7965=ORIENTED_EDGE('',*,*,#5765,.F.);
#7966=ORIENTED_EDGE('',*,*,#5654,.T.);
#7967=ORIENTED_EDGE('',*,*,#5741,.T.);
#7968=ORIENTED_EDGE('',*,*,#5651,.F.);
#7969=ORIENTED_EDGE('',*,*,#5739,.T.);
#7970=ORIENTED_EDGE('',*,*,#5740,.T.);
#7971=ORIENTED_EDGE('',*,*,#5671,.T.);
#7972=ORIENTED_EDGE('',*,*,#5737,.T.);
#7973=ORIENTED_EDGE('',*,*,#5649,.F.);
#7974=ORIENTED_EDGE('',*,*,#5771,.F.);
#7975=ORIENTED_EDGE('',*,*,#5771,.T.);
#7976=ORIENTED_EDGE('',*,*,#5772,.T.);
#7977=ORIENTED_EDGE('',*,*,#5773,.T.);
#7978=ORIENTED_EDGE('',*,*,#5772,.F.);
#7979=ORIENTED_EDGE('',*,*,#5773,.F.);
#7980=ORIENTED_EDGE('',*,*,#5774,.F.);
#7981=ORIENTED_EDGE('',*,*,#5774,.T.);
#7982=ORIENTED_EDGE('',*,*,#5775,.T.);
#7983=ORIENTED_EDGE('',*,*,#5776,.F.);
#7984=ORIENTED_EDGE('',*,*,#5777,.F.);
#7985=ORIENTED_EDGE('',*,*,#5778,.F.);
#7986=ORIENTED_EDGE('',*,*,#5779,.F.);
#7987=ORIENTED_EDGE('',*,*,#5775,.F.);
#7988=ORIENTED_EDGE('',*,*,#5767,.F.);
#7989=ORIENTED_EDGE('',*,*,#5780,.T.);
#7990=ORIENTED_EDGE('',*,*,#5742,.T.);
#7991=ORIENTED_EDGE('',*,*,#5656,.T.);
#7992=ORIENTED_EDGE('',*,*,#5738,.T.);
#7993=ORIENTED_EDGE('',*,*,#5681,.T.);
#7994=ORIENTED_EDGE('',*,*,#5768,.F.);
#7995=ORIENTED_EDGE('',*,*,#5780,.F.);
#7996=ORIENTED_EDGE('',*,*,#5766,.F.);
#7997=ORIENTED_EDGE('',*,*,#5770,.F.);
#7998=ORIENTED_EDGE('',*,*,#5707,.F.);
#7999=ORIENTED_EDGE('',*,*,#5711,.F.);
#8000=ORIENTED_EDGE('',*,*,#5726,.F.);
#8001=ORIENTED_EDGE('',*,*,#5700,.F.);
#8002=ORIENTED_EDGE('',*,*,#5713,.F.);
#8003=ORIENTED_EDGE('',*,*,#5781,.F.);
#8004=ORIENTED_EDGE('',*,*,#5751,.T.);
#8005=ORIENTED_EDGE('',*,*,#5769,.F.);
#8006=ORIENTED_EDGE('',*,*,#5781,.T.);
#8007=ORIENTED_EDGE('',*,*,#5715,.T.);
#8008=ORIENTED_EDGE('',*,*,#5722,.F.);
#8009=ORIENTED_EDGE('',*,*,#5717,.F.);
#8010=ORIENTED_EDGE('',*,*,#5761,.F.);
#8011=ORIENTED_EDGE('',*,*,#5782,.T.);
#8012=ORIENTED_EDGE('',*,*,#5783,.F.);
#8013=ORIENTED_EDGE('',*,*,#5782,.F.);
#8014=ORIENTED_EDGE('',*,*,#5762,.F.);
#8015=ORIENTED_EDGE('',*,*,#5784,.T.);
#8016=ORIENTED_EDGE('',*,*,#5785,.F.);
#8017=ORIENTED_EDGE('',*,*,#5784,.F.);
#8018=ORIENTED_EDGE('',*,*,#5763,.F.);
#8019=ORIENTED_EDGE('',*,*,#5786,.T.);
#8020=ORIENTED_EDGE('',*,*,#5787,.F.);
#8021=ORIENTED_EDGE('',*,*,#5786,.F.);
#8022=ORIENTED_EDGE('',*,*,#5764,.F.);
#8023=ORIENTED_EDGE('',*,*,#5788,.T.);
#8024=ORIENTED_EDGE('',*,*,#5789,.F.);
#8025=ORIENTED_EDGE('',*,*,#5788,.F.);
#8026=ORIENTED_EDGE('',*,*,#5725,.F.);
#8027=ORIENTED_EDGE('',*,*,#5790,.T.);
#8028=ORIENTED_EDGE('',*,*,#5776,.T.);
#8029=ORIENTED_EDGE('',*,*,#5779,.T.);
#8030=ORIENTED_EDGE('',*,*,#5791,.T.);
#8031=ORIENTED_EDGE('',*,*,#5792,.F.);
#8032=ORIENTED_EDGE('',*,*,#5791,.F.);
#8033=ORIENTED_EDGE('',*,*,#5778,.T.);
#8034=ORIENTED_EDGE('',*,*,#5777,.T.);
#8035=ORIENTED_EDGE('',*,*,#5790,.F.);
#8036=ORIENTED_EDGE('',*,*,#5748,.T.);
#8037=ORIENTED_EDGE('',*,*,#5749,.T.);
#8038=ORIENTED_EDGE('',*,*,#5793,.T.);
#8039=ORIENTED_EDGE('',*,*,#5794,.T.);
#8040=ORIENTED_EDGE('',*,*,#5760,.F.);
#8041=ORIENTED_EDGE('',*,*,#5795,.F.);
#8042=ORIENTED_EDGE('',*,*,#5796,.T.);
#8043=ORIENTED_EDGE('',*,*,#5795,.T.);
#8044=ORIENTED_EDGE('',*,*,#5759,.F.);
#8045=ORIENTED_EDGE('',*,*,#5797,.F.);
#8046=ORIENTED_EDGE('',*,*,#5798,.T.);
#8047=ORIENTED_EDGE('',*,*,#5797,.T.);
#8048=ORIENTED_EDGE('',*,*,#5758,.F.);
#8049=ORIENTED_EDGE('',*,*,#5799,.F.);
#8050=ORIENTED_EDGE('',*,*,#5800,.T.);
#8051=ORIENTED_EDGE('',*,*,#5799,.T.);
#8052=ORIENTED_EDGE('',*,*,#5757,.F.);
#8053=ORIENTED_EDGE('',*,*,#5794,.F.);
#8054=ORIENTED_EDGE('',*,*,#5800,.F.);
#8055=ORIENTED_EDGE('',*,*,#5793,.F.);
#8056=ORIENTED_EDGE('',*,*,#5796,.F.);
#8057=ORIENTED_EDGE('',*,*,#5798,.F.);
#8058=ORIENTED_EDGE('',*,*,#5792,.T.);
#8059=ORIENTED_EDGE('',*,*,#5789,.T.);
#8060=ORIENTED_EDGE('',*,*,#5787,.T.);
#8061=ORIENTED_EDGE('',*,*,#5785,.T.);
#8062=ORIENTED_EDGE('',*,*,#5783,.T.);
#8063=ORIENTED_EDGE('',*,*,#5801,.T.);
#8064=ORIENTED_EDGE('',*,*,#5802,.F.);
#8065=ORIENTED_EDGE('',*,*,#5801,.F.);
#8066=ORIENTED_EDGE('',*,*,#5803,.T.);
#8067=ORIENTED_EDGE('',*,*,#5804,.T.);
#8068=ORIENTED_EDGE('',*,*,#5803,.F.);
#8069=ORIENTED_EDGE('',*,*,#5804,.F.);
#8070=ORIENTED_EDGE('',*,*,#5805,.F.);
#8071=ORIENTED_EDGE('',*,*,#5806,.F.);
#8072=ORIENTED_EDGE('',*,*,#5807,.T.);
#8073=ORIENTED_EDGE('',*,*,#5805,.T.);
#8074=ORIENTED_EDGE('',*,*,#5807,.F.);
#8075=ORIENTED_EDGE('',*,*,#5808,.F.);
#8076=ORIENTED_EDGE('',*,*,#5809,.T.);
#8077=ORIENTED_EDGE('',*,*,#5802,.T.);
#8078=ORIENTED_EDGE('',*,*,#5809,.F.);
#8079=ORIENTED_EDGE('',*,*,#5808,.T.);
#8080=ORIENTED_EDGE('',*,*,#5806,.T.);
#8081=ORIENTED_EDGE('',*,*,#5810,.T.);
#8082=ORIENTED_EDGE('',*,*,#5811,.T.);
#8083=ORIENTED_EDGE('',*,*,#5812,.T.);
#8084=ORIENTED_EDGE('',*,*,#5813,.T.);
#8085=ORIENTED_EDGE('',*,*,#5814,.T.);
#8086=ORIENTED_EDGE('',*,*,#5815,.T.);
#8087=ORIENTED_EDGE('',*,*,#5814,.F.);
#8088=ORIENTED_EDGE('',*,*,#5816,.T.);
#8089=ORIENTED_EDGE('',*,*,#5817,.T.);
#8090=ORIENTED_EDGE('',*,*,#5818,.T.);
#8091=ORIENTED_EDGE('',*,*,#5810,.F.);
#8092=ORIENTED_EDGE('',*,*,#5819,.T.);
#8093=ORIENTED_EDGE('',*,*,#5820,.T.);
#8094=ORIENTED_EDGE('',*,*,#5821,.T.);
#8095=ORIENTED_EDGE('',*,*,#5817,.F.);
#8096=ORIENTED_EDGE('',*,*,#5822,.T.);
#8097=ORIENTED_EDGE('',*,*,#5823,.T.);
#8098=ORIENTED_EDGE('',*,*,#5824,.T.);
#8099=ORIENTED_EDGE('',*,*,#5820,.F.);
#8100=ORIENTED_EDGE('',*,*,#5825,.T.);
#8101=ORIENTED_EDGE('',*,*,#5826,.T.);
#8102=ORIENTED_EDGE('',*,*,#5827,.T.);
#8103=ORIENTED_EDGE('',*,*,#5823,.F.);
#8104=ORIENTED_EDGE('',*,*,#5828,.T.);
#8105=ORIENTED_EDGE('',*,*,#5829,.T.);
#8106=ORIENTED_EDGE('',*,*,#5830,.T.);
#8107=ORIENTED_EDGE('',*,*,#5826,.F.);
#8108=ORIENTED_EDGE('',*,*,#5831,.T.);
#8109=ORIENTED_EDGE('',*,*,#5832,.T.);
#8110=ORIENTED_EDGE('',*,*,#5833,.T.);
#8111=ORIENTED_EDGE('',*,*,#5829,.F.);
#8112=ORIENTED_EDGE('',*,*,#5834,.T.);
#8113=ORIENTED_EDGE('',*,*,#5835,.T.);
#8114=ORIENTED_EDGE('',*,*,#5836,.T.);
#8115=ORIENTED_EDGE('',*,*,#5832,.F.);
#8116=ORIENTED_EDGE('',*,*,#5837,.T.);
#8117=ORIENTED_EDGE('',*,*,#5838,.T.);
#8118=ORIENTED_EDGE('',*,*,#5839,.T.);
#8119=ORIENTED_EDGE('',*,*,#5835,.F.);
#8120=ORIENTED_EDGE('',*,*,#5840,.T.);
#8121=ORIENTED_EDGE('',*,*,#5841,.T.);
#8122=ORIENTED_EDGE('',*,*,#5842,.T.);
#8123=ORIENTED_EDGE('',*,*,#5838,.F.);
#8124=ORIENTED_EDGE('',*,*,#5843,.T.);
#8125=ORIENTED_EDGE('',*,*,#5844,.T.);
#8126=ORIENTED_EDGE('',*,*,#5845,.T.);
#8127=ORIENTED_EDGE('',*,*,#5841,.F.);
#8128=ORIENTED_EDGE('',*,*,#5846,.T.);
#8129=ORIENTED_EDGE('',*,*,#5847,.F.);
#8130=ORIENTED_EDGE('',*,*,#5848,.T.);
#8131=ORIENTED_EDGE('',*,*,#5849,.F.);
#8132=ORIENTED_EDGE('',*,*,#5850,.T.);
#8133=ORIENTED_EDGE('',*,*,#5851,.T.);
#8134=ORIENTED_EDGE('',*,*,#5852,.T.);
#8135=ORIENTED_EDGE('',*,*,#5853,.F.);
#8136=ORIENTED_EDGE('',*,*,#5854,.F.);
#8137=ORIENTED_EDGE('',*,*,#5855,.T.);
#8138=ORIENTED_EDGE('',*,*,#5856,.T.);
#8139=ORIENTED_EDGE('',*,*,#5851,.F.);
#8140=ORIENTED_EDGE('',*,*,#5857,.F.);
#8141=ORIENTED_EDGE('',*,*,#5858,.T.);
#8142=ORIENTED_EDGE('',*,*,#5859,.T.);
#8143=ORIENTED_EDGE('',*,*,#5855,.F.);
#8144=ORIENTED_EDGE('',*,*,#5860,.F.);
#8145=ORIENTED_EDGE('',*,*,#5861,.T.);
#8146=ORIENTED_EDGE('',*,*,#5862,.T.);
#8147=ORIENTED_EDGE('',*,*,#5858,.F.);
#8148=ORIENTED_EDGE('',*,*,#5863,.F.);
#8149=ORIENTED_EDGE('',*,*,#5864,.T.);
#8150=ORIENTED_EDGE('',*,*,#5865,.T.);
#8151=ORIENTED_EDGE('',*,*,#5861,.F.);
#8152=ORIENTED_EDGE('',*,*,#5866,.F.);
#8153=ORIENTED_EDGE('',*,*,#5867,.T.);
#8154=ORIENTED_EDGE('',*,*,#5868,.T.);
#8155=ORIENTED_EDGE('',*,*,#5864,.F.);
#8156=ORIENTED_EDGE('',*,*,#5869,.F.);
#8157=ORIENTED_EDGE('',*,*,#5870,.T.);
#8158=ORIENTED_EDGE('',*,*,#5871,.T.);
#8159=ORIENTED_EDGE('',*,*,#5867,.F.);
#8160=ORIENTED_EDGE('',*,*,#5872,.F.);
#8161=ORIENTED_EDGE('',*,*,#5873,.T.);
#8162=ORIENTED_EDGE('',*,*,#5874,.T.);
#8163=ORIENTED_EDGE('',*,*,#5870,.F.);
#8164=ORIENTED_EDGE('',*,*,#5875,.F.);
#8165=ORIENTED_EDGE('',*,*,#5876,.T.);
#8166=ORIENTED_EDGE('',*,*,#5877,.T.);
#8167=ORIENTED_EDGE('',*,*,#5873,.F.);
#8168=ORIENTED_EDGE('',*,*,#5878,.F.);
#8169=ORIENTED_EDGE('',*,*,#5879,.T.);
#8170=ORIENTED_EDGE('',*,*,#5880,.T.);
#8171=ORIENTED_EDGE('',*,*,#5876,.F.);
#8172=ORIENTED_EDGE('',*,*,#5881,.F.);
#8173=ORIENTED_EDGE('',*,*,#5882,.T.);
#8174=ORIENTED_EDGE('',*,*,#5883,.T.);
#8175=ORIENTED_EDGE('',*,*,#5879,.F.);
#8176=ORIENTED_EDGE('',*,*,#5884,.F.);
#8177=ORIENTED_EDGE('',*,*,#5885,.T.);
#8178=ORIENTED_EDGE('',*,*,#5886,.T.);
#8179=ORIENTED_EDGE('',*,*,#5882,.F.);
#8180=ORIENTED_EDGE('',*,*,#5887,.F.);
#8181=ORIENTED_EDGE('',*,*,#5888,.F.);
#8182=ORIENTED_EDGE('',*,*,#5889,.F.);
#8183=ORIENTED_EDGE('',*,*,#5890,.F.);
#8184=ORIENTED_EDGE('',*,*,#5891,.T.);
#8185=ORIENTED_EDGE('',*,*,#5892,.T.);
#8186=ORIENTED_EDGE('',*,*,#5893,.T.);
#8187=ORIENTED_EDGE('',*,*,#5894,.F.);
#8188=ORIENTED_EDGE('',*,*,#5895,.T.);
#8189=ORIENTED_EDGE('',*,*,#5896,.T.);
#8190=ORIENTED_EDGE('',*,*,#5897,.T.);
#8191=ORIENTED_EDGE('',*,*,#5892,.F.);
#8192=ORIENTED_EDGE('',*,*,#5898,.T.);
#8193=ORIENTED_EDGE('',*,*,#5899,.T.);
#8194=ORIENTED_EDGE('',*,*,#5900,.T.);
#8195=ORIENTED_EDGE('',*,*,#5896,.F.);
#8196=ORIENTED_EDGE('',*,*,#5901,.T.);
#8197=ORIENTED_EDGE('',*,*,#5902,.T.);
#8198=ORIENTED_EDGE('',*,*,#5903,.T.);
#8199=ORIENTED_EDGE('',*,*,#5899,.F.);
#8200=ORIENTED_EDGE('',*,*,#5904,.T.);
#8201=ORIENTED_EDGE('',*,*,#5905,.T.);
#8202=ORIENTED_EDGE('',*,*,#5906,.T.);
#8203=ORIENTED_EDGE('',*,*,#5902,.F.);
#8204=ORIENTED_EDGE('',*,*,#5907,.T.);
#8205=ORIENTED_EDGE('',*,*,#5908,.T.);
#8206=ORIENTED_EDGE('',*,*,#5909,.T.);
#8207=ORIENTED_EDGE('',*,*,#5905,.F.);
#8208=ORIENTED_EDGE('',*,*,#5910,.T.);
#8209=ORIENTED_EDGE('',*,*,#5911,.T.);
#8210=ORIENTED_EDGE('',*,*,#5912,.T.);
#8211=ORIENTED_EDGE('',*,*,#5908,.F.);
#8212=ORIENTED_EDGE('',*,*,#5913,.T.);
#8213=ORIENTED_EDGE('',*,*,#5914,.F.);
#8214=ORIENTED_EDGE('',*,*,#5915,.T.);
#8215=ORIENTED_EDGE('',*,*,#5916,.F.);
#8216=ORIENTED_EDGE('',*,*,#5917,.T.);
#8217=ORIENTED_EDGE('',*,*,#5918,.T.);
#8218=ORIENTED_EDGE('',*,*,#5919,.T.);
#8219=ORIENTED_EDGE('',*,*,#5920,.F.);
#8220=ORIENTED_EDGE('',*,*,#5921,.T.);
#8221=ORIENTED_EDGE('',*,*,#5922,.T.);
#8222=ORIENTED_EDGE('',*,*,#5923,.T.);
#8223=ORIENTED_EDGE('',*,*,#5918,.F.);
#8224=ORIENTED_EDGE('',*,*,#5924,.T.);
#8225=ORIENTED_EDGE('',*,*,#5925,.T.);
#8226=ORIENTED_EDGE('',*,*,#5926,.T.);
#8227=ORIENTED_EDGE('',*,*,#5922,.F.);
#8228=ORIENTED_EDGE('',*,*,#5927,.T.);
#8229=ORIENTED_EDGE('',*,*,#5928,.T.);
#8230=ORIENTED_EDGE('',*,*,#5929,.T.);
#8231=ORIENTED_EDGE('',*,*,#5925,.F.);
#8232=ORIENTED_EDGE('',*,*,#5930,.T.);
#8233=ORIENTED_EDGE('',*,*,#5931,.T.);
#8234=ORIENTED_EDGE('',*,*,#5932,.T.);
#8235=ORIENTED_EDGE('',*,*,#5928,.F.);
#8236=ORIENTED_EDGE('',*,*,#5933,.T.);
#8237=ORIENTED_EDGE('',*,*,#5934,.T.);
#8238=ORIENTED_EDGE('',*,*,#5935,.T.);
#8239=ORIENTED_EDGE('',*,*,#5931,.F.);
#8240=ORIENTED_EDGE('',*,*,#5936,.T.);
#8241=ORIENTED_EDGE('',*,*,#5937,.T.);
#8242=ORIENTED_EDGE('',*,*,#5938,.T.);
#8243=ORIENTED_EDGE('',*,*,#5934,.F.);
#8244=ORIENTED_EDGE('',*,*,#5939,.T.);
#8245=ORIENTED_EDGE('',*,*,#5940,.F.);
#8246=ORIENTED_EDGE('',*,*,#5941,.T.);
#8247=ORIENTED_EDGE('',*,*,#5942,.F.);
#8248=ORIENTED_EDGE('',*,*,#5943,.T.);
#8249=ORIENTED_EDGE('',*,*,#5944,.T.);
#8250=ORIENTED_EDGE('',*,*,#5945,.T.);
#8251=ORIENTED_EDGE('',*,*,#5946,.F.);
#8252=ORIENTED_EDGE('',*,*,#5947,.F.);
#8253=ORIENTED_EDGE('',*,*,#5948,.T.);
#8254=ORIENTED_EDGE('',*,*,#5949,.T.);
#8255=ORIENTED_EDGE('',*,*,#5944,.F.);
#8256=ORIENTED_EDGE('',*,*,#5950,.F.);
#8257=ORIENTED_EDGE('',*,*,#5951,.T.);
#8258=ORIENTED_EDGE('',*,*,#5952,.T.);
#8259=ORIENTED_EDGE('',*,*,#5948,.F.);
#8260=ORIENTED_EDGE('',*,*,#5953,.F.);
#8261=ORIENTED_EDGE('',*,*,#5954,.T.);
#8262=ORIENTED_EDGE('',*,*,#5955,.T.);
#8263=ORIENTED_EDGE('',*,*,#5951,.F.);
#8264=ORIENTED_EDGE('',*,*,#5956,.F.);
#8265=ORIENTED_EDGE('',*,*,#5957,.T.);
#8266=ORIENTED_EDGE('',*,*,#5958,.T.);
#8267=ORIENTED_EDGE('',*,*,#5954,.F.);
#8268=ORIENTED_EDGE('',*,*,#5959,.F.);
#8269=ORIENTED_EDGE('',*,*,#5960,.T.);
#8270=ORIENTED_EDGE('',*,*,#5961,.T.);
#8271=ORIENTED_EDGE('',*,*,#5957,.F.);
#8272=ORIENTED_EDGE('',*,*,#5962,.F.);
#8273=ORIENTED_EDGE('',*,*,#5963,.T.);
#8274=ORIENTED_EDGE('',*,*,#5964,.T.);
#8275=ORIENTED_EDGE('',*,*,#5960,.F.);
#8276=ORIENTED_EDGE('',*,*,#5965,.F.);
#8277=ORIENTED_EDGE('',*,*,#5966,.F.);
#8278=ORIENTED_EDGE('',*,*,#5967,.F.);
#8279=ORIENTED_EDGE('',*,*,#5968,.F.);
#8280=ORIENTED_EDGE('',*,*,#5969,.T.);
#8281=ORIENTED_EDGE('',*,*,#5970,.T.);
#8282=ORIENTED_EDGE('',*,*,#5971,.T.);
#8283=ORIENTED_EDGE('',*,*,#5972,.F.);
#8284=ORIENTED_EDGE('',*,*,#5973,.F.);
#8285=ORIENTED_EDGE('',*,*,#5974,.T.);
#8286=ORIENTED_EDGE('',*,*,#5975,.T.);
#8287=ORIENTED_EDGE('',*,*,#5970,.F.);
#8288=ORIENTED_EDGE('',*,*,#5976,.F.);
#8289=ORIENTED_EDGE('',*,*,#5977,.T.);
#8290=ORIENTED_EDGE('',*,*,#5978,.T.);
#8291=ORIENTED_EDGE('',*,*,#5974,.F.);
#8292=ORIENTED_EDGE('',*,*,#5979,.F.);
#8293=ORIENTED_EDGE('',*,*,#5980,.T.);
#8294=ORIENTED_EDGE('',*,*,#5981,.T.);
#8295=ORIENTED_EDGE('',*,*,#5977,.F.);
#8296=ORIENTED_EDGE('',*,*,#5982,.F.);
#8297=ORIENTED_EDGE('',*,*,#5983,.T.);
#8298=ORIENTED_EDGE('',*,*,#5984,.T.);
#8299=ORIENTED_EDGE('',*,*,#5980,.F.);
#8300=ORIENTED_EDGE('',*,*,#5985,.F.);
#8301=ORIENTED_EDGE('',*,*,#5986,.T.);
#8302=ORIENTED_EDGE('',*,*,#5987,.T.);
#8303=ORIENTED_EDGE('',*,*,#5983,.F.);
#8304=ORIENTED_EDGE('',*,*,#5988,.F.);
#8305=ORIENTED_EDGE('',*,*,#5989,.T.);
#8306=ORIENTED_EDGE('',*,*,#5990,.T.);
#8307=ORIENTED_EDGE('',*,*,#5986,.F.);
#8308=ORIENTED_EDGE('',*,*,#5991,.F.);
#8309=ORIENTED_EDGE('',*,*,#5992,.F.);
#8310=ORIENTED_EDGE('',*,*,#5993,.F.);
#8311=ORIENTED_EDGE('',*,*,#5994,.F.);
#8312=ORIENTED_EDGE('',*,*,#5995,.T.);
#8313=ORIENTED_EDGE('',*,*,#5992,.T.);
#8314=ORIENTED_EDGE('',*,*,#5996,.T.);
#8315=ORIENTED_EDGE('',*,*,#5989,.F.);
#8316=ORIENTED_EDGE('',*,*,#5997,.F.);
#8317=ORIENTED_EDGE('',*,*,#5998,.F.);
#8318=ORIENTED_EDGE('',*,*,#5971,.F.);
#8319=ORIENTED_EDGE('',*,*,#5975,.F.);
#8320=ORIENTED_EDGE('',*,*,#5978,.F.);
#8321=ORIENTED_EDGE('',*,*,#5981,.F.);
#8322=ORIENTED_EDGE('',*,*,#5984,.F.);
#8323=ORIENTED_EDGE('',*,*,#5987,.F.);
#8324=ORIENTED_EDGE('',*,*,#5990,.F.);
#8325=ORIENTED_EDGE('',*,*,#5996,.F.);
#8326=ORIENTED_EDGE('',*,*,#5995,.F.);
#8327=ORIENTED_EDGE('',*,*,#5999,.F.);
#8328=ORIENTED_EDGE('',*,*,#5941,.F.);
#8329=ORIENTED_EDGE('',*,*,#6000,.F.);
#8330=ORIENTED_EDGE('',*,*,#5939,.F.);
#8331=ORIENTED_EDGE('',*,*,#5936,.F.);
#8332=ORIENTED_EDGE('',*,*,#5933,.F.);
#8333=ORIENTED_EDGE('',*,*,#5930,.F.);
#8334=ORIENTED_EDGE('',*,*,#5927,.F.);
#8335=ORIENTED_EDGE('',*,*,#5924,.F.);
#8336=ORIENTED_EDGE('',*,*,#5921,.F.);
#8337=ORIENTED_EDGE('',*,*,#6001,.F.);
#8338=ORIENTED_EDGE('',*,*,#5919,.F.);
#8339=ORIENTED_EDGE('',*,*,#5923,.F.);
#8340=ORIENTED_EDGE('',*,*,#5926,.F.);
#8341=ORIENTED_EDGE('',*,*,#5929,.F.);
#8342=ORIENTED_EDGE('',*,*,#5932,.F.);
#8343=ORIENTED_EDGE('',*,*,#5935,.F.);
#8344=ORIENTED_EDGE('',*,*,#5938,.F.);
#8345=ORIENTED_EDGE('',*,*,#6002,.F.);
#8346=ORIENTED_EDGE('',*,*,#5943,.F.);
#8347=ORIENTED_EDGE('',*,*,#6003,.F.);
#8348=ORIENTED_EDGE('',*,*,#5993,.T.);
#8349=ORIENTED_EDGE('',*,*,#5997,.T.);
#8350=ORIENTED_EDGE('',*,*,#5991,.T.);
#8351=ORIENTED_EDGE('',*,*,#5988,.T.);
#8352=ORIENTED_EDGE('',*,*,#5985,.T.);
#8353=ORIENTED_EDGE('',*,*,#5982,.T.);
#8354=ORIENTED_EDGE('',*,*,#5979,.T.);
#8355=ORIENTED_EDGE('',*,*,#5976,.T.);
#8356=ORIENTED_EDGE('',*,*,#5973,.T.);
#8357=ORIENTED_EDGE('',*,*,#6004,.F.);
#8358=ORIENTED_EDGE('',*,*,#6005,.F.);
#8359=ORIENTED_EDGE('',*,*,#6006,.F.);
#8360=ORIENTED_EDGE('',*,*,#6007,.F.);
#8361=ORIENTED_EDGE('',*,*,#6008,.F.);
#8362=ORIENTED_EDGE('',*,*,#6009,.F.);
#8363=ORIENTED_EDGE('',*,*,#6001,.T.);
#8364=ORIENTED_EDGE('',*,*,#5972,.T.);
#8365=ORIENTED_EDGE('',*,*,#5998,.T.);
#8366=ORIENTED_EDGE('',*,*,#5920,.T.);
#8367=ORIENTED_EDGE('',*,*,#6010,.T.);
#8368=ORIENTED_EDGE('',*,*,#5946,.T.);
#8369=ORIENTED_EDGE('',*,*,#6011,.T.);
#8370=ORIENTED_EDGE('',*,*,#5894,.T.);
#8371=ORIENTED_EDGE('',*,*,#5966,.T.);
#8372=ORIENTED_EDGE('',*,*,#6012,.T.);
#8373=ORIENTED_EDGE('',*,*,#5963,.F.);
#8374=ORIENTED_EDGE('',*,*,#6013,.F.);
#8375=ORIENTED_EDGE('',*,*,#6011,.F.);
#8376=ORIENTED_EDGE('',*,*,#5945,.F.);
#8377=ORIENTED_EDGE('',*,*,#5949,.F.);
#8378=ORIENTED_EDGE('',*,*,#5952,.F.);
#8379=ORIENTED_EDGE('',*,*,#5955,.F.);
#8380=ORIENTED_EDGE('',*,*,#5958,.F.);
#8381=ORIENTED_EDGE('',*,*,#5961,.F.);
#8382=ORIENTED_EDGE('',*,*,#5964,.F.);
#8383=ORIENTED_EDGE('',*,*,#6012,.F.);
#8384=ORIENTED_EDGE('',*,*,#5969,.F.);
#8385=ORIENTED_EDGE('',*,*,#6014,.F.);
#8386=ORIENTED_EDGE('',*,*,#5915,.F.);
#8387=ORIENTED_EDGE('',*,*,#6015,.F.);
#8388=ORIENTED_EDGE('',*,*,#5913,.F.);
#8389=ORIENTED_EDGE('',*,*,#5910,.F.);
#8390=ORIENTED_EDGE('',*,*,#5907,.F.);
#8391=ORIENTED_EDGE('',*,*,#5904,.F.);
#8392=ORIENTED_EDGE('',*,*,#5901,.F.);
#8393=ORIENTED_EDGE('',*,*,#5898,.F.);
#8394=ORIENTED_EDGE('',*,*,#5895,.F.);
#8395=ORIENTED_EDGE('',*,*,#6010,.F.);
#8396=ORIENTED_EDGE('',*,*,#5893,.F.);
#8397=ORIENTED_EDGE('',*,*,#5897,.F.);
#8398=ORIENTED_EDGE('',*,*,#5900,.F.);
#8399=ORIENTED_EDGE('',*,*,#5903,.F.);
#8400=ORIENTED_EDGE('',*,*,#5906,.F.);
#8401=ORIENTED_EDGE('',*,*,#5909,.F.);
#8402=ORIENTED_EDGE('',*,*,#5912,.F.);
#8403=ORIENTED_EDGE('',*,*,#6016,.F.);
#8404=ORIENTED_EDGE('',*,*,#5917,.F.);
#8405=ORIENTED_EDGE('',*,*,#6017,.F.);
#8406=ORIENTED_EDGE('',*,*,#5967,.T.);
#8407=ORIENTED_EDGE('',*,*,#6013,.T.);
#8408=ORIENTED_EDGE('',*,*,#5965,.T.);
#8409=ORIENTED_EDGE('',*,*,#5962,.T.);
#8410=ORIENTED_EDGE('',*,*,#5959,.T.);
#8411=ORIENTED_EDGE('',*,*,#5956,.T.);
#8412=ORIENTED_EDGE('',*,*,#5953,.T.);
#8413=ORIENTED_EDGE('',*,*,#5950,.T.);
#8414=ORIENTED_EDGE('',*,*,#5947,.T.);
#8415=ORIENTED_EDGE('',*,*,#5940,.T.);
#8416=ORIENTED_EDGE('',*,*,#6002,.T.);
#8417=ORIENTED_EDGE('',*,*,#5937,.F.);
#8418=ORIENTED_EDGE('',*,*,#6000,.T.);
#8419=ORIENTED_EDGE('',*,*,#5914,.T.);
#8420=ORIENTED_EDGE('',*,*,#6016,.T.);
#8421=ORIENTED_EDGE('',*,*,#5911,.F.);
#8422=ORIENTED_EDGE('',*,*,#6015,.T.);
#8423=ORIENTED_EDGE('',*,*,#5812,.F.);
#8424=ORIENTED_EDGE('',*,*,#6018,.T.);
#8425=ORIENTED_EDGE('',*,*,#5853,.T.);
#8426=ORIENTED_EDGE('',*,*,#6019,.T.);
#8427=ORIENTED_EDGE('',*,*,#5888,.T.);
#8428=ORIENTED_EDGE('',*,*,#6020,.T.);
#8429=ORIENTED_EDGE('',*,*,#5885,.F.);
#8430=ORIENTED_EDGE('',*,*,#6021,.F.);
#8431=ORIENTED_EDGE('',*,*,#6019,.F.);
#8432=ORIENTED_EDGE('',*,*,#5852,.F.);
#8433=ORIENTED_EDGE('',*,*,#5856,.F.);
#8434=ORIENTED_EDGE('',*,*,#5859,.F.);
#8435=ORIENTED_EDGE('',*,*,#5862,.F.);
#8436=ORIENTED_EDGE('',*,*,#5865,.F.);
#8437=ORIENTED_EDGE('',*,*,#5868,.F.);
#8438=ORIENTED_EDGE('',*,*,#5871,.F.);
#8439=ORIENTED_EDGE('',*,*,#5874,.F.);
#8440=ORIENTED_EDGE('',*,*,#5877,.F.);
#8441=ORIENTED_EDGE('',*,*,#5880,.F.);
#8442=ORIENTED_EDGE('',*,*,#5883,.F.);
#8443=ORIENTED_EDGE('',*,*,#5886,.F.);
#8444=ORIENTED_EDGE('',*,*,#6020,.F.);
#8445=ORIENTED_EDGE('',*,*,#5891,.F.);
#8446=ORIENTED_EDGE('',*,*,#6022,.F.);
#8447=ORIENTED_EDGE('',*,*,#5848,.F.);
#8448=ORIENTED_EDGE('',*,*,#6023,.F.);
#8449=ORIENTED_EDGE('',*,*,#5846,.F.);
#8450=ORIENTED_EDGE('',*,*,#5843,.F.);
#8451=ORIENTED_EDGE('',*,*,#5840,.F.);
#8452=ORIENTED_EDGE('',*,*,#5837,.F.);
#8453=ORIENTED_EDGE('',*,*,#5834,.F.);
#8454=ORIENTED_EDGE('',*,*,#5831,.F.);
#8455=ORIENTED_EDGE('',*,*,#5828,.F.);
#8456=ORIENTED_EDGE('',*,*,#5825,.F.);
#8457=ORIENTED_EDGE('',*,*,#5822,.F.);
#8458=ORIENTED_EDGE('',*,*,#5819,.F.);
#8459=ORIENTED_EDGE('',*,*,#5816,.F.);
#8460=ORIENTED_EDGE('',*,*,#5813,.F.);
#8461=ORIENTED_EDGE('',*,*,#6018,.F.);
#8462=ORIENTED_EDGE('',*,*,#5811,.F.);
#8463=ORIENTED_EDGE('',*,*,#5818,.F.);
#8464=ORIENTED_EDGE('',*,*,#5821,.F.);
#8465=ORIENTED_EDGE('',*,*,#5824,.F.);
#8466=ORIENTED_EDGE('',*,*,#5827,.F.);
#8467=ORIENTED_EDGE('',*,*,#5830,.F.);
#8468=ORIENTED_EDGE('',*,*,#5833,.F.);
#8469=ORIENTED_EDGE('',*,*,#5836,.F.);
#8470=ORIENTED_EDGE('',*,*,#5839,.F.);
#8471=ORIENTED_EDGE('',*,*,#5842,.F.);
#8472=ORIENTED_EDGE('',*,*,#5845,.F.);
#8473=ORIENTED_EDGE('',*,*,#6024,.F.);
#8474=ORIENTED_EDGE('',*,*,#5850,.F.);
#8475=ORIENTED_EDGE('',*,*,#6025,.F.);
#8476=ORIENTED_EDGE('',*,*,#5889,.T.);
#8477=ORIENTED_EDGE('',*,*,#6021,.T.);
#8478=ORIENTED_EDGE('',*,*,#5887,.T.);
#8479=ORIENTED_EDGE('',*,*,#5884,.T.);
#8480=ORIENTED_EDGE('',*,*,#5881,.T.);
#8481=ORIENTED_EDGE('',*,*,#5878,.T.);
#8482=ORIENTED_EDGE('',*,*,#5875,.T.);
#8483=ORIENTED_EDGE('',*,*,#5872,.T.);
#8484=ORIENTED_EDGE('',*,*,#5869,.T.);
#8485=ORIENTED_EDGE('',*,*,#5866,.T.);
#8486=ORIENTED_EDGE('',*,*,#5863,.T.);
#8487=ORIENTED_EDGE('',*,*,#5860,.T.);
#8488=ORIENTED_EDGE('',*,*,#5857,.T.);
#8489=ORIENTED_EDGE('',*,*,#5854,.T.);
#8490=ORIENTED_EDGE('',*,*,#5847,.T.);
#8491=ORIENTED_EDGE('',*,*,#6024,.T.);
#8492=ORIENTED_EDGE('',*,*,#5844,.F.);
#8493=ORIENTED_EDGE('',*,*,#6023,.T.);
#8494=ORIENTED_EDGE('',*,*,#5815,.F.);
#8495=ORIENTED_EDGE('',*,*,#6026,.F.);
#8496=ORIENTED_EDGE('',*,*,#6027,.T.);
#8497=ORIENTED_EDGE('',*,*,#6028,.F.);
#8498=ORIENTED_EDGE('',*,*,#6027,.F.);
#8499=ORIENTED_EDGE('',*,*,#6028,.T.);
#8500=ORIENTED_EDGE('',*,*,#6029,.T.);
#8501=ORIENTED_EDGE('',*,*,#6030,.T.);
#8502=ORIENTED_EDGE('',*,*,#6029,.F.);
#8503=ORIENTED_EDGE('',*,*,#6030,.F.);
#8504=ORIENTED_EDGE('',*,*,#6031,.T.);
#8505=ORIENTED_EDGE('',*,*,#6032,.F.);
#8506=ORIENTED_EDGE('',*,*,#6031,.F.);
#8507=ORIENTED_EDGE('',*,*,#6032,.T.);
#8508=ORIENTED_EDGE('',*,*,#6033,.T.);
#8509=ORIENTED_EDGE('',*,*,#6034,.F.);
#8510=ORIENTED_EDGE('',*,*,#6033,.F.);
#8511=ORIENTED_EDGE('',*,*,#6035,.T.);
#8512=ORIENTED_EDGE('',*,*,#6036,.F.);
#8513=ORIENTED_EDGE('',*,*,#6037,.F.);
#8514=ORIENTED_EDGE('',*,*,#6038,.F.);
#8515=ORIENTED_EDGE('',*,*,#6035,.F.);
#8516=ORIENTED_EDGE('',*,*,#6039,.T.);
#8517=ORIENTED_EDGE('',*,*,#6037,.T.);
#8518=ORIENTED_EDGE('',*,*,#6039,.F.);
#8519=ORIENTED_EDGE('',*,*,#6038,.T.);
#8520=ORIENTED_EDGE('',*,*,#6040,.T.);
#8521=ORIENTED_EDGE('',*,*,#6026,.T.);
#8522=ORIENTED_EDGE('',*,*,#6040,.F.);
#8523=ORIENTED_EDGE('',*,*,#6041,.F.);
#8524=ORIENTED_EDGE('',*,*,#6009,.T.);
#8525=ORIENTED_EDGE('',*,*,#6042,.T.);
#8526=ORIENTED_EDGE('',*,*,#6043,.F.);
#8527=ORIENTED_EDGE('',*,*,#6007,.T.);
#8528=ORIENTED_EDGE('',*,*,#6044,.T.);
#8529=ORIENTED_EDGE('',*,*,#6045,.F.);
#8530=ORIENTED_EDGE('',*,*,#6046,.F.);
#8531=ORIENTED_EDGE('',*,*,#6008,.T.);
#8532=ORIENTED_EDGE('',*,*,#6046,.T.);
#8533=ORIENTED_EDGE('',*,*,#6047,.F.);
#8534=ORIENTED_EDGE('',*,*,#6042,.F.);
#8535=ORIENTED_EDGE('',*,*,#6048,.F.);
#8536=ORIENTED_EDGE('',*,*,#6049,.F.);
#8537=ORIENTED_EDGE('',*,*,#6050,.F.);
#8538=ORIENTED_EDGE('',*,*,#6005,.T.);
#8539=ORIENTED_EDGE('',*,*,#6006,.T.);
#8540=ORIENTED_EDGE('',*,*,#6050,.T.);
#8541=ORIENTED_EDGE('',*,*,#6051,.F.);
#8542=ORIENTED_EDGE('',*,*,#6044,.F.);
#8543=ORIENTED_EDGE('',*,*,#6048,.T.);
#8544=ORIENTED_EDGE('',*,*,#6004,.T.);
#8545=ORIENTED_EDGE('',*,*,#6041,.T.);
#8546=ORIENTED_EDGE('',*,*,#6052,.F.);
#8547=ORIENTED_EDGE('',*,*,#6053,.F.);
#8548=ORIENTED_EDGE('',*,*,#6054,.T.);
#8549=ORIENTED_EDGE('',*,*,#6036,.T.);
#8550=ORIENTED_EDGE('',*,*,#6054,.F.);
#8551=ORIENTED_EDGE('',*,*,#6053,.T.);
#8552=ORIENTED_EDGE('',*,*,#6025,.T.);
#8553=ORIENTED_EDGE('',*,*,#5849,.T.);
#8554=ORIENTED_EDGE('',*,*,#6022,.T.);
#8555=ORIENTED_EDGE('',*,*,#5890,.T.);
#8556=ORIENTED_EDGE('',*,*,#6052,.T.);
#8557=ORIENTED_EDGE('',*,*,#6043,.T.);
#8558=ORIENTED_EDGE('',*,*,#6047,.T.);
#8559=ORIENTED_EDGE('',*,*,#6045,.T.);
#8560=ORIENTED_EDGE('',*,*,#6051,.T.);
#8561=ORIENTED_EDGE('',*,*,#6049,.T.);
#8562=ORIENTED_EDGE('',*,*,#6003,.T.);
#8563=ORIENTED_EDGE('',*,*,#5942,.T.);
#8564=ORIENTED_EDGE('',*,*,#5999,.T.);
#8565=ORIENTED_EDGE('',*,*,#5994,.T.);
#8566=ORIENTED_EDGE('',*,*,#6017,.T.);
#8567=ORIENTED_EDGE('',*,*,#5916,.T.);
#8568=ORIENTED_EDGE('',*,*,#6014,.T.);
#8569=ORIENTED_EDGE('',*,*,#5968,.T.);
#8570=ORIENTED_EDGE('',*,*,#6034,.T.);
#8571=ORIENTED_EDGE('',*,*,#6055,.T.);
#8572=ORIENTED_EDGE('',*,*,#6056,.T.);
#8573=ORIENTED_EDGE('',*,*,#6057,.T.);
#8574=ORIENTED_EDGE('',*,*,#6056,.F.);
#8575=ORIENTED_EDGE('',*,*,#6057,.F.);
#8576=ORIENTED_EDGE('',*,*,#6058,.T.);
#8577=ORIENTED_EDGE('',*,*,#6059,.F.);
#8578=ORIENTED_EDGE('',*,*,#6058,.F.);
#8579=ORIENTED_EDGE('',*,*,#6055,.F.);
#8580=ORIENTED_EDGE('',*,*,#6060,.T.);
#8581=ORIENTED_EDGE('',*,*,#6059,.T.);
#8582=ORIENTED_EDGE('',*,*,#6061,.T.);
#8583=ORIENTED_EDGE('',*,*,#6062,.T.);
#8584=ORIENTED_EDGE('',*,*,#6061,.F.);
#8585=ORIENTED_EDGE('',*,*,#6062,.F.);
#8586=ORIENTED_EDGE('',*,*,#6063,.T.);
#8587=ORIENTED_EDGE('',*,*,#6064,.F.);
#8588=ORIENTED_EDGE('',*,*,#6065,.F.);
#8589=ORIENTED_EDGE('',*,*,#6060,.F.);
#8590=ORIENTED_EDGE('',*,*,#6066,.T.);
#8591=ORIENTED_EDGE('',*,*,#6064,.T.);
#8592=ORIENTED_EDGE('',*,*,#6066,.F.);
#8593=ORIENTED_EDGE('',*,*,#6067,.T.);
#8594=ORIENTED_EDGE('',*,*,#6068,.F.);
#8595=ORIENTED_EDGE('',*,*,#6065,.T.);
#8596=ORIENTED_EDGE('',*,*,#6069,.T.);
#8597=ORIENTED_EDGE('',*,*,#6068,.T.);
#8598=ORIENTED_EDGE('',*,*,#6069,.F.);
#8599=ORIENTED_EDGE('',*,*,#6067,.F.);
#8600=ORIENTED_EDGE('',*,*,#6070,.T.);
#8601=ORIENTED_EDGE('',*,*,#6071,.T.);
#8602=ORIENTED_EDGE('',*,*,#6070,.F.);
#8603=ORIENTED_EDGE('',*,*,#6063,.F.);
#8604=ORIENTED_EDGE('',*,*,#6072,.T.);
#8605=ORIENTED_EDGE('',*,*,#6073,.T.);
#8606=ORIENTED_EDGE('',*,*,#6072,.F.);
#8607=ORIENTED_EDGE('',*,*,#6073,.F.);
#8608=ORIENTED_EDGE('',*,*,#6071,.F.);
#8609=ORIENTED_EDGE('',*,*,#6074,.F.);
#8610=ORIENTED_EDGE('',*,*,#6075,.T.);
#8611=ORIENTED_EDGE('',*,*,#6076,.F.);
#8612=ORIENTED_EDGE('',*,*,#6075,.F.);
#8613=ORIENTED_EDGE('',*,*,#6077,.F.);
#8614=ORIENTED_EDGE('',*,*,#6078,.T.);
#8615=ORIENTED_EDGE('',*,*,#6079,.F.);
#8616=ORIENTED_EDGE('',*,*,#6078,.F.);
#8617=ORIENTED_EDGE('',*,*,#6080,.T.);
#8618=ORIENTED_EDGE('',*,*,#6081,.T.);
#8619=ORIENTED_EDGE('',*,*,#6082,.F.);
#8620=ORIENTED_EDGE('',*,*,#6083,.F.);
#8621=ORIENTED_EDGE('',*,*,#6084,.T.);
#8622=ORIENTED_EDGE('',*,*,#6083,.T.);
#8623=ORIENTED_EDGE('',*,*,#6085,.F.);
#8624=ORIENTED_EDGE('',*,*,#6086,.F.);
#8625=ORIENTED_EDGE('',*,*,#6087,.T.);
#8626=ORIENTED_EDGE('',*,*,#6086,.T.);
#8627=ORIENTED_EDGE('',*,*,#6088,.F.);
#8628=ORIENTED_EDGE('',*,*,#6089,.F.);
#8629=ORIENTED_EDGE('',*,*,#6090,.T.);
#8630=ORIENTED_EDGE('',*,*,#6089,.T.);
#8631=ORIENTED_EDGE('',*,*,#6091,.F.);
#8632=ORIENTED_EDGE('',*,*,#6081,.F.);
#8633=ORIENTED_EDGE('',*,*,#6091,.T.);
#8634=ORIENTED_EDGE('',*,*,#6088,.T.);
#8635=ORIENTED_EDGE('',*,*,#6085,.T.);
#8636=ORIENTED_EDGE('',*,*,#6082,.T.);
#8637=ORIENTED_EDGE('',*,*,#6074,.T.);
#8638=ORIENTED_EDGE('',*,*,#6077,.T.);
#8639=ORIENTED_EDGE('',*,*,#6090,.F.);
#8640=ORIENTED_EDGE('',*,*,#6080,.F.);
#8641=ORIENTED_EDGE('',*,*,#6084,.F.);
#8642=ORIENTED_EDGE('',*,*,#6087,.F.);
#8643=ORIENTED_EDGE('',*,*,#6076,.T.);
#8644=ORIENTED_EDGE('',*,*,#6079,.T.);
#8645=ORIENTED_EDGE('',*,*,#6092,.T.);
#8646=ORIENTED_EDGE('',*,*,#6093,.T.);
#8647=ORIENTED_EDGE('',*,*,#6094,.F.);
#8648=ORIENTED_EDGE('',*,*,#6093,.F.);
#8649=ORIENTED_EDGE('',*,*,#6094,.T.);
#8650=ORIENTED_EDGE('',*,*,#6092,.F.);
#8651=ORIENTED_EDGE('',*,*,#6095,.T.);
#8652=ORIENTED_EDGE('',*,*,#6096,.T.);
#8653=ORIENTED_EDGE('',*,*,#6097,.T.);
#8654=ORIENTED_EDGE('',*,*,#6098,.T.);
#8655=ORIENTED_EDGE('',*,*,#6099,.T.);
#8656=ORIENTED_EDGE('',*,*,#6100,.T.);
#8657=ORIENTED_EDGE('',*,*,#6099,.F.);
#8658=ORIENTED_EDGE('',*,*,#6101,.T.);
#8659=ORIENTED_EDGE('',*,*,#6102,.T.);
#8660=ORIENTED_EDGE('',*,*,#6103,.T.);
#8661=ORIENTED_EDGE('',*,*,#6095,.F.);
#8662=ORIENTED_EDGE('',*,*,#6104,.T.);
#8663=ORIENTED_EDGE('',*,*,#6105,.T.);
#8664=ORIENTED_EDGE('',*,*,#6106,.T.);
#8665=ORIENTED_EDGE('',*,*,#6102,.F.);
#8666=ORIENTED_EDGE('',*,*,#6107,.T.);
#8667=ORIENTED_EDGE('',*,*,#6108,.T.);
#8668=ORIENTED_EDGE('',*,*,#6109,.T.);
#8669=ORIENTED_EDGE('',*,*,#6105,.F.);
#8670=ORIENTED_EDGE('',*,*,#6110,.T.);
#8671=ORIENTED_EDGE('',*,*,#6111,.T.);
#8672=ORIENTED_EDGE('',*,*,#6112,.T.);
#8673=ORIENTED_EDGE('',*,*,#6108,.F.);
#8674=ORIENTED_EDGE('',*,*,#6113,.T.);
#8675=ORIENTED_EDGE('',*,*,#6114,.T.);
#8676=ORIENTED_EDGE('',*,*,#6115,.T.);
#8677=ORIENTED_EDGE('',*,*,#6111,.F.);
#8678=ORIENTED_EDGE('',*,*,#6116,.T.);
#8679=ORIENTED_EDGE('',*,*,#6117,.T.);
#8680=ORIENTED_EDGE('',*,*,#6118,.T.);
#8681=ORIENTED_EDGE('',*,*,#6114,.F.);
#8682=ORIENTED_EDGE('',*,*,#6119,.T.);
#8683=ORIENTED_EDGE('',*,*,#6120,.T.);
#8684=ORIENTED_EDGE('',*,*,#6121,.T.);
#8685=ORIENTED_EDGE('',*,*,#6117,.F.);
#8686=ORIENTED_EDGE('',*,*,#6122,.T.);
#8687=ORIENTED_EDGE('',*,*,#6123,.T.);
#8688=ORIENTED_EDGE('',*,*,#6124,.T.);
#8689=ORIENTED_EDGE('',*,*,#6120,.F.);
#8690=ORIENTED_EDGE('',*,*,#6125,.T.);
#8691=ORIENTED_EDGE('',*,*,#6126,.T.);
#8692=ORIENTED_EDGE('',*,*,#6127,.T.);
#8693=ORIENTED_EDGE('',*,*,#6123,.F.);
#8694=ORIENTED_EDGE('',*,*,#6128,.T.);
#8695=ORIENTED_EDGE('',*,*,#6129,.T.);
#8696=ORIENTED_EDGE('',*,*,#6130,.T.);
#8697=ORIENTED_EDGE('',*,*,#6126,.F.);
#8698=ORIENTED_EDGE('',*,*,#6131,.T.);
#8699=ORIENTED_EDGE('',*,*,#6132,.F.);
#8700=ORIENTED_EDGE('',*,*,#6133,.T.);
#8701=ORIENTED_EDGE('',*,*,#6134,.F.);
#8702=ORIENTED_EDGE('',*,*,#6135,.T.);
#8703=ORIENTED_EDGE('',*,*,#6136,.T.);
#8704=ORIENTED_EDGE('',*,*,#6137,.T.);
#8705=ORIENTED_EDGE('',*,*,#6138,.F.);
#8706=ORIENTED_EDGE('',*,*,#6139,.F.);
#8707=ORIENTED_EDGE('',*,*,#6140,.T.);
#8708=ORIENTED_EDGE('',*,*,#6141,.T.);
#8709=ORIENTED_EDGE('',*,*,#6136,.F.);
#8710=ORIENTED_EDGE('',*,*,#6142,.F.);
#8711=ORIENTED_EDGE('',*,*,#6143,.T.);
#8712=ORIENTED_EDGE('',*,*,#6144,.T.);
#8713=ORIENTED_EDGE('',*,*,#6140,.F.);
#8714=ORIENTED_EDGE('',*,*,#6145,.F.);
#8715=ORIENTED_EDGE('',*,*,#6146,.T.);
#8716=ORIENTED_EDGE('',*,*,#6147,.T.);
#8717=ORIENTED_EDGE('',*,*,#6143,.F.);
#8718=ORIENTED_EDGE('',*,*,#6148,.F.);
#8719=ORIENTED_EDGE('',*,*,#6149,.T.);
#8720=ORIENTED_EDGE('',*,*,#6150,.T.);
#8721=ORIENTED_EDGE('',*,*,#6146,.F.);
#8722=ORIENTED_EDGE('',*,*,#6151,.F.);
#8723=ORIENTED_EDGE('',*,*,#6152,.T.);
#8724=ORIENTED_EDGE('',*,*,#6153,.T.);
#8725=ORIENTED_EDGE('',*,*,#6149,.F.);
#8726=ORIENTED_EDGE('',*,*,#6154,.F.);
#8727=ORIENTED_EDGE('',*,*,#6155,.T.);
#8728=ORIENTED_EDGE('',*,*,#6156,.T.);
#8729=ORIENTED_EDGE('',*,*,#6152,.F.);
#8730=ORIENTED_EDGE('',*,*,#6157,.F.);
#8731=ORIENTED_EDGE('',*,*,#6158,.T.);
#8732=ORIENTED_EDGE('',*,*,#6159,.T.);
#8733=ORIENTED_EDGE('',*,*,#6155,.F.);
#8734=ORIENTED_EDGE('',*,*,#6160,.F.);
#8735=ORIENTED_EDGE('',*,*,#6161,.T.);
#8736=ORIENTED_EDGE('',*,*,#6162,.T.);
#8737=ORIENTED_EDGE('',*,*,#6158,.F.);
#8738=ORIENTED_EDGE('',*,*,#6163,.F.);
#8739=ORIENTED_EDGE('',*,*,#6164,.T.);
#8740=ORIENTED_EDGE('',*,*,#6165,.T.);
#8741=ORIENTED_EDGE('',*,*,#6161,.F.);
#8742=ORIENTED_EDGE('',*,*,#6166,.F.);
#8743=ORIENTED_EDGE('',*,*,#6167,.T.);
#8744=ORIENTED_EDGE('',*,*,#6168,.T.);
#8745=ORIENTED_EDGE('',*,*,#6164,.F.);
#8746=ORIENTED_EDGE('',*,*,#6169,.F.);
#8747=ORIENTED_EDGE('',*,*,#6170,.T.);
#8748=ORIENTED_EDGE('',*,*,#6171,.T.);
#8749=ORIENTED_EDGE('',*,*,#6167,.F.);
#8750=ORIENTED_EDGE('',*,*,#6172,.F.);
#8751=ORIENTED_EDGE('',*,*,#6173,.F.);
#8752=ORIENTED_EDGE('',*,*,#6174,.F.);
#8753=ORIENTED_EDGE('',*,*,#6175,.F.);
#8754=ORIENTED_EDGE('',*,*,#6176,.T.);
#8755=ORIENTED_EDGE('',*,*,#6177,.T.);
#8756=ORIENTED_EDGE('',*,*,#6178,.T.);
#8757=ORIENTED_EDGE('',*,*,#6179,.T.);
#8758=ORIENTED_EDGE('',*,*,#6180,.T.);
#8759=ORIENTED_EDGE('',*,*,#6181,.T.);
#8760=ORIENTED_EDGE('',*,*,#6180,.F.);
#8761=ORIENTED_EDGE('',*,*,#6182,.T.);
#8762=ORIENTED_EDGE('',*,*,#6183,.T.);
#8763=ORIENTED_EDGE('',*,*,#6184,.T.);
#8764=ORIENTED_EDGE('',*,*,#6185,.T.);
#8765=ORIENTED_EDGE('',*,*,#6177,.F.);
#8766=ORIENTED_EDGE('',*,*,#6186,.T.);
#8767=ORIENTED_EDGE('',*,*,#6187,.T.);
#8768=ORIENTED_EDGE('',*,*,#6188,.T.);
#8769=ORIENTED_EDGE('',*,*,#6184,.F.);
#8770=ORIENTED_EDGE('',*,*,#6189,.T.);
#8771=ORIENTED_EDGE('',*,*,#6190,.T.);
#8772=ORIENTED_EDGE('',*,*,#6191,.T.);
#8773=ORIENTED_EDGE('',*,*,#6187,.F.);
#8774=ORIENTED_EDGE('',*,*,#6192,.T.);
#8775=ORIENTED_EDGE('',*,*,#6193,.T.);
#8776=ORIENTED_EDGE('',*,*,#6194,.T.);
#8777=ORIENTED_EDGE('',*,*,#6190,.F.);
#8778=ORIENTED_EDGE('',*,*,#6195,.T.);
#8779=ORIENTED_EDGE('',*,*,#6196,.T.);
#8780=ORIENTED_EDGE('',*,*,#6197,.T.);
#8781=ORIENTED_EDGE('',*,*,#6193,.F.);
#8782=ORIENTED_EDGE('',*,*,#6198,.T.);
#8783=ORIENTED_EDGE('',*,*,#6199,.T.);
#8784=ORIENTED_EDGE('',*,*,#6200,.T.);
#8785=ORIENTED_EDGE('',*,*,#6196,.F.);
#8786=ORIENTED_EDGE('',*,*,#6201,.T.);
#8787=ORIENTED_EDGE('',*,*,#6202,.T.);
#8788=ORIENTED_EDGE('',*,*,#6203,.T.);
#8789=ORIENTED_EDGE('',*,*,#6199,.F.);
#8790=ORIENTED_EDGE('',*,*,#6204,.T.);
#8791=ORIENTED_EDGE('',*,*,#6205,.T.);
#8792=ORIENTED_EDGE('',*,*,#6206,.T.);
#8793=ORIENTED_EDGE('',*,*,#6202,.F.);
#8794=ORIENTED_EDGE('',*,*,#6207,.T.);
#8795=ORIENTED_EDGE('',*,*,#6208,.T.);
#8796=ORIENTED_EDGE('',*,*,#6209,.T.);
#8797=ORIENTED_EDGE('',*,*,#6205,.F.);
#8798=ORIENTED_EDGE('',*,*,#6210,.T.);
#8799=ORIENTED_EDGE('',*,*,#6211,.T.);
#8800=ORIENTED_EDGE('',*,*,#6212,.T.);
#8801=ORIENTED_EDGE('',*,*,#6208,.F.);
#8802=ORIENTED_EDGE('',*,*,#6213,.T.);
#8803=ORIENTED_EDGE('',*,*,#6214,.T.);
#8804=ORIENTED_EDGE('',*,*,#6215,.T.);
#8805=ORIENTED_EDGE('',*,*,#6211,.F.);
#8806=ORIENTED_EDGE('',*,*,#6216,.T.);
#8807=ORIENTED_EDGE('',*,*,#6217,.T.);
#8808=ORIENTED_EDGE('',*,*,#6218,.T.);
#8809=ORIENTED_EDGE('',*,*,#6214,.F.);
#8810=ORIENTED_EDGE('',*,*,#6219,.T.);
#8811=ORIENTED_EDGE('',*,*,#6220,.T.);
#8812=ORIENTED_EDGE('',*,*,#6221,.T.);
#8813=ORIENTED_EDGE('',*,*,#6217,.F.);
#8814=ORIENTED_EDGE('',*,*,#6222,.T.);
#8815=ORIENTED_EDGE('',*,*,#6223,.T.);
#8816=ORIENTED_EDGE('',*,*,#6224,.T.);
#8817=ORIENTED_EDGE('',*,*,#6220,.F.);
#8818=ORIENTED_EDGE('',*,*,#6225,.T.);
#8819=ORIENTED_EDGE('',*,*,#6226,.T.);
#8820=ORIENTED_EDGE('',*,*,#6227,.T.);
#8821=ORIENTED_EDGE('',*,*,#6223,.F.);
#8822=ORIENTED_EDGE('',*,*,#6228,.T.);
#8823=ORIENTED_EDGE('',*,*,#6229,.T.);
#8824=ORIENTED_EDGE('',*,*,#6230,.T.);
#8825=ORIENTED_EDGE('',*,*,#6226,.F.);
#8826=ORIENTED_EDGE('',*,*,#6231,.T.);
#8827=ORIENTED_EDGE('',*,*,#6232,.F.);
#8828=ORIENTED_EDGE('',*,*,#6233,.T.);
#8829=ORIENTED_EDGE('',*,*,#6234,.F.);
#8830=ORIENTED_EDGE('',*,*,#6235,.T.);
#8831=ORIENTED_EDGE('',*,*,#6236,.T.);
#8832=ORIENTED_EDGE('',*,*,#6237,.T.);
#8833=ORIENTED_EDGE('',*,*,#6238,.F.);
#8834=ORIENTED_EDGE('',*,*,#6239,.F.);
#8835=ORIENTED_EDGE('',*,*,#6240,.T.);
#8836=ORIENTED_EDGE('',*,*,#6241,.T.);
#8837=ORIENTED_EDGE('',*,*,#6236,.F.);
#8838=ORIENTED_EDGE('',*,*,#6242,.F.);
#8839=ORIENTED_EDGE('',*,*,#6243,.T.);
#8840=ORIENTED_EDGE('',*,*,#6244,.T.);
#8841=ORIENTED_EDGE('',*,*,#6240,.F.);
#8842=ORIENTED_EDGE('',*,*,#6245,.F.);
#8843=ORIENTED_EDGE('',*,*,#6246,.T.);
#8844=ORIENTED_EDGE('',*,*,#6247,.T.);
#8845=ORIENTED_EDGE('',*,*,#6243,.F.);
#8846=ORIENTED_EDGE('',*,*,#6248,.F.);
#8847=ORIENTED_EDGE('',*,*,#6249,.T.);
#8848=ORIENTED_EDGE('',*,*,#6250,.T.);
#8849=ORIENTED_EDGE('',*,*,#6246,.F.);
#8850=ORIENTED_EDGE('',*,*,#6251,.F.);
#8851=ORIENTED_EDGE('',*,*,#6252,.T.);
#8852=ORIENTED_EDGE('',*,*,#6253,.T.);
#8853=ORIENTED_EDGE('',*,*,#6249,.F.);
#8854=ORIENTED_EDGE('',*,*,#6254,.F.);
#8855=ORIENTED_EDGE('',*,*,#6255,.T.);
#8856=ORIENTED_EDGE('',*,*,#6256,.T.);
#8857=ORIENTED_EDGE('',*,*,#6252,.F.);
#8858=ORIENTED_EDGE('',*,*,#6257,.F.);
#8859=ORIENTED_EDGE('',*,*,#6258,.T.);
#8860=ORIENTED_EDGE('',*,*,#6259,.T.);
#8861=ORIENTED_EDGE('',*,*,#6255,.F.);
#8862=ORIENTED_EDGE('',*,*,#6260,.F.);
#8863=ORIENTED_EDGE('',*,*,#6261,.T.);
#8864=ORIENTED_EDGE('',*,*,#6262,.T.);
#8865=ORIENTED_EDGE('',*,*,#6258,.F.);
#8866=ORIENTED_EDGE('',*,*,#6263,.F.);
#8867=ORIENTED_EDGE('',*,*,#6264,.T.);
#8868=ORIENTED_EDGE('',*,*,#6265,.T.);
#8869=ORIENTED_EDGE('',*,*,#6261,.F.);
#8870=ORIENTED_EDGE('',*,*,#6266,.F.);
#8871=ORIENTED_EDGE('',*,*,#6267,.T.);
#8872=ORIENTED_EDGE('',*,*,#6268,.T.);
#8873=ORIENTED_EDGE('',*,*,#6264,.F.);
#8874=ORIENTED_EDGE('',*,*,#6269,.F.);
#8875=ORIENTED_EDGE('',*,*,#6270,.T.);
#8876=ORIENTED_EDGE('',*,*,#6271,.T.);
#8877=ORIENTED_EDGE('',*,*,#6267,.F.);
#8878=ORIENTED_EDGE('',*,*,#6272,.F.);
#8879=ORIENTED_EDGE('',*,*,#6273,.T.);
#8880=ORIENTED_EDGE('',*,*,#6274,.T.);
#8881=ORIENTED_EDGE('',*,*,#6270,.F.);
#8882=ORIENTED_EDGE('',*,*,#6275,.F.);
#8883=ORIENTED_EDGE('',*,*,#6276,.T.);
#8884=ORIENTED_EDGE('',*,*,#6277,.T.);
#8885=ORIENTED_EDGE('',*,*,#6273,.F.);
#8886=ORIENTED_EDGE('',*,*,#6278,.F.);
#8887=ORIENTED_EDGE('',*,*,#6279,.T.);
#8888=ORIENTED_EDGE('',*,*,#6280,.T.);
#8889=ORIENTED_EDGE('',*,*,#6276,.F.);
#8890=ORIENTED_EDGE('',*,*,#6281,.F.);
#8891=ORIENTED_EDGE('',*,*,#6282,.T.);
#8892=ORIENTED_EDGE('',*,*,#6283,.T.);
#8893=ORIENTED_EDGE('',*,*,#6279,.F.);
#8894=ORIENTED_EDGE('',*,*,#6284,.F.);
#8895=ORIENTED_EDGE('',*,*,#6285,.T.);
#8896=ORIENTED_EDGE('',*,*,#6286,.T.);
#8897=ORIENTED_EDGE('',*,*,#6282,.F.);
#8898=ORIENTED_EDGE('',*,*,#6287,.F.);
#8899=ORIENTED_EDGE('',*,*,#6288,.F.);
#8900=ORIENTED_EDGE('',*,*,#6289,.F.);
#8901=ORIENTED_EDGE('',*,*,#6290,.F.);
#8902=ORIENTED_EDGE('',*,*,#6291,.T.);
#8903=ORIENTED_EDGE('',*,*,#6179,.F.);
#8904=ORIENTED_EDGE('',*,*,#6292,.T.);
#8905=ORIENTED_EDGE('',*,*,#6238,.T.);
#8906=ORIENTED_EDGE('',*,*,#6293,.T.);
#8907=ORIENTED_EDGE('',*,*,#6182,.F.);
#8908=ORIENTED_EDGE('',*,*,#6288,.T.);
#8909=ORIENTED_EDGE('',*,*,#6294,.T.);
#8910=ORIENTED_EDGE('',*,*,#6285,.F.);
#8911=ORIENTED_EDGE('',*,*,#6295,.F.);
#8912=ORIENTED_EDGE('',*,*,#6293,.F.);
#8913=ORIENTED_EDGE('',*,*,#6237,.F.);
#8914=ORIENTED_EDGE('',*,*,#6241,.F.);
#8915=ORIENTED_EDGE('',*,*,#6244,.F.);
#8916=ORIENTED_EDGE('',*,*,#6247,.F.);
#8917=ORIENTED_EDGE('',*,*,#6250,.F.);
#8918=ORIENTED_EDGE('',*,*,#6253,.F.);
#8919=ORIENTED_EDGE('',*,*,#6256,.F.);
#8920=ORIENTED_EDGE('',*,*,#6259,.F.);
#8921=ORIENTED_EDGE('',*,*,#6262,.F.);
#8922=ORIENTED_EDGE('',*,*,#6265,.F.);
#8923=ORIENTED_EDGE('',*,*,#6268,.F.);
#8924=ORIENTED_EDGE('',*,*,#6271,.F.);
#8925=ORIENTED_EDGE('',*,*,#6274,.F.);
#8926=ORIENTED_EDGE('',*,*,#6277,.F.);
#8927=ORIENTED_EDGE('',*,*,#6280,.F.);
#8928=ORIENTED_EDGE('',*,*,#6283,.F.);
#8929=ORIENTED_EDGE('',*,*,#6286,.F.);
#8930=ORIENTED_EDGE('',*,*,#6294,.F.);
#8931=ORIENTED_EDGE('',*,*,#6291,.F.);
#8932=ORIENTED_EDGE('',*,*,#6296,.F.);
#8933=ORIENTED_EDGE('',*,*,#6233,.F.);
#8934=ORIENTED_EDGE('',*,*,#6297,.F.);
#8935=ORIENTED_EDGE('',*,*,#6231,.F.);
#8936=ORIENTED_EDGE('',*,*,#6228,.F.);
#8937=ORIENTED_EDGE('',*,*,#6225,.F.);
#8938=ORIENTED_EDGE('',*,*,#6222,.F.);
#8939=ORIENTED_EDGE('',*,*,#6219,.F.);
#8940=ORIENTED_EDGE('',*,*,#6216,.F.);
#8941=ORIENTED_EDGE('',*,*,#6213,.F.);
#8942=ORIENTED_EDGE('',*,*,#6210,.F.);
#8943=ORIENTED_EDGE('',*,*,#6207,.F.);
#8944=ORIENTED_EDGE('',*,*,#6204,.F.);
#8945=ORIENTED_EDGE('',*,*,#6201,.F.);
#8946=ORIENTED_EDGE('',*,*,#6198,.F.);
#8947=ORIENTED_EDGE('',*,*,#6195,.F.);
#8948=ORIENTED_EDGE('',*,*,#6192,.F.);
#8949=ORIENTED_EDGE('',*,*,#6189,.F.);
#8950=ORIENTED_EDGE('',*,*,#6186,.F.);
#8951=ORIENTED_EDGE('',*,*,#6183,.F.);
#8952=ORIENTED_EDGE('',*,*,#6292,.F.);
#8953=ORIENTED_EDGE('',*,*,#6178,.F.);
#8954=ORIENTED_EDGE('',*,*,#6185,.F.);
#8955=ORIENTED_EDGE('',*,*,#6188,.F.);
#8956=ORIENTED_EDGE('',*,*,#6191,.F.);
#8957=ORIENTED_EDGE('',*,*,#6194,.F.);
#8958=ORIENTED_EDGE('',*,*,#6197,.F.);
#8959=ORIENTED_EDGE('',*,*,#6200,.F.);
#8960=ORIENTED_EDGE('',*,*,#6203,.F.);
#8961=ORIENTED_EDGE('',*,*,#6206,.F.);
#8962=ORIENTED_EDGE('',*,*,#6209,.F.);
#8963=ORIENTED_EDGE('',*,*,#6212,.F.);
#8964=ORIENTED_EDGE('',*,*,#6215,.F.);
#8965=ORIENTED_EDGE('',*,*,#6218,.F.);
#8966=ORIENTED_EDGE('',*,*,#6221,.F.);
#8967=ORIENTED_EDGE('',*,*,#6224,.F.);
#8968=ORIENTED_EDGE('',*,*,#6227,.F.);
#8969=ORIENTED_EDGE('',*,*,#6230,.F.);
#8970=ORIENTED_EDGE('',*,*,#6298,.F.);
#8971=ORIENTED_EDGE('',*,*,#6235,.F.);
#8972=ORIENTED_EDGE('',*,*,#6299,.F.);
#8973=ORIENTED_EDGE('',*,*,#6289,.T.);
#8974=ORIENTED_EDGE('',*,*,#6295,.T.);
#8975=ORIENTED_EDGE('',*,*,#6287,.T.);
#8976=ORIENTED_EDGE('',*,*,#6284,.T.);
#8977=ORIENTED_EDGE('',*,*,#6281,.T.);
#8978=ORIENTED_EDGE('',*,*,#6278,.T.);
#8979=ORIENTED_EDGE('',*,*,#6275,.T.);
#8980=ORIENTED_EDGE('',*,*,#6272,.T.);
#8981=ORIENTED_EDGE('',*,*,#6269,.T.);
#8982=ORIENTED_EDGE('',*,*,#6266,.T.);
#8983=ORIENTED_EDGE('',*,*,#6263,.T.);
#8984=ORIENTED_EDGE('',*,*,#6260,.T.);
#8985=ORIENTED_EDGE('',*,*,#6257,.T.);
#8986=ORIENTED_EDGE('',*,*,#6254,.T.);
#8987=ORIENTED_EDGE('',*,*,#6251,.T.);
#8988=ORIENTED_EDGE('',*,*,#6248,.T.);
#8989=ORIENTED_EDGE('',*,*,#6245,.T.);
#8990=ORIENTED_EDGE('',*,*,#6242,.T.);
#8991=ORIENTED_EDGE('',*,*,#6239,.T.);
#8992=ORIENTED_EDGE('',*,*,#6232,.T.);
#8993=ORIENTED_EDGE('',*,*,#6298,.T.);
#8994=ORIENTED_EDGE('',*,*,#6229,.F.);
#8995=ORIENTED_EDGE('',*,*,#6297,.T.);
#8996=ORIENTED_EDGE('',*,*,#6181,.F.);
#8997=ORIENTED_EDGE('',*,*,#6097,.F.);
#8998=ORIENTED_EDGE('',*,*,#6300,.T.);
#8999=ORIENTED_EDGE('',*,*,#6138,.T.);
#9000=ORIENTED_EDGE('',*,*,#6301,.T.);
#9001=ORIENTED_EDGE('',*,*,#6173,.T.);
#9002=ORIENTED_EDGE('',*,*,#6302,.T.);
#9003=ORIENTED_EDGE('',*,*,#6170,.F.);
#9004=ORIENTED_EDGE('',*,*,#6303,.F.);
#9005=ORIENTED_EDGE('',*,*,#6301,.F.);
#9006=ORIENTED_EDGE('',*,*,#6137,.F.);
#9007=ORIENTED_EDGE('',*,*,#6141,.F.);
#9008=ORIENTED_EDGE('',*,*,#6144,.F.);
#9009=ORIENTED_EDGE('',*,*,#6147,.F.);
#9010=ORIENTED_EDGE('',*,*,#6150,.F.);
#9011=ORIENTED_EDGE('',*,*,#6153,.F.);
#9012=ORIENTED_EDGE('',*,*,#6156,.F.);
#9013=ORIENTED_EDGE('',*,*,#6159,.F.);
#9014=ORIENTED_EDGE('',*,*,#6162,.F.);
#9015=ORIENTED_EDGE('',*,*,#6165,.F.);
#9016=ORIENTED_EDGE('',*,*,#6168,.F.);
#9017=ORIENTED_EDGE('',*,*,#6171,.F.);
#9018=ORIENTED_EDGE('',*,*,#6302,.F.);
#9019=ORIENTED_EDGE('',*,*,#6176,.F.);
#9020=ORIENTED_EDGE('',*,*,#6304,.F.);
#9021=ORIENTED_EDGE('',*,*,#6133,.F.);
#9022=ORIENTED_EDGE('',*,*,#6305,.F.);
#9023=ORIENTED_EDGE('',*,*,#6131,.F.);
#9024=ORIENTED_EDGE('',*,*,#6128,.F.);
#9025=ORIENTED_EDGE('',*,*,#6125,.F.);
#9026=ORIENTED_EDGE('',*,*,#6122,.F.);
#9027=ORIENTED_EDGE('',*,*,#6119,.F.);
#9028=ORIENTED_EDGE('',*,*,#6116,.F.);
#9029=ORIENTED_EDGE('',*,*,#6113,.F.);
#9030=ORIENTED_EDGE('',*,*,#6110,.F.);
#9031=ORIENTED_EDGE('',*,*,#6107,.F.);
#9032=ORIENTED_EDGE('',*,*,#6104,.F.);
#9033=ORIENTED_EDGE('',*,*,#6101,.F.);
#9034=ORIENTED_EDGE('',*,*,#6098,.F.);
#9035=ORIENTED_EDGE('',*,*,#6300,.F.);
#9036=ORIENTED_EDGE('',*,*,#6096,.F.);
#9037=ORIENTED_EDGE('',*,*,#6103,.F.);
#9038=ORIENTED_EDGE('',*,*,#6106,.F.);
#9039=ORIENTED_EDGE('',*,*,#6109,.F.);
#9040=ORIENTED_EDGE('',*,*,#6112,.F.);
#9041=ORIENTED_EDGE('',*,*,#6115,.F.);
#9042=ORIENTED_EDGE('',*,*,#6118,.F.);
#9043=ORIENTED_EDGE('',*,*,#6121,.F.);
#9044=ORIENTED_EDGE('',*,*,#6124,.F.);
#9045=ORIENTED_EDGE('',*,*,#6127,.F.);
#9046=ORIENTED_EDGE('',*,*,#6130,.F.);
#9047=ORIENTED_EDGE('',*,*,#6306,.F.);
#9048=ORIENTED_EDGE('',*,*,#6135,.F.);
#9049=ORIENTED_EDGE('',*,*,#6307,.F.);
#9050=ORIENTED_EDGE('',*,*,#6174,.T.);
#9051=ORIENTED_EDGE('',*,*,#6303,.T.);
#9052=ORIENTED_EDGE('',*,*,#6172,.T.);
#9053=ORIENTED_EDGE('',*,*,#6169,.T.);
#9054=ORIENTED_EDGE('',*,*,#6166,.T.);
#9055=ORIENTED_EDGE('',*,*,#6163,.T.);
#9056=ORIENTED_EDGE('',*,*,#6160,.T.);
#9057=ORIENTED_EDGE('',*,*,#6157,.T.);
#9058=ORIENTED_EDGE('',*,*,#6154,.T.);
#9059=ORIENTED_EDGE('',*,*,#6151,.T.);
#9060=ORIENTED_EDGE('',*,*,#6148,.T.);
#9061=ORIENTED_EDGE('',*,*,#6145,.T.);
#9062=ORIENTED_EDGE('',*,*,#6142,.T.);
#9063=ORIENTED_EDGE('',*,*,#6139,.T.);
#9064=ORIENTED_EDGE('',*,*,#6132,.T.);
#9065=ORIENTED_EDGE('',*,*,#6306,.T.);
#9066=ORIENTED_EDGE('',*,*,#6129,.F.);
#9067=ORIENTED_EDGE('',*,*,#6305,.T.);
#9068=ORIENTED_EDGE('',*,*,#6100,.F.);
#9069=ORIENTED_EDGE('',*,*,#6308,.T.);
#9070=ORIENTED_EDGE('',*,*,#6309,.T.);
#9071=ORIENTED_EDGE('',*,*,#6310,.F.);
#9072=ORIENTED_EDGE('',*,*,#6311,.F.);
#9073=ORIENTED_EDGE('',*,*,#6312,.T.);
#9074=ORIENTED_EDGE('',*,*,#6311,.T.);
#9075=ORIENTED_EDGE('',*,*,#6313,.F.);
#9076=ORIENTED_EDGE('',*,*,#6314,.F.);
#9077=ORIENTED_EDGE('',*,*,#6315,.T.);
#9078=ORIENTED_EDGE('',*,*,#6314,.T.);
#9079=ORIENTED_EDGE('',*,*,#6316,.F.);
#9080=ORIENTED_EDGE('',*,*,#6317,.F.);
#9081=ORIENTED_EDGE('',*,*,#6318,.T.);
#9082=ORIENTED_EDGE('',*,*,#6317,.T.);
#9083=ORIENTED_EDGE('',*,*,#6319,.F.);
#9084=ORIENTED_EDGE('',*,*,#6309,.F.);
#9085=ORIENTED_EDGE('',*,*,#6319,.T.);
#9086=ORIENTED_EDGE('',*,*,#6316,.T.);
#9087=ORIENTED_EDGE('',*,*,#6313,.T.);
#9088=ORIENTED_EDGE('',*,*,#6310,.T.);
#9089=ORIENTED_EDGE('',*,*,#6299,.T.);
#9090=ORIENTED_EDGE('',*,*,#6234,.T.);
#9091=ORIENTED_EDGE('',*,*,#6296,.T.);
#9092=ORIENTED_EDGE('',*,*,#6290,.T.);
#9093=ORIENTED_EDGE('',*,*,#6318,.F.);
#9094=ORIENTED_EDGE('',*,*,#6308,.F.);
#9095=ORIENTED_EDGE('',*,*,#6312,.F.);
#9096=ORIENTED_EDGE('',*,*,#6315,.F.);
#9097=ORIENTED_EDGE('',*,*,#6307,.T.);
#9098=ORIENTED_EDGE('',*,*,#6134,.T.);
#9099=ORIENTED_EDGE('',*,*,#6304,.T.);
#9100=ORIENTED_EDGE('',*,*,#6175,.T.);
#9101=ORIENTED_EDGE('',*,*,#6320,.T.);
#9102=ORIENTED_EDGE('',*,*,#6321,.T.);
#9103=ORIENTED_EDGE('',*,*,#6322,.T.);
#9104=ORIENTED_EDGE('',*,*,#6323,.T.);
#9105=ORIENTED_EDGE('',*,*,#6324,.T.);
#9106=ORIENTED_EDGE('',*,*,#6323,.F.);
#9107=ORIENTED_EDGE('',*,*,#6325,.T.);
#9108=ORIENTED_EDGE('',*,*,#6326,.T.);
#9109=ORIENTED_EDGE('',*,*,#6327,.T.);
#9110=ORIENTED_EDGE('',*,*,#6328,.T.);
#9111=ORIENTED_EDGE('',*,*,#6320,.F.);
#9112=ORIENTED_EDGE('',*,*,#6329,.T.);
#9113=ORIENTED_EDGE('',*,*,#6330,.T.);
#9114=ORIENTED_EDGE('',*,*,#6331,.T.);
#9115=ORIENTED_EDGE('',*,*,#6327,.F.);
#9116=ORIENTED_EDGE('',*,*,#6332,.T.);
#9117=ORIENTED_EDGE('',*,*,#6333,.T.);
#9118=ORIENTED_EDGE('',*,*,#6334,.T.);
#9119=ORIENTED_EDGE('',*,*,#6330,.F.);
#9120=ORIENTED_EDGE('',*,*,#6335,.T.);
#9121=ORIENTED_EDGE('',*,*,#6336,.T.);
#9122=ORIENTED_EDGE('',*,*,#6337,.T.);
#9123=ORIENTED_EDGE('',*,*,#6333,.F.);
#9124=ORIENTED_EDGE('',*,*,#6338,.T.);
#9125=ORIENTED_EDGE('',*,*,#6339,.T.);
#9126=ORIENTED_EDGE('',*,*,#6340,.T.);
#9127=ORIENTED_EDGE('',*,*,#6336,.F.);
#9128=ORIENTED_EDGE('',*,*,#6341,.T.);
#9129=ORIENTED_EDGE('',*,*,#6342,.T.);
#9130=ORIENTED_EDGE('',*,*,#6343,.T.);
#9131=ORIENTED_EDGE('',*,*,#6339,.F.);
#9132=ORIENTED_EDGE('',*,*,#6344,.T.);
#9133=ORIENTED_EDGE('',*,*,#6345,.T.);
#9134=ORIENTED_EDGE('',*,*,#6346,.T.);
#9135=ORIENTED_EDGE('',*,*,#6342,.F.);
#9136=ORIENTED_EDGE('',*,*,#6347,.T.);
#9137=ORIENTED_EDGE('',*,*,#6348,.T.);
#9138=ORIENTED_EDGE('',*,*,#6349,.T.);
#9139=ORIENTED_EDGE('',*,*,#6345,.F.);
#9140=ORIENTED_EDGE('',*,*,#6350,.T.);
#9141=ORIENTED_EDGE('',*,*,#6351,.F.);
#9142=ORIENTED_EDGE('',*,*,#6352,.T.);
#9143=ORIENTED_EDGE('',*,*,#6353,.F.);
#9144=ORIENTED_EDGE('',*,*,#6354,.T.);
#9145=ORIENTED_EDGE('',*,*,#6355,.T.);
#9146=ORIENTED_EDGE('',*,*,#6356,.T.);
#9147=ORIENTED_EDGE('',*,*,#6357,.F.);
#9148=ORIENTED_EDGE('',*,*,#6358,.F.);
#9149=ORIENTED_EDGE('',*,*,#6359,.T.);
#9150=ORIENTED_EDGE('',*,*,#6360,.T.);
#9151=ORIENTED_EDGE('',*,*,#6355,.F.);
#9152=ORIENTED_EDGE('',*,*,#6361,.F.);
#9153=ORIENTED_EDGE('',*,*,#6362,.T.);
#9154=ORIENTED_EDGE('',*,*,#6363,.T.);
#9155=ORIENTED_EDGE('',*,*,#6359,.F.);
#9156=ORIENTED_EDGE('',*,*,#6364,.F.);
#9157=ORIENTED_EDGE('',*,*,#6365,.T.);
#9158=ORIENTED_EDGE('',*,*,#6366,.T.);
#9159=ORIENTED_EDGE('',*,*,#6362,.F.);
#9160=ORIENTED_EDGE('',*,*,#6367,.F.);
#9161=ORIENTED_EDGE('',*,*,#6368,.T.);
#9162=ORIENTED_EDGE('',*,*,#6369,.T.);
#9163=ORIENTED_EDGE('',*,*,#6365,.F.);
#9164=ORIENTED_EDGE('',*,*,#6370,.F.);
#9165=ORIENTED_EDGE('',*,*,#6371,.T.);
#9166=ORIENTED_EDGE('',*,*,#6372,.T.);
#9167=ORIENTED_EDGE('',*,*,#6368,.F.);
#9168=ORIENTED_EDGE('',*,*,#6373,.F.);
#9169=ORIENTED_EDGE('',*,*,#6374,.T.);
#9170=ORIENTED_EDGE('',*,*,#6375,.T.);
#9171=ORIENTED_EDGE('',*,*,#6371,.F.);
#9172=ORIENTED_EDGE('',*,*,#6376,.F.);
#9173=ORIENTED_EDGE('',*,*,#6377,.T.);
#9174=ORIENTED_EDGE('',*,*,#6378,.T.);
#9175=ORIENTED_EDGE('',*,*,#6374,.F.);
#9176=ORIENTED_EDGE('',*,*,#6379,.F.);
#9177=ORIENTED_EDGE('',*,*,#6380,.T.);
#9178=ORIENTED_EDGE('',*,*,#6381,.T.);
#9179=ORIENTED_EDGE('',*,*,#6377,.F.);
#9180=ORIENTED_EDGE('',*,*,#6382,.F.);
#9181=ORIENTED_EDGE('',*,*,#6383,.F.);
#9182=ORIENTED_EDGE('',*,*,#6384,.F.);
#9183=ORIENTED_EDGE('',*,*,#6385,.F.);
#9184=ORIENTED_EDGE('',*,*,#6386,.T.);
#9185=ORIENTED_EDGE('',*,*,#6322,.F.);
#9186=ORIENTED_EDGE('',*,*,#6387,.T.);
#9187=ORIENTED_EDGE('',*,*,#6357,.T.);
#9188=ORIENTED_EDGE('',*,*,#6388,.T.);
#9189=ORIENTED_EDGE('',*,*,#6325,.F.);
#9190=ORIENTED_EDGE('',*,*,#6383,.T.);
#9191=ORIENTED_EDGE('',*,*,#6389,.T.);
#9192=ORIENTED_EDGE('',*,*,#6380,.F.);
#9193=ORIENTED_EDGE('',*,*,#6390,.F.);
#9194=ORIENTED_EDGE('',*,*,#6388,.F.);
#9195=ORIENTED_EDGE('',*,*,#6356,.F.);
#9196=ORIENTED_EDGE('',*,*,#6360,.F.);
#9197=ORIENTED_EDGE('',*,*,#6363,.F.);
#9198=ORIENTED_EDGE('',*,*,#6366,.F.);
#9199=ORIENTED_EDGE('',*,*,#6369,.F.);
#9200=ORIENTED_EDGE('',*,*,#6372,.F.);
#9201=ORIENTED_EDGE('',*,*,#6375,.F.);
#9202=ORIENTED_EDGE('',*,*,#6378,.F.);
#9203=ORIENTED_EDGE('',*,*,#6381,.F.);
#9204=ORIENTED_EDGE('',*,*,#6389,.F.);
#9205=ORIENTED_EDGE('',*,*,#6386,.F.);
#9206=ORIENTED_EDGE('',*,*,#6391,.F.);
#9207=ORIENTED_EDGE('',*,*,#6352,.F.);
#9208=ORIENTED_EDGE('',*,*,#6392,.F.);
#9209=ORIENTED_EDGE('',*,*,#6350,.F.);
#9210=ORIENTED_EDGE('',*,*,#6347,.F.);
#9211=ORIENTED_EDGE('',*,*,#6344,.F.);
#9212=ORIENTED_EDGE('',*,*,#6341,.F.);
#9213=ORIENTED_EDGE('',*,*,#6338,.F.);
#9214=ORIENTED_EDGE('',*,*,#6335,.F.);
#9215=ORIENTED_EDGE('',*,*,#6332,.F.);
#9216=ORIENTED_EDGE('',*,*,#6329,.F.);
#9217=ORIENTED_EDGE('',*,*,#6326,.F.);
#9218=ORIENTED_EDGE('',*,*,#6387,.F.);
#9219=ORIENTED_EDGE('',*,*,#6321,.F.);
#9220=ORIENTED_EDGE('',*,*,#6328,.F.);
#9221=ORIENTED_EDGE('',*,*,#6331,.F.);
#9222=ORIENTED_EDGE('',*,*,#6334,.F.);
#9223=ORIENTED_EDGE('',*,*,#6337,.F.);
#9224=ORIENTED_EDGE('',*,*,#6340,.F.);
#9225=ORIENTED_EDGE('',*,*,#6343,.F.);
#9226=ORIENTED_EDGE('',*,*,#6346,.F.);
#9227=ORIENTED_EDGE('',*,*,#6349,.F.);
#9228=ORIENTED_EDGE('',*,*,#6393,.F.);
#9229=ORIENTED_EDGE('',*,*,#6354,.F.);
#9230=ORIENTED_EDGE('',*,*,#6394,.F.);
#9231=ORIENTED_EDGE('',*,*,#6384,.T.);
#9232=ORIENTED_EDGE('',*,*,#6390,.T.);
#9233=ORIENTED_EDGE('',*,*,#6382,.T.);
#9234=ORIENTED_EDGE('',*,*,#6379,.T.);
#9235=ORIENTED_EDGE('',*,*,#6376,.T.);
#9236=ORIENTED_EDGE('',*,*,#6373,.T.);
#9237=ORIENTED_EDGE('',*,*,#6370,.T.);
#9238=ORIENTED_EDGE('',*,*,#6367,.T.);
#9239=ORIENTED_EDGE('',*,*,#6364,.T.);
#9240=ORIENTED_EDGE('',*,*,#6361,.T.);
#9241=ORIENTED_EDGE('',*,*,#6358,.T.);
#9242=ORIENTED_EDGE('',*,*,#6351,.T.);
#9243=ORIENTED_EDGE('',*,*,#6393,.T.);
#9244=ORIENTED_EDGE('',*,*,#6348,.F.);
#9245=ORIENTED_EDGE('',*,*,#6392,.T.);
#9246=ORIENTED_EDGE('',*,*,#6324,.F.);
#9247=ORIENTED_EDGE('',*,*,#6395,.F.);
#9248=ORIENTED_EDGE('',*,*,#6396,.T.);
#9249=ORIENTED_EDGE('',*,*,#6397,.F.);
#9250=ORIENTED_EDGE('',*,*,#6396,.F.);
#9251=ORIENTED_EDGE('',*,*,#6398,.T.);
#9252=ORIENTED_EDGE('',*,*,#6399,.T.);
#9253=ORIENTED_EDGE('',*,*,#6400,.F.);
#9254=ORIENTED_EDGE('',*,*,#6401,.F.);
#9255=ORIENTED_EDGE('',*,*,#6402,.F.);
#9256=ORIENTED_EDGE('',*,*,#6403,.F.);
#9257=ORIENTED_EDGE('',*,*,#6398,.F.);
#9258=ORIENTED_EDGE('',*,*,#6404,.F.);
#9259=ORIENTED_EDGE('',*,*,#6397,.T.);
#9260=ORIENTED_EDGE('',*,*,#6405,.F.);
#9261=ORIENTED_EDGE('',*,*,#6399,.F.);
#9262=ORIENTED_EDGE('',*,*,#6403,.T.);
#9263=ORIENTED_EDGE('',*,*,#6406,.F.);
#9264=ORIENTED_EDGE('',*,*,#6407,.T.);
#9265=ORIENTED_EDGE('',*,*,#6408,.T.);
#9266=ORIENTED_EDGE('',*,*,#6402,.T.);
#9267=ORIENTED_EDGE('',*,*,#6409,.F.);
#9268=ORIENTED_EDGE('',*,*,#6410,.T.);
#9269=ORIENTED_EDGE('',*,*,#6406,.T.);
#9270=ORIENTED_EDGE('',*,*,#6411,.F.);
#9271=ORIENTED_EDGE('',*,*,#6412,.F.);
#9272=ORIENTED_EDGE('',*,*,#6413,.T.);
#9273=ORIENTED_EDGE('',*,*,#6409,.T.);
#9274=ORIENTED_EDGE('',*,*,#6404,.T.);
#9275=ORIENTED_EDGE('',*,*,#6401,.T.);
#9276=ORIENTED_EDGE('',*,*,#6414,.T.);
#9277=ORIENTED_EDGE('',*,*,#6412,.T.);
#9278=ORIENTED_EDGE('',*,*,#6415,.F.);
#9279=ORIENTED_EDGE('',*,*,#6408,.F.);
#9280=ORIENTED_EDGE('',*,*,#6405,.T.);
#9281=ORIENTED_EDGE('',*,*,#6415,.T.);
#9282=ORIENTED_EDGE('',*,*,#6411,.T.);
#9283=ORIENTED_EDGE('',*,*,#6400,.T.);
#9284=ORIENTED_EDGE('',*,*,#6394,.T.);
#9285=ORIENTED_EDGE('',*,*,#6353,.T.);
#9286=ORIENTED_EDGE('',*,*,#6391,.T.);
#9287=ORIENTED_EDGE('',*,*,#6385,.T.);
#9288=ORIENTED_EDGE('',*,*,#6395,.T.);
#9289=ORIENTED_EDGE('',*,*,#6414,.F.);
#9290=ORIENTED_EDGE('',*,*,#6407,.F.);
#9291=ORIENTED_EDGE('',*,*,#6410,.F.);
#9292=ORIENTED_EDGE('',*,*,#6413,.F.);
#9293=ORIENTED_EDGE('',*,*,#6416,.F.);
#9294=ORIENTED_EDGE('',*,*,#6417,.T.);
#9295=ORIENTED_EDGE('',*,*,#6418,.F.);
#9296=ORIENTED_EDGE('',*,*,#6417,.F.);
#9297=ORIENTED_EDGE('',*,*,#6419,.T.);
#9298=ORIENTED_EDGE('',*,*,#6420,.T.);
#9299=ORIENTED_EDGE('',*,*,#6421,.F.);
#9300=ORIENTED_EDGE('',*,*,#6422,.F.);
#9301=ORIENTED_EDGE('',*,*,#6423,.T.);
#9302=ORIENTED_EDGE('',*,*,#6422,.T.);
#9303=ORIENTED_EDGE('',*,*,#6424,.F.);
#9304=ORIENTED_EDGE('',*,*,#6425,.F.);
#9305=ORIENTED_EDGE('',*,*,#6426,.T.);
#9306=ORIENTED_EDGE('',*,*,#6425,.T.);
#9307=ORIENTED_EDGE('',*,*,#6427,.F.);
#9308=ORIENTED_EDGE('',*,*,#6428,.F.);
#9309=ORIENTED_EDGE('',*,*,#6429,.T.);
#9310=ORIENTED_EDGE('',*,*,#6428,.T.);
#9311=ORIENTED_EDGE('',*,*,#6430,.F.);
#9312=ORIENTED_EDGE('',*,*,#6420,.F.);
#9313=ORIENTED_EDGE('',*,*,#6430,.T.);
#9314=ORIENTED_EDGE('',*,*,#6427,.T.);
#9315=ORIENTED_EDGE('',*,*,#6424,.T.);
#9316=ORIENTED_EDGE('',*,*,#6421,.T.);
#9317=ORIENTED_EDGE('',*,*,#6416,.T.);
#9318=ORIENTED_EDGE('',*,*,#6429,.F.);
#9319=ORIENTED_EDGE('',*,*,#6419,.F.);
#9320=ORIENTED_EDGE('',*,*,#6423,.F.);
#9321=ORIENTED_EDGE('',*,*,#6426,.F.);
#9322=ORIENTED_EDGE('',*,*,#6418,.T.);
#9323=ORIENTED_EDGE('',*,*,#6431,.T.);
#9324=ORIENTED_EDGE('',*,*,#6431,.F.);
#9325=ORIENTED_EDGE('',*,*,#6432,.F.);
#9326=ORIENTED_EDGE('',*,*,#6433,.T.);
#9327=ORIENTED_EDGE('',*,*,#6434,.F.);
#9328=ORIENTED_EDGE('',*,*,#6435,.T.);
#9329=ORIENTED_EDGE('',*,*,#6432,.T.);
#9330=ORIENTED_EDGE('',*,*,#6435,.F.);
#9331=ORIENTED_EDGE('',*,*,#6434,.T.);
#9332=ORIENTED_EDGE('',*,*,#6433,.F.);
#9333=ORIENTED_EDGE('',*,*,#6436,.T.);
#9334=ORIENTED_EDGE('',*,*,#6437,.T.);
#9335=ORIENTED_EDGE('',*,*,#6436,.F.);
#9336=ORIENTED_EDGE('',*,*,#6437,.F.);
#9337=ORIENTED_EDGE('',*,*,#6438,.T.);
#9338=ORIENTED_EDGE('',*,*,#6439,.T.);
#9339=ORIENTED_EDGE('',*,*,#6440,.F.);
#9340=ORIENTED_EDGE('',*,*,#6439,.F.);
#9341=ORIENTED_EDGE('',*,*,#6440,.T.);
#9342=ORIENTED_EDGE('',*,*,#6438,.F.);
#9343=ORIENTED_EDGE('',*,*,#6441,.F.);
#9344=ORIENTED_EDGE('',*,*,#6442,.T.);
#9345=ORIENTED_EDGE('',*,*,#6443,.T.);
#9346=ORIENTED_EDGE('',*,*,#6444,.T.);
#9347=ORIENTED_EDGE('',*,*,#6445,.F.);
#9348=ORIENTED_EDGE('',*,*,#6446,.T.);
#9349=ORIENTED_EDGE('',*,*,#6441,.T.);
#9350=ORIENTED_EDGE('',*,*,#6447,.T.);
#9351=ORIENTED_EDGE('',*,*,#6448,.F.);
#9352=ORIENTED_EDGE('',*,*,#6449,.T.);
#9353=ORIENTED_EDGE('',*,*,#6445,.T.);
#9354=ORIENTED_EDGE('',*,*,#6450,.T.);
#9355=ORIENTED_EDGE('',*,*,#6451,.F.);
#9356=ORIENTED_EDGE('',*,*,#6452,.T.);
#9357=ORIENTED_EDGE('',*,*,#6448,.T.);
#9358=ORIENTED_EDGE('',*,*,#6453,.T.);
#9359=ORIENTED_EDGE('',*,*,#6454,.F.);
#9360=ORIENTED_EDGE('',*,*,#6455,.T.);
#9361=ORIENTED_EDGE('',*,*,#6451,.T.);
#9362=ORIENTED_EDGE('',*,*,#6456,.T.);
#9363=ORIENTED_EDGE('',*,*,#6457,.F.);
#9364=ORIENTED_EDGE('',*,*,#6458,.T.);
#9365=ORIENTED_EDGE('',*,*,#6454,.T.);
#9366=ORIENTED_EDGE('',*,*,#6459,.T.);
#9367=ORIENTED_EDGE('',*,*,#6460,.F.);
#9368=ORIENTED_EDGE('',*,*,#6461,.T.);
#9369=ORIENTED_EDGE('',*,*,#6457,.T.);
#9370=ORIENTED_EDGE('',*,*,#6462,.T.);
#9371=ORIENTED_EDGE('',*,*,#6463,.F.);
#9372=ORIENTED_EDGE('',*,*,#6464,.T.);
#9373=ORIENTED_EDGE('',*,*,#6460,.T.);
#9374=ORIENTED_EDGE('',*,*,#6465,.T.);
#9375=ORIENTED_EDGE('',*,*,#6466,.F.);
#9376=ORIENTED_EDGE('',*,*,#6467,.T.);
#9377=ORIENTED_EDGE('',*,*,#6463,.T.);
#9378=ORIENTED_EDGE('',*,*,#6468,.T.);
#9379=ORIENTED_EDGE('',*,*,#6469,.F.);
#9380=ORIENTED_EDGE('',*,*,#6470,.T.);
#9381=ORIENTED_EDGE('',*,*,#6466,.T.);
#9382=ORIENTED_EDGE('',*,*,#6471,.T.);
#9383=ORIENTED_EDGE('',*,*,#6472,.F.);
#9384=ORIENTED_EDGE('',*,*,#6473,.T.);
#9385=ORIENTED_EDGE('',*,*,#6469,.T.);
#9386=ORIENTED_EDGE('',*,*,#6474,.T.);
#9387=ORIENTED_EDGE('',*,*,#6475,.F.);
#9388=ORIENTED_EDGE('',*,*,#6476,.T.);
#9389=ORIENTED_EDGE('',*,*,#6472,.T.);
#9390=ORIENTED_EDGE('',*,*,#6477,.T.);
#9391=ORIENTED_EDGE('',*,*,#6478,.F.);
#9392=ORIENTED_EDGE('',*,*,#6479,.T.);
#9393=ORIENTED_EDGE('',*,*,#6475,.T.);
#9394=ORIENTED_EDGE('',*,*,#6480,.T.);
#9395=ORIENTED_EDGE('',*,*,#6481,.F.);
#9396=ORIENTED_EDGE('',*,*,#6482,.T.);
#9397=ORIENTED_EDGE('',*,*,#6478,.T.);
#9398=ORIENTED_EDGE('',*,*,#6483,.T.);
#9399=ORIENTED_EDGE('',*,*,#6484,.F.);
#9400=ORIENTED_EDGE('',*,*,#6485,.T.);
#9401=ORIENTED_EDGE('',*,*,#6481,.T.);
#9402=ORIENTED_EDGE('',*,*,#6486,.T.);
#9403=ORIENTED_EDGE('',*,*,#6487,.F.);
#9404=ORIENTED_EDGE('',*,*,#6488,.T.);
#9405=ORIENTED_EDGE('',*,*,#6484,.T.);
#9406=ORIENTED_EDGE('',*,*,#6489,.T.);
#9407=ORIENTED_EDGE('',*,*,#6490,.F.);
#9408=ORIENTED_EDGE('',*,*,#6491,.T.);
#9409=ORIENTED_EDGE('',*,*,#6492,.T.);
#9410=ORIENTED_EDGE('',*,*,#6493,.F.);
#9411=ORIENTED_EDGE('',*,*,#6494,.F.);
#9412=ORIENTED_EDGE('',*,*,#6495,.T.);
#9413=ORIENTED_EDGE('',*,*,#6490,.T.);
#9414=ORIENTED_EDGE('',*,*,#6496,.F.);
#9415=ORIENTED_EDGE('',*,*,#6497,.F.);
#9416=ORIENTED_EDGE('',*,*,#6498,.T.);
#9417=ORIENTED_EDGE('',*,*,#6494,.T.);
#9418=ORIENTED_EDGE('',*,*,#6499,.F.);
#9419=ORIENTED_EDGE('',*,*,#6500,.F.);
#9420=ORIENTED_EDGE('',*,*,#6501,.T.);
#9421=ORIENTED_EDGE('',*,*,#6497,.T.);
#9422=ORIENTED_EDGE('',*,*,#6502,.F.);
#9423=ORIENTED_EDGE('',*,*,#6503,.F.);
#9424=ORIENTED_EDGE('',*,*,#6504,.T.);
#9425=ORIENTED_EDGE('',*,*,#6500,.T.);
#9426=ORIENTED_EDGE('',*,*,#6505,.F.);
#9427=ORIENTED_EDGE('',*,*,#6506,.F.);
#9428=ORIENTED_EDGE('',*,*,#6507,.T.);
#9429=ORIENTED_EDGE('',*,*,#6503,.T.);
#9430=ORIENTED_EDGE('',*,*,#6508,.F.);
#9431=ORIENTED_EDGE('',*,*,#6509,.F.);
#9432=ORIENTED_EDGE('',*,*,#6510,.T.);
#9433=ORIENTED_EDGE('',*,*,#6506,.T.);
#9434=ORIENTED_EDGE('',*,*,#6511,.F.);
#9435=ORIENTED_EDGE('',*,*,#6512,.F.);
#9436=ORIENTED_EDGE('',*,*,#6513,.T.);
#9437=ORIENTED_EDGE('',*,*,#6509,.T.);
#9438=ORIENTED_EDGE('',*,*,#6514,.F.);
#9439=ORIENTED_EDGE('',*,*,#6515,.F.);
#9440=ORIENTED_EDGE('',*,*,#6516,.T.);
#9441=ORIENTED_EDGE('',*,*,#6512,.T.);
#9442=ORIENTED_EDGE('',*,*,#6517,.F.);
#9443=ORIENTED_EDGE('',*,*,#6518,.F.);
#9444=ORIENTED_EDGE('',*,*,#6519,.T.);
#9445=ORIENTED_EDGE('',*,*,#6515,.T.);
#9446=ORIENTED_EDGE('',*,*,#6520,.F.);
#9447=ORIENTED_EDGE('',*,*,#6521,.F.);
#9448=ORIENTED_EDGE('',*,*,#6522,.T.);
#9449=ORIENTED_EDGE('',*,*,#6518,.T.);
#9450=ORIENTED_EDGE('',*,*,#6523,.F.);
#9451=ORIENTED_EDGE('',*,*,#6524,.F.);
#9452=ORIENTED_EDGE('',*,*,#6525,.T.);
#9453=ORIENTED_EDGE('',*,*,#6521,.T.);
#9454=ORIENTED_EDGE('',*,*,#6526,.F.);
#9455=ORIENTED_EDGE('',*,*,#6527,.F.);
#9456=ORIENTED_EDGE('',*,*,#6528,.T.);
#9457=ORIENTED_EDGE('',*,*,#6524,.T.);
#9458=ORIENTED_EDGE('',*,*,#6529,.F.);
#9459=ORIENTED_EDGE('',*,*,#6530,.F.);
#9460=ORIENTED_EDGE('',*,*,#6531,.T.);
#9461=ORIENTED_EDGE('',*,*,#6527,.T.);
#9462=ORIENTED_EDGE('',*,*,#6532,.F.);
#9463=ORIENTED_EDGE('',*,*,#6533,.F.);
#9464=ORIENTED_EDGE('',*,*,#6534,.T.);
#9465=ORIENTED_EDGE('',*,*,#6530,.T.);
#9466=ORIENTED_EDGE('',*,*,#6535,.F.);
#9467=ORIENTED_EDGE('',*,*,#6536,.F.);
#9468=ORIENTED_EDGE('',*,*,#6537,.T.);
#9469=ORIENTED_EDGE('',*,*,#6533,.T.);
#9470=ORIENTED_EDGE('',*,*,#6538,.F.);
#9471=ORIENTED_EDGE('',*,*,#6539,.F.);
#9472=ORIENTED_EDGE('',*,*,#6492,.F.);
#9473=ORIENTED_EDGE('',*,*,#6540,.F.);
#9474=ORIENTED_EDGE('',*,*,#6541,.F.);
#9475=ORIENTED_EDGE('',*,*,#6542,.F.);
#9476=ORIENTED_EDGE('',*,*,#6543,.T.);
#9477=ORIENTED_EDGE('',*,*,#6544,.F.);
#9478=ORIENTED_EDGE('',*,*,#6543,.F.);
#9479=ORIENTED_EDGE('',*,*,#6540,.T.);
#9480=ORIENTED_EDGE('',*,*,#6491,.F.);
#9481=ORIENTED_EDGE('',*,*,#6495,.F.);
#9482=ORIENTED_EDGE('',*,*,#6498,.F.);
#9483=ORIENTED_EDGE('',*,*,#6501,.F.);
#9484=ORIENTED_EDGE('',*,*,#6504,.F.);
#9485=ORIENTED_EDGE('',*,*,#6507,.F.);
#9486=ORIENTED_EDGE('',*,*,#6510,.F.);
#9487=ORIENTED_EDGE('',*,*,#6513,.F.);
#9488=ORIENTED_EDGE('',*,*,#6516,.F.);
#9489=ORIENTED_EDGE('',*,*,#6519,.F.);
#9490=ORIENTED_EDGE('',*,*,#6522,.F.);
#9491=ORIENTED_EDGE('',*,*,#6525,.F.);
#9492=ORIENTED_EDGE('',*,*,#6528,.F.);
#9493=ORIENTED_EDGE('',*,*,#6531,.F.);
#9494=ORIENTED_EDGE('',*,*,#6534,.F.);
#9495=ORIENTED_EDGE('',*,*,#6537,.F.);
#9496=ORIENTED_EDGE('',*,*,#6545,.F.);
#9497=ORIENTED_EDGE('',*,*,#6546,.F.);
#9498=ORIENTED_EDGE('',*,*,#6442,.F.);
#9499=ORIENTED_EDGE('',*,*,#6446,.F.);
#9500=ORIENTED_EDGE('',*,*,#6449,.F.);
#9501=ORIENTED_EDGE('',*,*,#6452,.F.);
#9502=ORIENTED_EDGE('',*,*,#6455,.F.);
#9503=ORIENTED_EDGE('',*,*,#6458,.F.);
#9504=ORIENTED_EDGE('',*,*,#6461,.F.);
#9505=ORIENTED_EDGE('',*,*,#6464,.F.);
#9506=ORIENTED_EDGE('',*,*,#6467,.F.);
#9507=ORIENTED_EDGE('',*,*,#6470,.F.);
#9508=ORIENTED_EDGE('',*,*,#6473,.F.);
#9509=ORIENTED_EDGE('',*,*,#6476,.F.);
#9510=ORIENTED_EDGE('',*,*,#6479,.F.);
#9511=ORIENTED_EDGE('',*,*,#6482,.F.);
#9512=ORIENTED_EDGE('',*,*,#6485,.F.);
#9513=ORIENTED_EDGE('',*,*,#6488,.F.);
#9514=ORIENTED_EDGE('',*,*,#6547,.F.);
#9515=ORIENTED_EDGE('',*,*,#6536,.T.);
#9516=ORIENTED_EDGE('',*,*,#6548,.F.);
#9517=ORIENTED_EDGE('',*,*,#6549,.F.);
#9518=ORIENTED_EDGE('',*,*,#6545,.T.);
#9519=ORIENTED_EDGE('',*,*,#6539,.T.);
#9520=ORIENTED_EDGE('',*,*,#6542,.T.);
#9521=ORIENTED_EDGE('',*,*,#6550,.F.);
#9522=ORIENTED_EDGE('',*,*,#6489,.F.);
#9523=ORIENTED_EDGE('',*,*,#6486,.F.);
#9524=ORIENTED_EDGE('',*,*,#6483,.F.);
#9525=ORIENTED_EDGE('',*,*,#6480,.F.);
#9526=ORIENTED_EDGE('',*,*,#6477,.F.);
#9527=ORIENTED_EDGE('',*,*,#6474,.F.);
#9528=ORIENTED_EDGE('',*,*,#6471,.F.);
#9529=ORIENTED_EDGE('',*,*,#6468,.F.);
#9530=ORIENTED_EDGE('',*,*,#6465,.F.);
#9531=ORIENTED_EDGE('',*,*,#6462,.F.);
#9532=ORIENTED_EDGE('',*,*,#6459,.F.);
#9533=ORIENTED_EDGE('',*,*,#6456,.F.);
#9534=ORIENTED_EDGE('',*,*,#6453,.F.);
#9535=ORIENTED_EDGE('',*,*,#6450,.F.);
#9536=ORIENTED_EDGE('',*,*,#6447,.F.);
#9537=ORIENTED_EDGE('',*,*,#6444,.F.);
#9538=ORIENTED_EDGE('',*,*,#6551,.F.);
#9539=ORIENTED_EDGE('',*,*,#6548,.T.);
#9540=ORIENTED_EDGE('',*,*,#6538,.T.);
#9541=ORIENTED_EDGE('',*,*,#6535,.T.);
#9542=ORIENTED_EDGE('',*,*,#6532,.T.);
#9543=ORIENTED_EDGE('',*,*,#6529,.T.);
#9544=ORIENTED_EDGE('',*,*,#6526,.T.);
#9545=ORIENTED_EDGE('',*,*,#6523,.T.);
#9546=ORIENTED_EDGE('',*,*,#6520,.T.);
#9547=ORIENTED_EDGE('',*,*,#6517,.T.);
#9548=ORIENTED_EDGE('',*,*,#6514,.T.);
#9549=ORIENTED_EDGE('',*,*,#6511,.T.);
#9550=ORIENTED_EDGE('',*,*,#6508,.T.);
#9551=ORIENTED_EDGE('',*,*,#6505,.T.);
#9552=ORIENTED_EDGE('',*,*,#6502,.T.);
#9553=ORIENTED_EDGE('',*,*,#6499,.T.);
#9554=ORIENTED_EDGE('',*,*,#6496,.T.);
#9555=ORIENTED_EDGE('',*,*,#6493,.T.);
#9556=ORIENTED_EDGE('',*,*,#6487,.T.);
#9557=ORIENTED_EDGE('',*,*,#6550,.T.);
#9558=ORIENTED_EDGE('',*,*,#6541,.T.);
#9559=ORIENTED_EDGE('',*,*,#6547,.T.);
#9560=ORIENTED_EDGE('',*,*,#6552,.F.);
#9561=ORIENTED_EDGE('',*,*,#6553,.T.);
#9562=ORIENTED_EDGE('',*,*,#6554,.T.);
#9563=ORIENTED_EDGE('',*,*,#6555,.F.);
#9564=ORIENTED_EDGE('',*,*,#6556,.F.);
#9565=ORIENTED_EDGE('',*,*,#6557,.T.);
#9566=ORIENTED_EDGE('',*,*,#6558,.T.);
#9567=ORIENTED_EDGE('',*,*,#6553,.F.);
#9568=ORIENTED_EDGE('',*,*,#6559,.F.);
#9569=ORIENTED_EDGE('',*,*,#6560,.T.);
#9570=ORIENTED_EDGE('',*,*,#6561,.T.);
#9571=ORIENTED_EDGE('',*,*,#6557,.F.);
#9572=ORIENTED_EDGE('',*,*,#6562,.F.);
#9573=ORIENTED_EDGE('',*,*,#6563,.T.);
#9574=ORIENTED_EDGE('',*,*,#6564,.T.);
#9575=ORIENTED_EDGE('',*,*,#6560,.F.);
#9576=ORIENTED_EDGE('',*,*,#6565,.F.);
#9577=ORIENTED_EDGE('',*,*,#6566,.T.);
#9578=ORIENTED_EDGE('',*,*,#6567,.T.);
#9579=ORIENTED_EDGE('',*,*,#6563,.F.);
#9580=ORIENTED_EDGE('',*,*,#6568,.F.);
#9581=ORIENTED_EDGE('',*,*,#6555,.T.);
#9582=ORIENTED_EDGE('',*,*,#6569,.T.);
#9583=ORIENTED_EDGE('',*,*,#6566,.F.);
#9584=ORIENTED_EDGE('',*,*,#6569,.F.);
#9585=ORIENTED_EDGE('',*,*,#6554,.F.);
#9586=ORIENTED_EDGE('',*,*,#6558,.F.);
#9587=ORIENTED_EDGE('',*,*,#6561,.F.);
#9588=ORIENTED_EDGE('',*,*,#6564,.F.);
#9589=ORIENTED_EDGE('',*,*,#6567,.F.);
#9590=ORIENTED_EDGE('',*,*,#6570,.T.);
#9591=ORIENTED_EDGE('',*,*,#6546,.T.);
#9592=ORIENTED_EDGE('',*,*,#6549,.T.);
#9593=ORIENTED_EDGE('',*,*,#6551,.T.);
#9594=ORIENTED_EDGE('',*,*,#6443,.F.);
#9595=ORIENTED_EDGE('',*,*,#6570,.F.);
#9596=ORIENTED_EDGE('',*,*,#6571,.T.);
#9597=ORIENTED_EDGE('',*,*,#6572,.T.);
#9598=ORIENTED_EDGE('',*,*,#6571,.F.);
#9599=ORIENTED_EDGE('',*,*,#6572,.F.);
#9600=ORIENTED_EDGE('',*,*,#6552,.T.);
#9601=ORIENTED_EDGE('',*,*,#6568,.T.);
#9602=ORIENTED_EDGE('',*,*,#6565,.T.);
#9603=ORIENTED_EDGE('',*,*,#6562,.T.);
#9604=ORIENTED_EDGE('',*,*,#6559,.T.);
#9605=ORIENTED_EDGE('',*,*,#6556,.T.);
#9606=ORIENTED_EDGE('',*,*,#6544,.T.);
#9607=ORIENTED_EDGE('',*,*,#6573,.F.);
#9608=ORIENTED_EDGE('',*,*,#6574,.T.);
#9609=ORIENTED_EDGE('',*,*,#6575,.T.);
#9610=ORIENTED_EDGE('',*,*,#6576,.T.);
#9611=ORIENTED_EDGE('',*,*,#6577,.F.);
#9612=ORIENTED_EDGE('',*,*,#6578,.T.);
#9613=ORIENTED_EDGE('',*,*,#6573,.T.);
#9614=ORIENTED_EDGE('',*,*,#6579,.T.);
#9615=ORIENTED_EDGE('',*,*,#6580,.F.);
#9616=ORIENTED_EDGE('',*,*,#6581,.T.);
#9617=ORIENTED_EDGE('',*,*,#6577,.T.);
#9618=ORIENTED_EDGE('',*,*,#6582,.T.);
#9619=ORIENTED_EDGE('',*,*,#6583,.F.);
#9620=ORIENTED_EDGE('',*,*,#6584,.T.);
#9621=ORIENTED_EDGE('',*,*,#6580,.T.);
#9622=ORIENTED_EDGE('',*,*,#6585,.T.);
#9623=ORIENTED_EDGE('',*,*,#6586,.F.);
#9624=ORIENTED_EDGE('',*,*,#6587,.T.);
#9625=ORIENTED_EDGE('',*,*,#6583,.T.);
#9626=ORIENTED_EDGE('',*,*,#6588,.T.);
#9627=ORIENTED_EDGE('',*,*,#6589,.F.);
#9628=ORIENTED_EDGE('',*,*,#6590,.T.);
#9629=ORIENTED_EDGE('',*,*,#6586,.T.);
#9630=ORIENTED_EDGE('',*,*,#6591,.T.);
#9631=ORIENTED_EDGE('',*,*,#6592,.F.);
#9632=ORIENTED_EDGE('',*,*,#6593,.T.);
#9633=ORIENTED_EDGE('',*,*,#6589,.T.);
#9634=ORIENTED_EDGE('',*,*,#6594,.T.);
#9635=ORIENTED_EDGE('',*,*,#6595,.F.);
#9636=ORIENTED_EDGE('',*,*,#6596,.T.);
#9637=ORIENTED_EDGE('',*,*,#6592,.T.);
#9638=ORIENTED_EDGE('',*,*,#6597,.T.);
#9639=ORIENTED_EDGE('',*,*,#6598,.F.);
#9640=ORIENTED_EDGE('',*,*,#6599,.T.);
#9641=ORIENTED_EDGE('',*,*,#6595,.T.);
#9642=ORIENTED_EDGE('',*,*,#6600,.T.);
#9643=ORIENTED_EDGE('',*,*,#6601,.F.);
#9644=ORIENTED_EDGE('',*,*,#6602,.T.);
#9645=ORIENTED_EDGE('',*,*,#6598,.T.);
#9646=ORIENTED_EDGE('',*,*,#6603,.T.);
#9647=ORIENTED_EDGE('',*,*,#6604,.F.);
#9648=ORIENTED_EDGE('',*,*,#6605,.T.);
#9649=ORIENTED_EDGE('',*,*,#6606,.T.);
#9650=ORIENTED_EDGE('',*,*,#6607,.F.);
#9651=ORIENTED_EDGE('',*,*,#6608,.F.);
#9652=ORIENTED_EDGE('',*,*,#6609,.T.);
#9653=ORIENTED_EDGE('',*,*,#6604,.T.);
#9654=ORIENTED_EDGE('',*,*,#6610,.F.);
#9655=ORIENTED_EDGE('',*,*,#6611,.F.);
#9656=ORIENTED_EDGE('',*,*,#6612,.T.);
#9657=ORIENTED_EDGE('',*,*,#6608,.T.);
#9658=ORIENTED_EDGE('',*,*,#6613,.F.);
#9659=ORIENTED_EDGE('',*,*,#6614,.F.);
#9660=ORIENTED_EDGE('',*,*,#6615,.T.);
#9661=ORIENTED_EDGE('',*,*,#6611,.T.);
#9662=ORIENTED_EDGE('',*,*,#6616,.F.);
#9663=ORIENTED_EDGE('',*,*,#6617,.F.);
#9664=ORIENTED_EDGE('',*,*,#6618,.T.);
#9665=ORIENTED_EDGE('',*,*,#6614,.T.);
#9666=ORIENTED_EDGE('',*,*,#6619,.F.);
#9667=ORIENTED_EDGE('',*,*,#6620,.F.);
#9668=ORIENTED_EDGE('',*,*,#6621,.T.);
#9669=ORIENTED_EDGE('',*,*,#6617,.T.);
#9670=ORIENTED_EDGE('',*,*,#6622,.F.);
#9671=ORIENTED_EDGE('',*,*,#6623,.F.);
#9672=ORIENTED_EDGE('',*,*,#6624,.T.);
#9673=ORIENTED_EDGE('',*,*,#6620,.T.);
#9674=ORIENTED_EDGE('',*,*,#6625,.F.);
#9675=ORIENTED_EDGE('',*,*,#6626,.F.);
#9676=ORIENTED_EDGE('',*,*,#6627,.T.);
#9677=ORIENTED_EDGE('',*,*,#6623,.T.);
#9678=ORIENTED_EDGE('',*,*,#6628,.F.);
#9679=ORIENTED_EDGE('',*,*,#6629,.F.);
#9680=ORIENTED_EDGE('',*,*,#6630,.T.);
#9681=ORIENTED_EDGE('',*,*,#6626,.T.);
#9682=ORIENTED_EDGE('',*,*,#6631,.F.);
#9683=ORIENTED_EDGE('',*,*,#6632,.F.);
#9684=ORIENTED_EDGE('',*,*,#6633,.T.);
#9685=ORIENTED_EDGE('',*,*,#6629,.T.);
#9686=ORIENTED_EDGE('',*,*,#6634,.F.);
#9687=ORIENTED_EDGE('',*,*,#6635,.F.);
#9688=ORIENTED_EDGE('',*,*,#6606,.F.);
#9689=ORIENTED_EDGE('',*,*,#6636,.F.);
#9690=ORIENTED_EDGE('',*,*,#6637,.F.);
#9691=ORIENTED_EDGE('',*,*,#6638,.F.);
#9692=ORIENTED_EDGE('',*,*,#6639,.T.);
#9693=ORIENTED_EDGE('',*,*,#6640,.F.);
#9694=ORIENTED_EDGE('',*,*,#6639,.F.);
#9695=ORIENTED_EDGE('',*,*,#6636,.T.);
#9696=ORIENTED_EDGE('',*,*,#6605,.F.);
#9697=ORIENTED_EDGE('',*,*,#6609,.F.);
#9698=ORIENTED_EDGE('',*,*,#6612,.F.);
#9699=ORIENTED_EDGE('',*,*,#6615,.F.);
#9700=ORIENTED_EDGE('',*,*,#6618,.F.);
#9701=ORIENTED_EDGE('',*,*,#6621,.F.);
#9702=ORIENTED_EDGE('',*,*,#6624,.F.);
#9703=ORIENTED_EDGE('',*,*,#6627,.F.);
#9704=ORIENTED_EDGE('',*,*,#6630,.F.);
#9705=ORIENTED_EDGE('',*,*,#6633,.F.);
#9706=ORIENTED_EDGE('',*,*,#6641,.F.);
#9707=ORIENTED_EDGE('',*,*,#6642,.F.);
#9708=ORIENTED_EDGE('',*,*,#6574,.F.);
#9709=ORIENTED_EDGE('',*,*,#6578,.F.);
#9710=ORIENTED_EDGE('',*,*,#6581,.F.);
#9711=ORIENTED_EDGE('',*,*,#6584,.F.);
#9712=ORIENTED_EDGE('',*,*,#6587,.F.);
#9713=ORIENTED_EDGE('',*,*,#6590,.F.);
#9714=ORIENTED_EDGE('',*,*,#6593,.F.);
#9715=ORIENTED_EDGE('',*,*,#6596,.F.);
#9716=ORIENTED_EDGE('',*,*,#6599,.F.);
#9717=ORIENTED_EDGE('',*,*,#6602,.F.);
#9718=ORIENTED_EDGE('',*,*,#6643,.F.);
#9719=ORIENTED_EDGE('',*,*,#6632,.T.);
#9720=ORIENTED_EDGE('',*,*,#6644,.F.);
#9721=ORIENTED_EDGE('',*,*,#6645,.F.);
#9722=ORIENTED_EDGE('',*,*,#6641,.T.);
#9723=ORIENTED_EDGE('',*,*,#6635,.T.);
#9724=ORIENTED_EDGE('',*,*,#6638,.T.);
#9725=ORIENTED_EDGE('',*,*,#6646,.F.);
#9726=ORIENTED_EDGE('',*,*,#6603,.F.);
#9727=ORIENTED_EDGE('',*,*,#6600,.F.);
#9728=ORIENTED_EDGE('',*,*,#6597,.F.);
#9729=ORIENTED_EDGE('',*,*,#6594,.F.);
#9730=ORIENTED_EDGE('',*,*,#6591,.F.);
#9731=ORIENTED_EDGE('',*,*,#6588,.F.);
#9732=ORIENTED_EDGE('',*,*,#6585,.F.);
#9733=ORIENTED_EDGE('',*,*,#6582,.F.);
#9734=ORIENTED_EDGE('',*,*,#6579,.F.);
#9735=ORIENTED_EDGE('',*,*,#6576,.F.);
#9736=ORIENTED_EDGE('',*,*,#6647,.F.);
#9737=ORIENTED_EDGE('',*,*,#6644,.T.);
#9738=ORIENTED_EDGE('',*,*,#6634,.T.);
#9739=ORIENTED_EDGE('',*,*,#6631,.T.);
#9740=ORIENTED_EDGE('',*,*,#6628,.T.);
#9741=ORIENTED_EDGE('',*,*,#6625,.T.);
#9742=ORIENTED_EDGE('',*,*,#6622,.T.);
#9743=ORIENTED_EDGE('',*,*,#6619,.T.);
#9744=ORIENTED_EDGE('',*,*,#6616,.T.);
#9745=ORIENTED_EDGE('',*,*,#6613,.T.);
#9746=ORIENTED_EDGE('',*,*,#6610,.T.);
#9747=ORIENTED_EDGE('',*,*,#6607,.T.);
#9748=ORIENTED_EDGE('',*,*,#6601,.T.);
#9749=ORIENTED_EDGE('',*,*,#6646,.T.);
#9750=ORIENTED_EDGE('',*,*,#6637,.T.);
#9751=ORIENTED_EDGE('',*,*,#6643,.T.);
#9752=ORIENTED_EDGE('',*,*,#6648,.F.);
#9753=ORIENTED_EDGE('',*,*,#6649,.T.);
#9754=ORIENTED_EDGE('',*,*,#6650,.T.);
#9755=ORIENTED_EDGE('',*,*,#6651,.F.);
#9756=ORIENTED_EDGE('',*,*,#6652,.F.);
#9757=ORIENTED_EDGE('',*,*,#6653,.T.);
#9758=ORIENTED_EDGE('',*,*,#6654,.T.);
#9759=ORIENTED_EDGE('',*,*,#6649,.F.);
#9760=ORIENTED_EDGE('',*,*,#6655,.F.);
#9761=ORIENTED_EDGE('',*,*,#6656,.T.);
#9762=ORIENTED_EDGE('',*,*,#6657,.T.);
#9763=ORIENTED_EDGE('',*,*,#6653,.F.);
#9764=ORIENTED_EDGE('',*,*,#6658,.F.);
#9765=ORIENTED_EDGE('',*,*,#6659,.T.);
#9766=ORIENTED_EDGE('',*,*,#6660,.T.);
#9767=ORIENTED_EDGE('',*,*,#6656,.F.);
#9768=ORIENTED_EDGE('',*,*,#6661,.F.);
#9769=ORIENTED_EDGE('',*,*,#6662,.T.);
#9770=ORIENTED_EDGE('',*,*,#6663,.T.);
#9771=ORIENTED_EDGE('',*,*,#6659,.F.);
#9772=ORIENTED_EDGE('',*,*,#6664,.F.);
#9773=ORIENTED_EDGE('',*,*,#6651,.T.);
#9774=ORIENTED_EDGE('',*,*,#6665,.T.);
#9775=ORIENTED_EDGE('',*,*,#6662,.F.);
#9776=ORIENTED_EDGE('',*,*,#6665,.F.);
#9777=ORIENTED_EDGE('',*,*,#6650,.F.);
#9778=ORIENTED_EDGE('',*,*,#6654,.F.);
#9779=ORIENTED_EDGE('',*,*,#6657,.F.);
#9780=ORIENTED_EDGE('',*,*,#6660,.F.);
#9781=ORIENTED_EDGE('',*,*,#6663,.F.);
#9782=ORIENTED_EDGE('',*,*,#6666,.T.);
#9783=ORIENTED_EDGE('',*,*,#6642,.T.);
#9784=ORIENTED_EDGE('',*,*,#6645,.T.);
#9785=ORIENTED_EDGE('',*,*,#6647,.T.);
#9786=ORIENTED_EDGE('',*,*,#6575,.F.);
#9787=ORIENTED_EDGE('',*,*,#6666,.F.);
#9788=ORIENTED_EDGE('',*,*,#6667,.T.);
#9789=ORIENTED_EDGE('',*,*,#6668,.T.);
#9790=ORIENTED_EDGE('',*,*,#6667,.F.);
#9791=ORIENTED_EDGE('',*,*,#6668,.F.);
#9792=ORIENTED_EDGE('',*,*,#6648,.T.);
#9793=ORIENTED_EDGE('',*,*,#6664,.T.);
#9794=ORIENTED_EDGE('',*,*,#6661,.T.);
#9795=ORIENTED_EDGE('',*,*,#6658,.T.);
#9796=ORIENTED_EDGE('',*,*,#6655,.T.);
#9797=ORIENTED_EDGE('',*,*,#6652,.T.);
#9798=ORIENTED_EDGE('',*,*,#6640,.T.);
#9799=ORIENTED_EDGE('',*,*,#6669,.F.);
#9800=ORIENTED_EDGE('',*,*,#6670,.T.);
#9801=ORIENTED_EDGE('',*,*,#6671,.T.);
#9802=ORIENTED_EDGE('',*,*,#6672,.T.);
#9803=ORIENTED_EDGE('',*,*,#6673,.F.);
#9804=ORIENTED_EDGE('',*,*,#6674,.T.);
#9805=ORIENTED_EDGE('',*,*,#6669,.T.);
#9806=ORIENTED_EDGE('',*,*,#6675,.T.);
#9807=ORIENTED_EDGE('',*,*,#6676,.F.);
#9808=ORIENTED_EDGE('',*,*,#6677,.T.);
#9809=ORIENTED_EDGE('',*,*,#6673,.T.);
#9810=ORIENTED_EDGE('',*,*,#6678,.T.);
#9811=ORIENTED_EDGE('',*,*,#6679,.F.);
#9812=ORIENTED_EDGE('',*,*,#6680,.T.);
#9813=ORIENTED_EDGE('',*,*,#6676,.T.);
#9814=ORIENTED_EDGE('',*,*,#6681,.T.);
#9815=ORIENTED_EDGE('',*,*,#6682,.F.);
#9816=ORIENTED_EDGE('',*,*,#6683,.T.);
#9817=ORIENTED_EDGE('',*,*,#6679,.T.);
#9818=ORIENTED_EDGE('',*,*,#6684,.T.);
#9819=ORIENTED_EDGE('',*,*,#6685,.F.);
#9820=ORIENTED_EDGE('',*,*,#6686,.T.);
#9821=ORIENTED_EDGE('',*,*,#6682,.T.);
#9822=ORIENTED_EDGE('',*,*,#6687,.T.);
#9823=ORIENTED_EDGE('',*,*,#6688,.F.);
#9824=ORIENTED_EDGE('',*,*,#6689,.T.);
#9825=ORIENTED_EDGE('',*,*,#6685,.T.);
#9826=ORIENTED_EDGE('',*,*,#6690,.T.);
#9827=ORIENTED_EDGE('',*,*,#6691,.F.);
#9828=ORIENTED_EDGE('',*,*,#6692,.T.);
#9829=ORIENTED_EDGE('',*,*,#6688,.T.);
#9830=ORIENTED_EDGE('',*,*,#6693,.T.);
#9831=ORIENTED_EDGE('',*,*,#6694,.F.);
#9832=ORIENTED_EDGE('',*,*,#6695,.T.);
#9833=ORIENTED_EDGE('',*,*,#6691,.T.);
#9834=ORIENTED_EDGE('',*,*,#6696,.T.);
#9835=ORIENTED_EDGE('',*,*,#6697,.F.);
#9836=ORIENTED_EDGE('',*,*,#6698,.T.);
#9837=ORIENTED_EDGE('',*,*,#6694,.T.);
#9838=ORIENTED_EDGE('',*,*,#6699,.T.);
#9839=ORIENTED_EDGE('',*,*,#6700,.F.);
#9840=ORIENTED_EDGE('',*,*,#6701,.T.);
#9841=ORIENTED_EDGE('',*,*,#6697,.T.);
#9842=ORIENTED_EDGE('',*,*,#6702,.T.);
#9843=ORIENTED_EDGE('',*,*,#6703,.F.);
#9844=ORIENTED_EDGE('',*,*,#6704,.T.);
#9845=ORIENTED_EDGE('',*,*,#6700,.T.);
#9846=ORIENTED_EDGE('',*,*,#6705,.T.);
#9847=ORIENTED_EDGE('',*,*,#6706,.F.);
#9848=ORIENTED_EDGE('',*,*,#6707,.T.);
#9849=ORIENTED_EDGE('',*,*,#6703,.T.);
#9850=ORIENTED_EDGE('',*,*,#6708,.T.);
#9851=ORIENTED_EDGE('',*,*,#6709,.F.);
#9852=ORIENTED_EDGE('',*,*,#6710,.T.);
#9853=ORIENTED_EDGE('',*,*,#6706,.T.);
#9854=ORIENTED_EDGE('',*,*,#6711,.T.);
#9855=ORIENTED_EDGE('',*,*,#6712,.F.);
#9856=ORIENTED_EDGE('',*,*,#6713,.T.);
#9857=ORIENTED_EDGE('',*,*,#6709,.T.);
#9858=ORIENTED_EDGE('',*,*,#6714,.T.);
#9859=ORIENTED_EDGE('',*,*,#6715,.F.);
#9860=ORIENTED_EDGE('',*,*,#6716,.T.);
#9861=ORIENTED_EDGE('',*,*,#6712,.T.);
#9862=ORIENTED_EDGE('',*,*,#6717,.T.);
#9863=ORIENTED_EDGE('',*,*,#6718,.F.);
#9864=ORIENTED_EDGE('',*,*,#6719,.T.);
#9865=ORIENTED_EDGE('',*,*,#6715,.T.);
#9866=ORIENTED_EDGE('',*,*,#6720,.T.);
#9867=ORIENTED_EDGE('',*,*,#6721,.F.);
#9868=ORIENTED_EDGE('',*,*,#6722,.T.);
#9869=ORIENTED_EDGE('',*,*,#6718,.T.);
#9870=ORIENTED_EDGE('',*,*,#6723,.T.);
#9871=ORIENTED_EDGE('',*,*,#6724,.F.);
#9872=ORIENTED_EDGE('',*,*,#6725,.T.);
#9873=ORIENTED_EDGE('',*,*,#6726,.T.);
#9874=ORIENTED_EDGE('',*,*,#6727,.F.);
#9875=ORIENTED_EDGE('',*,*,#6728,.F.);
#9876=ORIENTED_EDGE('',*,*,#6729,.T.);
#9877=ORIENTED_EDGE('',*,*,#6724,.T.);
#9878=ORIENTED_EDGE('',*,*,#6730,.F.);
#9879=ORIENTED_EDGE('',*,*,#6731,.F.);
#9880=ORIENTED_EDGE('',*,*,#6732,.T.);
#9881=ORIENTED_EDGE('',*,*,#6728,.T.);
#9882=ORIENTED_EDGE('',*,*,#6733,.F.);
#9883=ORIENTED_EDGE('',*,*,#6734,.F.);
#9884=ORIENTED_EDGE('',*,*,#6735,.T.);
#9885=ORIENTED_EDGE('',*,*,#6731,.T.);
#9886=ORIENTED_EDGE('',*,*,#6736,.F.);
#9887=ORIENTED_EDGE('',*,*,#6737,.F.);
#9888=ORIENTED_EDGE('',*,*,#6738,.T.);
#9889=ORIENTED_EDGE('',*,*,#6734,.T.);
#9890=ORIENTED_EDGE('',*,*,#6739,.F.);
#9891=ORIENTED_EDGE('',*,*,#6740,.F.);
#9892=ORIENTED_EDGE('',*,*,#6741,.T.);
#9893=ORIENTED_EDGE('',*,*,#6737,.T.);
#9894=ORIENTED_EDGE('',*,*,#6742,.F.);
#9895=ORIENTED_EDGE('',*,*,#6743,.F.);
#9896=ORIENTED_EDGE('',*,*,#6744,.T.);
#9897=ORIENTED_EDGE('',*,*,#6740,.T.);
#9898=ORIENTED_EDGE('',*,*,#6745,.F.);
#9899=ORIENTED_EDGE('',*,*,#6746,.F.);
#9900=ORIENTED_EDGE('',*,*,#6747,.T.);
#9901=ORIENTED_EDGE('',*,*,#6743,.T.);
#9902=ORIENTED_EDGE('',*,*,#6748,.F.);
#9903=ORIENTED_EDGE('',*,*,#6749,.F.);
#9904=ORIENTED_EDGE('',*,*,#6750,.T.);
#9905=ORIENTED_EDGE('',*,*,#6746,.T.);
#9906=ORIENTED_EDGE('',*,*,#6751,.F.);
#9907=ORIENTED_EDGE('',*,*,#6752,.F.);
#9908=ORIENTED_EDGE('',*,*,#6753,.T.);
#9909=ORIENTED_EDGE('',*,*,#6749,.T.);
#9910=ORIENTED_EDGE('',*,*,#6754,.F.);
#9911=ORIENTED_EDGE('',*,*,#6755,.F.);
#9912=ORIENTED_EDGE('',*,*,#6756,.T.);
#9913=ORIENTED_EDGE('',*,*,#6752,.T.);
#9914=ORIENTED_EDGE('',*,*,#6757,.F.);
#9915=ORIENTED_EDGE('',*,*,#6758,.F.);
#9916=ORIENTED_EDGE('',*,*,#6759,.T.);
#9917=ORIENTED_EDGE('',*,*,#6755,.T.);
#9918=ORIENTED_EDGE('',*,*,#6760,.F.);
#9919=ORIENTED_EDGE('',*,*,#6761,.F.);
#9920=ORIENTED_EDGE('',*,*,#6762,.T.);
#9921=ORIENTED_EDGE('',*,*,#6758,.T.);
#9922=ORIENTED_EDGE('',*,*,#6763,.F.);
#9923=ORIENTED_EDGE('',*,*,#6764,.F.);
#9924=ORIENTED_EDGE('',*,*,#6765,.T.);
#9925=ORIENTED_EDGE('',*,*,#6761,.T.);
#9926=ORIENTED_EDGE('',*,*,#6766,.F.);
#9927=ORIENTED_EDGE('',*,*,#6767,.F.);
#9928=ORIENTED_EDGE('',*,*,#6768,.T.);
#9929=ORIENTED_EDGE('',*,*,#6764,.T.);
#9930=ORIENTED_EDGE('',*,*,#6769,.F.);
#9931=ORIENTED_EDGE('',*,*,#6770,.F.);
#9932=ORIENTED_EDGE('',*,*,#6771,.T.);
#9933=ORIENTED_EDGE('',*,*,#6767,.T.);
#9934=ORIENTED_EDGE('',*,*,#6772,.F.);
#9935=ORIENTED_EDGE('',*,*,#6773,.F.);
#9936=ORIENTED_EDGE('',*,*,#6774,.T.);
#9937=ORIENTED_EDGE('',*,*,#6770,.T.);
#9938=ORIENTED_EDGE('',*,*,#6775,.F.);
#9939=ORIENTED_EDGE('',*,*,#6776,.F.);
#9940=ORIENTED_EDGE('',*,*,#6777,.T.);
#9941=ORIENTED_EDGE('',*,*,#6773,.T.);
#9942=ORIENTED_EDGE('',*,*,#6778,.F.);
#9943=ORIENTED_EDGE('',*,*,#6779,.F.);
#9944=ORIENTED_EDGE('',*,*,#6726,.F.);
#9945=ORIENTED_EDGE('',*,*,#6780,.F.);
#9946=ORIENTED_EDGE('',*,*,#6781,.F.);
#9947=ORIENTED_EDGE('',*,*,#6782,.F.);
#9948=ORIENTED_EDGE('',*,*,#6783,.T.);
#9949=ORIENTED_EDGE('',*,*,#6784,.F.);
#9950=ORIENTED_EDGE('',*,*,#6783,.F.);
#9951=ORIENTED_EDGE('',*,*,#6780,.T.);
#9952=ORIENTED_EDGE('',*,*,#6725,.F.);
#9953=ORIENTED_EDGE('',*,*,#6729,.F.);
#9954=ORIENTED_EDGE('',*,*,#6732,.F.);
#9955=ORIENTED_EDGE('',*,*,#6735,.F.);
#9956=ORIENTED_EDGE('',*,*,#6738,.F.);
#9957=ORIENTED_EDGE('',*,*,#6741,.F.);
#9958=ORIENTED_EDGE('',*,*,#6744,.F.);
#9959=ORIENTED_EDGE('',*,*,#6747,.F.);
#9960=ORIENTED_EDGE('',*,*,#6750,.F.);
#9961=ORIENTED_EDGE('',*,*,#6753,.F.);
#9962=ORIENTED_EDGE('',*,*,#6756,.F.);
#9963=ORIENTED_EDGE('',*,*,#6759,.F.);
#9964=ORIENTED_EDGE('',*,*,#6762,.F.);
#9965=ORIENTED_EDGE('',*,*,#6765,.F.);
#9966=ORIENTED_EDGE('',*,*,#6768,.F.);
#9967=ORIENTED_EDGE('',*,*,#6771,.F.);
#9968=ORIENTED_EDGE('',*,*,#6774,.F.);
#9969=ORIENTED_EDGE('',*,*,#6777,.F.);
#9970=ORIENTED_EDGE('',*,*,#6785,.F.);
#9971=ORIENTED_EDGE('',*,*,#6786,.F.);
#9972=ORIENTED_EDGE('',*,*,#6670,.F.);
#9973=ORIENTED_EDGE('',*,*,#6674,.F.);
#9974=ORIENTED_EDGE('',*,*,#6677,.F.);
#9975=ORIENTED_EDGE('',*,*,#6680,.F.);
#9976=ORIENTED_EDGE('',*,*,#6683,.F.);
#9977=ORIENTED_EDGE('',*,*,#6686,.F.);
#9978=ORIENTED_EDGE('',*,*,#6689,.F.);
#9979=ORIENTED_EDGE('',*,*,#6692,.F.);
#9980=ORIENTED_EDGE('',*,*,#6695,.F.);
#9981=ORIENTED_EDGE('',*,*,#6698,.F.);
#9982=ORIENTED_EDGE('',*,*,#6701,.F.);
#9983=ORIENTED_EDGE('',*,*,#6704,.F.);
#9984=ORIENTED_EDGE('',*,*,#6707,.F.);
#9985=ORIENTED_EDGE('',*,*,#6710,.F.);
#9986=ORIENTED_EDGE('',*,*,#6713,.F.);
#9987=ORIENTED_EDGE('',*,*,#6716,.F.);
#9988=ORIENTED_EDGE('',*,*,#6719,.F.);
#9989=ORIENTED_EDGE('',*,*,#6722,.F.);
#9990=ORIENTED_EDGE('',*,*,#6787,.F.);
#9991=ORIENTED_EDGE('',*,*,#6776,.T.);
#9992=ORIENTED_EDGE('',*,*,#6788,.F.);
#9993=ORIENTED_EDGE('',*,*,#6789,.F.);
#9994=ORIENTED_EDGE('',*,*,#6785,.T.);
#9995=ORIENTED_EDGE('',*,*,#6779,.T.);
#9996=ORIENTED_EDGE('',*,*,#6782,.T.);
#9997=ORIENTED_EDGE('',*,*,#6790,.F.);
#9998=ORIENTED_EDGE('',*,*,#6723,.F.);
#9999=ORIENTED_EDGE('',*,*,#6720,.F.);
#10000=ORIENTED_EDGE('',*,*,#6717,.F.);
#10001=ORIENTED_EDGE('',*,*,#6714,.F.);
#10002=ORIENTED_EDGE('',*,*,#6711,.F.);
#10003=ORIENTED_EDGE('',*,*,#6708,.F.);
#10004=ORIENTED_EDGE('',*,*,#6705,.F.);
#10005=ORIENTED_EDGE('',*,*,#6702,.F.);
#10006=ORIENTED_EDGE('',*,*,#6699,.F.);
#10007=ORIENTED_EDGE('',*,*,#6696,.F.);
#10008=ORIENTED_EDGE('',*,*,#6693,.F.);
#10009=ORIENTED_EDGE('',*,*,#6690,.F.);
#10010=ORIENTED_EDGE('',*,*,#6687,.F.);
#10011=ORIENTED_EDGE('',*,*,#6684,.F.);
#10012=ORIENTED_EDGE('',*,*,#6681,.F.);
#10013=ORIENTED_EDGE('',*,*,#6678,.F.);
#10014=ORIENTED_EDGE('',*,*,#6675,.F.);
#10015=ORIENTED_EDGE('',*,*,#6672,.F.);
#10016=ORIENTED_EDGE('',*,*,#6791,.F.);
#10017=ORIENTED_EDGE('',*,*,#6788,.T.);
#10018=ORIENTED_EDGE('',*,*,#6778,.T.);
#10019=ORIENTED_EDGE('',*,*,#6775,.T.);
#10020=ORIENTED_EDGE('',*,*,#6772,.T.);
#10021=ORIENTED_EDGE('',*,*,#6769,.T.);
#10022=ORIENTED_EDGE('',*,*,#6766,.T.);
#10023=ORIENTED_EDGE('',*,*,#6763,.T.);
#10024=ORIENTED_EDGE('',*,*,#6760,.T.);
#10025=ORIENTED_EDGE('',*,*,#6757,.T.);
#10026=ORIENTED_EDGE('',*,*,#6754,.T.);
#10027=ORIENTED_EDGE('',*,*,#6751,.T.);
#10028=ORIENTED_EDGE('',*,*,#6748,.T.);
#10029=ORIENTED_EDGE('',*,*,#6745,.T.);
#10030=ORIENTED_EDGE('',*,*,#6742,.T.);
#10031=ORIENTED_EDGE('',*,*,#6739,.T.);
#10032=ORIENTED_EDGE('',*,*,#6736,.T.);
#10033=ORIENTED_EDGE('',*,*,#6733,.T.);
#10034=ORIENTED_EDGE('',*,*,#6730,.T.);
#10035=ORIENTED_EDGE('',*,*,#6727,.T.);
#10036=ORIENTED_EDGE('',*,*,#6721,.T.);
#10037=ORIENTED_EDGE('',*,*,#6790,.T.);
#10038=ORIENTED_EDGE('',*,*,#6781,.T.);
#10039=ORIENTED_EDGE('',*,*,#6787,.T.);
#10040=ORIENTED_EDGE('',*,*,#6792,.F.);
#10041=ORIENTED_EDGE('',*,*,#6793,.T.);
#10042=ORIENTED_EDGE('',*,*,#6794,.T.);
#10043=ORIENTED_EDGE('',*,*,#6795,.F.);
#10044=ORIENTED_EDGE('',*,*,#6796,.F.);
#10045=ORIENTED_EDGE('',*,*,#6797,.T.);
#10046=ORIENTED_EDGE('',*,*,#6798,.T.);
#10047=ORIENTED_EDGE('',*,*,#6793,.F.);
#10048=ORIENTED_EDGE('',*,*,#6799,.F.);
#10049=ORIENTED_EDGE('',*,*,#6800,.T.);
#10050=ORIENTED_EDGE('',*,*,#6801,.T.);
#10051=ORIENTED_EDGE('',*,*,#6797,.F.);
#10052=ORIENTED_EDGE('',*,*,#6802,.F.);
#10053=ORIENTED_EDGE('',*,*,#6803,.T.);
#10054=ORIENTED_EDGE('',*,*,#6804,.T.);
#10055=ORIENTED_EDGE('',*,*,#6800,.F.);
#10056=ORIENTED_EDGE('',*,*,#6805,.F.);
#10057=ORIENTED_EDGE('',*,*,#6806,.T.);
#10058=ORIENTED_EDGE('',*,*,#6807,.T.);
#10059=ORIENTED_EDGE('',*,*,#6803,.F.);
#10060=ORIENTED_EDGE('',*,*,#6808,.F.);
#10061=ORIENTED_EDGE('',*,*,#6795,.T.);
#10062=ORIENTED_EDGE('',*,*,#6809,.T.);
#10063=ORIENTED_EDGE('',*,*,#6806,.F.);
#10064=ORIENTED_EDGE('',*,*,#6809,.F.);
#10065=ORIENTED_EDGE('',*,*,#6794,.F.);
#10066=ORIENTED_EDGE('',*,*,#6798,.F.);
#10067=ORIENTED_EDGE('',*,*,#6801,.F.);
#10068=ORIENTED_EDGE('',*,*,#6804,.F.);
#10069=ORIENTED_EDGE('',*,*,#6807,.F.);
#10070=ORIENTED_EDGE('',*,*,#6810,.T.);
#10071=ORIENTED_EDGE('',*,*,#6786,.T.);
#10072=ORIENTED_EDGE('',*,*,#6789,.T.);
#10073=ORIENTED_EDGE('',*,*,#6791,.T.);
#10074=ORIENTED_EDGE('',*,*,#6671,.F.);
#10075=ORIENTED_EDGE('',*,*,#6810,.F.);
#10076=ORIENTED_EDGE('',*,*,#6811,.T.);
#10077=ORIENTED_EDGE('',*,*,#6812,.T.);
#10078=ORIENTED_EDGE('',*,*,#6811,.F.);
#10079=ORIENTED_EDGE('',*,*,#6812,.F.);
#10080=ORIENTED_EDGE('',*,*,#6792,.T.);
#10081=ORIENTED_EDGE('',*,*,#6808,.T.);
#10082=ORIENTED_EDGE('',*,*,#6805,.T.);
#10083=ORIENTED_EDGE('',*,*,#6802,.T.);
#10084=ORIENTED_EDGE('',*,*,#6799,.T.);
#10085=ORIENTED_EDGE('',*,*,#6796,.T.);
#10086=ORIENTED_EDGE('',*,*,#6784,.T.);
#10087=ORIENTED_EDGE('',*,*,#6813,.F.);
#10088=ORIENTED_EDGE('',*,*,#6814,.T.);
#10089=ORIENTED_EDGE('',*,*,#6815,.T.);
#10090=ORIENTED_EDGE('',*,*,#6816,.T.);
#10091=ORIENTED_EDGE('',*,*,#6817,.F.);
#10092=ORIENTED_EDGE('',*,*,#6818,.T.);
#10093=ORIENTED_EDGE('',*,*,#6813,.T.);
#10094=ORIENTED_EDGE('',*,*,#6819,.T.);
#10095=ORIENTED_EDGE('',*,*,#6820,.F.);
#10096=ORIENTED_EDGE('',*,*,#6821,.T.);
#10097=ORIENTED_EDGE('',*,*,#6822,.T.);
#10098=ORIENTED_EDGE('',*,*,#6823,.F.);
#10099=ORIENTED_EDGE('',*,*,#6824,.F.);
#10100=ORIENTED_EDGE('',*,*,#6825,.T.);
#10101=ORIENTED_EDGE('',*,*,#6820,.T.);
#10102=ORIENTED_EDGE('',*,*,#6826,.F.);
#10103=ORIENTED_EDGE('',*,*,#6827,.F.);
#10104=ORIENTED_EDGE('',*,*,#6822,.F.);
#10105=ORIENTED_EDGE('',*,*,#6828,.F.);
#10106=ORIENTED_EDGE('',*,*,#6829,.F.);
#10107=ORIENTED_EDGE('',*,*,#6830,.F.);
#10108=ORIENTED_EDGE('',*,*,#6831,.T.);
#10109=ORIENTED_EDGE('',*,*,#6832,.F.);
#10110=ORIENTED_EDGE('',*,*,#6831,.F.);
#10111=ORIENTED_EDGE('',*,*,#6828,.T.);
#10112=ORIENTED_EDGE('',*,*,#6821,.F.);
#10113=ORIENTED_EDGE('',*,*,#6825,.F.);
#10114=ORIENTED_EDGE('',*,*,#6833,.F.);
#10115=ORIENTED_EDGE('',*,*,#6834,.F.);
#10116=ORIENTED_EDGE('',*,*,#6814,.F.);
#10117=ORIENTED_EDGE('',*,*,#6818,.F.);
#10118=ORIENTED_EDGE('',*,*,#6835,.F.);
#10119=ORIENTED_EDGE('',*,*,#6824,.T.);
#10120=ORIENTED_EDGE('',*,*,#6836,.F.);
#10121=ORIENTED_EDGE('',*,*,#6837,.F.);
#10122=ORIENTED_EDGE('',*,*,#6833,.T.);
#10123=ORIENTED_EDGE('',*,*,#6827,.T.);
#10124=ORIENTED_EDGE('',*,*,#6830,.T.);
#10125=ORIENTED_EDGE('',*,*,#6838,.F.);
#10126=ORIENTED_EDGE('',*,*,#6819,.F.);
#10127=ORIENTED_EDGE('',*,*,#6816,.F.);
#10128=ORIENTED_EDGE('',*,*,#6839,.F.);
#10129=ORIENTED_EDGE('',*,*,#6836,.T.);
#10130=ORIENTED_EDGE('',*,*,#6826,.T.);
#10131=ORIENTED_EDGE('',*,*,#6823,.T.);
#10132=ORIENTED_EDGE('',*,*,#6817,.T.);
#10133=ORIENTED_EDGE('',*,*,#6838,.T.);
#10134=ORIENTED_EDGE('',*,*,#6829,.T.);
#10135=ORIENTED_EDGE('',*,*,#6835,.T.);
#10136=ORIENTED_EDGE('',*,*,#6840,.F.);
#10137=ORIENTED_EDGE('',*,*,#6841,.T.);
#10138=ORIENTED_EDGE('',*,*,#6842,.T.);
#10139=ORIENTED_EDGE('',*,*,#6843,.F.);
#10140=ORIENTED_EDGE('',*,*,#6844,.F.);
#10141=ORIENTED_EDGE('',*,*,#6845,.T.);
#10142=ORIENTED_EDGE('',*,*,#6846,.T.);
#10143=ORIENTED_EDGE('',*,*,#6841,.F.);
#10144=ORIENTED_EDGE('',*,*,#6847,.F.);
#10145=ORIENTED_EDGE('',*,*,#6848,.T.);
#10146=ORIENTED_EDGE('',*,*,#6849,.T.);
#10147=ORIENTED_EDGE('',*,*,#6845,.F.);
#10148=ORIENTED_EDGE('',*,*,#6850,.F.);
#10149=ORIENTED_EDGE('',*,*,#6851,.T.);
#10150=ORIENTED_EDGE('',*,*,#6852,.T.);
#10151=ORIENTED_EDGE('',*,*,#6848,.F.);
#10152=ORIENTED_EDGE('',*,*,#6853,.F.);
#10153=ORIENTED_EDGE('',*,*,#6854,.T.);
#10154=ORIENTED_EDGE('',*,*,#6855,.T.);
#10155=ORIENTED_EDGE('',*,*,#6851,.F.);
#10156=ORIENTED_EDGE('',*,*,#6856,.F.);
#10157=ORIENTED_EDGE('',*,*,#6843,.T.);
#10158=ORIENTED_EDGE('',*,*,#6857,.T.);
#10159=ORIENTED_EDGE('',*,*,#6854,.F.);
#10160=ORIENTED_EDGE('',*,*,#6857,.F.);
#10161=ORIENTED_EDGE('',*,*,#6842,.F.);
#10162=ORIENTED_EDGE('',*,*,#6846,.F.);
#10163=ORIENTED_EDGE('',*,*,#6849,.F.);
#10164=ORIENTED_EDGE('',*,*,#6852,.F.);
#10165=ORIENTED_EDGE('',*,*,#6855,.F.);
#10166=ORIENTED_EDGE('',*,*,#6858,.T.);
#10167=ORIENTED_EDGE('',*,*,#6834,.T.);
#10168=ORIENTED_EDGE('',*,*,#6837,.T.);
#10169=ORIENTED_EDGE('',*,*,#6839,.T.);
#10170=ORIENTED_EDGE('',*,*,#6815,.F.);
#10171=ORIENTED_EDGE('',*,*,#6858,.F.);
#10172=ORIENTED_EDGE('',*,*,#6859,.T.);
#10173=ORIENTED_EDGE('',*,*,#6860,.T.);
#10174=ORIENTED_EDGE('',*,*,#6859,.F.);
#10175=ORIENTED_EDGE('',*,*,#6860,.F.);
#10176=ORIENTED_EDGE('',*,*,#6840,.T.);
#10177=ORIENTED_EDGE('',*,*,#6856,.T.);
#10178=ORIENTED_EDGE('',*,*,#6853,.T.);
#10179=ORIENTED_EDGE('',*,*,#6850,.T.);
#10180=ORIENTED_EDGE('',*,*,#6847,.T.);
#10181=ORIENTED_EDGE('',*,*,#6844,.T.);
#10182=ORIENTED_EDGE('',*,*,#6832,.T.);
#10183=CYLINDRICAL_SURFACE('',#11438,0.1666);
#10184=CYLINDRICAL_SURFACE('',#11441,0.1666);
#10185=CYLINDRICAL_SURFACE('',#11442,0.1666);
#10186=CYLINDRICAL_SURFACE('',#11443,0.1666);
#10187=CYLINDRICAL_SURFACE('',#11444,0.1666);
#10188=CYLINDRICAL_SURFACE('',#11445,0.1666);
#10189=CYLINDRICAL_SURFACE('',#11446,0.1666);
#10190=CYLINDRICAL_SURFACE('',#11447,0.1666);
#10191=CYLINDRICAL_SURFACE('',#11448,0.1666);
#10192=CYLINDRICAL_SURFACE('',#11449,0.1666);
#10193=CYLINDRICAL_SURFACE('',#11450,0.1666);
#10194=CYLINDRICAL_SURFACE('',#11451,0.1666);
#10195=CYLINDRICAL_SURFACE('',#11453,0.205475000000001);
#10196=CYLINDRICAL_SURFACE('',#11455,0.205475000000001);
#10197=CYLINDRICAL_SURFACE('',#11456,0.205475000000001);
#10198=CYLINDRICAL_SURFACE('',#11457,0.205475000000001);
#10199=CYLINDRICAL_SURFACE('',#11458,0.205475000000001);
#10200=CYLINDRICAL_SURFACE('',#11459,0.205475000000001);
#10201=CYLINDRICAL_SURFACE('',#11460,0.205475000000001);
#10202=CYLINDRICAL_SURFACE('',#11461,0.205475000000001);
#10203=CYLINDRICAL_SURFACE('',#11462,0.205475000000001);
#10204=CYLINDRICAL_SURFACE('',#11463,0.205475000000001);
#10205=CYLINDRICAL_SURFACE('',#11464,0.205475000000001);
#10206=CYLINDRICAL_SURFACE('',#11465,0.205475000000001);
#10207=CYLINDRICAL_SURFACE('',#11466,0.205475000000001);
#10208=CYLINDRICAL_SURFACE('',#11468,0.1666);
#10209=CYLINDRICAL_SURFACE('',#11471,0.1666);
#10210=CYLINDRICAL_SURFACE('',#11472,0.1666);
#10211=CYLINDRICAL_SURFACE('',#11473,0.1666);
#10212=CYLINDRICAL_SURFACE('',#11474,0.1666);
#10213=CYLINDRICAL_SURFACE('',#11475,0.1666);
#10214=CYLINDRICAL_SURFACE('',#11476,0.1666);
#10215=CYLINDRICAL_SURFACE('',#11477,0.1666);
#10216=CYLINDRICAL_SURFACE('',#11478,0.1666);
#10217=CYLINDRICAL_SURFACE('',#11479,0.1666);
#10218=CYLINDRICAL_SURFACE('',#11480,0.1666);
#10219=CYLINDRICAL_SURFACE('',#11481,0.1666);
#10220=CYLINDRICAL_SURFACE('',#11483,0.205475000000001);
#10221=CYLINDRICAL_SURFACE('',#11485,0.205475000000001);
#10222=CYLINDRICAL_SURFACE('',#11486,0.205475000000001);
#10223=CYLINDRICAL_SURFACE('',#11487,0.205475000000001);
#10224=CYLINDRICAL_SURFACE('',#11488,0.205475000000001);
#10225=CYLINDRICAL_SURFACE('',#11489,0.205475000000001);
#10226=CYLINDRICAL_SURFACE('',#11490,0.205475000000001);
#10227=CYLINDRICAL_SURFACE('',#11491,0.205475000000001);
#10228=CYLINDRICAL_SURFACE('',#11492,0.205475000000001);
#10229=CYLINDRICAL_SURFACE('',#11493,0.205475000000001);
#10230=CYLINDRICAL_SURFACE('',#11494,0.205475000000001);
#10231=CYLINDRICAL_SURFACE('',#11495,0.205475000000001);
#10232=CYLINDRICAL_SURFACE('',#11496,0.205475000000001);
#10233=CYLINDRICAL_SURFACE('',#11498,0.1666);
#10234=CYLINDRICAL_SURFACE('',#11501,0.1666);
#10235=CYLINDRICAL_SURFACE('',#11502,0.1666);
#10236=CYLINDRICAL_SURFACE('',#11503,0.1666);
#10237=CYLINDRICAL_SURFACE('',#11504,0.1666);
#10238=CYLINDRICAL_SURFACE('',#11505,0.1666);
#10239=CYLINDRICAL_SURFACE('',#11506,0.1666);
#10240=CYLINDRICAL_SURFACE('',#11507,0.1666);
#10241=CYLINDRICAL_SURFACE('',#11508,0.1666);
#10242=CYLINDRICAL_SURFACE('',#11509,0.1666);
#10243=CYLINDRICAL_SURFACE('',#11510,0.1666);
#10244=CYLINDRICAL_SURFACE('',#11511,0.1666);
#10245=CYLINDRICAL_SURFACE('',#11513,0.205475);
#10246=CYLINDRICAL_SURFACE('',#11515,0.205475);
#10247=CYLINDRICAL_SURFACE('',#11516,0.205475);
#10248=CYLINDRICAL_SURFACE('',#11517,0.205475);
#10249=CYLINDRICAL_SURFACE('',#11518,0.205475);
#10250=CYLINDRICAL_SURFACE('',#11519,0.205475);
#10251=CYLINDRICAL_SURFACE('',#11520,0.205475);
#10252=CYLINDRICAL_SURFACE('',#11521,0.205475);
#10253=CYLINDRICAL_SURFACE('',#11522,0.205475);
#10254=CYLINDRICAL_SURFACE('',#11523,0.205475);
#10255=CYLINDRICAL_SURFACE('',#11524,0.205475);
#10256=CYLINDRICAL_SURFACE('',#11525,0.205475);
#10257=CYLINDRICAL_SURFACE('',#11526,0.205475);
#10258=CYLINDRICAL_SURFACE('',#11528,0.1666);
#10259=CYLINDRICAL_SURFACE('',#11531,0.1666);
#10260=CYLINDRICAL_SURFACE('',#11532,0.1666);
#10261=CYLINDRICAL_SURFACE('',#11533,0.1666);
#10262=CYLINDRICAL_SURFACE('',#11534,0.1666);
#10263=CYLINDRICAL_SURFACE('',#11535,0.1666);
#10264=CYLINDRICAL_SURFACE('',#11536,0.1666);
#10265=CYLINDRICAL_SURFACE('',#11537,0.1666);
#10266=CYLINDRICAL_SURFACE('',#11538,0.1666);
#10267=CYLINDRICAL_SURFACE('',#11539,0.1666);
#10268=CYLINDRICAL_SURFACE('',#11540,0.1666);
#10269=CYLINDRICAL_SURFACE('',#11541,0.1666);
#10270=CYLINDRICAL_SURFACE('',#11543,0.205475);
#10271=CYLINDRICAL_SURFACE('',#11545,0.205475);
#10272=CYLINDRICAL_SURFACE('',#11546,0.205475);
#10273=CYLINDRICAL_SURFACE('',#11547,0.205475);
#10274=CYLINDRICAL_SURFACE('',#11548,0.205475);
#10275=CYLINDRICAL_SURFACE('',#11549,0.205475);
#10276=CYLINDRICAL_SURFACE('',#11550,0.205475);
#10277=CYLINDRICAL_SURFACE('',#11551,0.205475);
#10278=CYLINDRICAL_SURFACE('',#11552,0.205475);
#10279=CYLINDRICAL_SURFACE('',#11553,0.205475);
#10280=CYLINDRICAL_SURFACE('',#11554,0.205475);
#10281=CYLINDRICAL_SURFACE('',#11555,0.205475);
#10282=CYLINDRICAL_SURFACE('',#11556,0.205475);
#10283=CYLINDRICAL_SURFACE('',#11558,0.6);
#10284=CYLINDRICAL_SURFACE('',#11564,0.4);
#10285=CYLINDRICAL_SURFACE('',#11566,0.25);
#10286=CYLINDRICAL_SURFACE('',#11571,0.4);
#10287=CYLINDRICAL_SURFACE('',#11573,0.25);
#10288=CYLINDRICAL_SURFACE('',#11576,0.205475);
#10289=CYLINDRICAL_SURFACE('',#11577,0.1666);
#10290=CYLINDRICAL_SURFACE('',#11579,0.205475);
#10291=CYLINDRICAL_SURFACE('',#11580,0.1666);
#10292=CYLINDRICAL_SURFACE('',#11582,0.205475000000001);
#10293=CYLINDRICAL_SURFACE('',#11583,0.1666);
#10294=CYLINDRICAL_SURFACE('',#11585,0.205475000000001);
#10295=CYLINDRICAL_SURFACE('',#11586,0.1666);
#10296=CYLINDRICAL_SURFACE('',#11591,0.3);
#10297=CYLINDRICAL_SURFACE('',#11594,0.3);
#10298=CYLINDRICAL_SURFACE('',#11605,0.65);
#10299=CYLINDRICAL_SURFACE('',#11608,0.8);
#10300=CYLINDRICAL_SURFACE('',#11617,0.2);
#10301=CYLINDRICAL_SURFACE('',#11620,0.2);
#10302=CYLINDRICAL_SURFACE('',#11623,0.2);
#10303=CYLINDRICAL_SURFACE('',#11627,0.2);
#10304=CYLINDRICAL_SURFACE('',#11637,0.4263);
#10305=CYLINDRICAL_SURFACE('',#11639,0.4263);
#10306=CYLINDRICAL_SURFACE('',#11640,0.4263);
#10307=CYLINDRICAL_SURFACE('',#11642,0.4263);
#10308=CYLINDRICAL_SURFACE('',#11644,0.4263);
#10309=CYLINDRICAL_SURFACE('',#11645,0.4263);
#10310=CYLINDRICAL_SURFACE('',#11647,0.5099);
#10311=CYLINDRICAL_SURFACE('',#11649,0.5099);
#10312=CYLINDRICAL_SURFACE('',#11650,0.5099);
#10313=CYLINDRICAL_SURFACE('',#11651,0.5099);
#10314=CYLINDRICAL_SURFACE('',#11653,0.5099);
#10315=CYLINDRICAL_SURFACE('',#11655,0.5099);
#10316=CYLINDRICAL_SURFACE('',#11656,0.5099);
#10317=CYLINDRICAL_SURFACE('',#11657,0.5099);
#10318=CYLINDRICAL_SURFACE('',#11677,0.5099);
#10319=CYLINDRICAL_SURFACE('',#11678,0.5099);
#10320=CYLINDRICAL_SURFACE('',#11679,0.4263);
#10321=CYLINDRICAL_SURFACE('',#11682,0.4);
#10322=CYLINDRICAL_SURFACE('',#11686,0.2);
#10323=CYLINDRICAL_SURFACE('',#11687,0.7);
#10324=CYLINDRICAL_SURFACE('',#11699,2.4);
#10325=CYLINDRICAL_SURFACE('',#11700,0.4263);
#10326=CYLINDRICAL_SURFACE('',#11703,0.4);
#10327=CYLINDRICAL_SURFACE('',#11707,0.2);
#10328=CYLINDRICAL_SURFACE('',#11710,0.7);
#10329=CYLINDRICAL_SURFACE('',#11711,2.4);
#10330=CYLINDRICAL_SURFACE('',#11712,0.25);
#10331=CYLINDRICAL_SURFACE('',#11714,0.25);
#10332=CYLINDRICAL_SURFACE('',#11716,0.25);
#10333=CYLINDRICAL_SURFACE('',#11718,0.25);
#10334=CYLINDRICAL_SURFACE('',#11720,0.6);
#10335=CYLINDRICAL_SURFACE('',#11731,0.8);
#10336=CYLINDRICAL_SURFACE('',#11735,0.4);
#10337=CYLINDRICAL_SURFACE('',#11737,0.6);
#10338=CYLINDRICAL_SURFACE('',#11741,0.1666);
#10339=CYLINDRICAL_SURFACE('',#11744,0.1666);
#10340=CYLINDRICAL_SURFACE('',#11745,0.1666);
#10341=CYLINDRICAL_SURFACE('',#11746,0.1666);
#10342=CYLINDRICAL_SURFACE('',#11747,0.1666);
#10343=CYLINDRICAL_SURFACE('',#11748,0.1666);
#10344=CYLINDRICAL_SURFACE('',#11749,0.1666);
#10345=CYLINDRICAL_SURFACE('',#11750,0.1666);
#10346=CYLINDRICAL_SURFACE('',#11751,0.1666);
#10347=CYLINDRICAL_SURFACE('',#11752,0.1666);
#10348=CYLINDRICAL_SURFACE('',#11753,0.1666);
#10349=CYLINDRICAL_SURFACE('',#11754,0.1666);
#10350=CYLINDRICAL_SURFACE('',#11756,0.205475);
#10351=CYLINDRICAL_SURFACE('',#11758,0.205475);
#10352=CYLINDRICAL_SURFACE('',#11759,0.205475);
#10353=CYLINDRICAL_SURFACE('',#11760,0.205475);
#10354=CYLINDRICAL_SURFACE('',#11761,0.205475);
#10355=CYLINDRICAL_SURFACE('',#11762,0.205475);
#10356=CYLINDRICAL_SURFACE('',#11763,0.205475);
#10357=CYLINDRICAL_SURFACE('',#11764,0.205475);
#10358=CYLINDRICAL_SURFACE('',#11765,0.205475);
#10359=CYLINDRICAL_SURFACE('',#11766,0.205475);
#10360=CYLINDRICAL_SURFACE('',#11767,0.205475);
#10361=CYLINDRICAL_SURFACE('',#11768,0.205475);
#10362=CYLINDRICAL_SURFACE('',#11769,0.205475);
#10363=CYLINDRICAL_SURFACE('',#11771,0.12645);
#10364=CYLINDRICAL_SURFACE('',#11773,0.12645);
#10365=CYLINDRICAL_SURFACE('',#11774,0.12645);
#10366=CYLINDRICAL_SURFACE('',#11775,0.12645);
#10367=CYLINDRICAL_SURFACE('',#11776,0.12645);
#10368=CYLINDRICAL_SURFACE('',#11777,0.12645);
#10369=CYLINDRICAL_SURFACE('',#11778,0.12645);
#10370=CYLINDRICAL_SURFACE('',#11779,0.12645);
#10371=CYLINDRICAL_SURFACE('',#11781,0.12645);
#10372=CYLINDRICAL_SURFACE('',#11783,0.12645);
#10373=CYLINDRICAL_SURFACE('',#11784,0.12645);
#10374=CYLINDRICAL_SURFACE('',#11785,0.12645);
#10375=CYLINDRICAL_SURFACE('',#11786,0.12645);
#10376=CYLINDRICAL_SURFACE('',#11787,0.12645);
#10377=CYLINDRICAL_SURFACE('',#11788,0.12645);
#10378=CYLINDRICAL_SURFACE('',#11789,0.12645);
#10379=CYLINDRICAL_SURFACE('',#11791,0.1543);
#10380=CYLINDRICAL_SURFACE('',#11793,0.1543);
#10381=CYLINDRICAL_SURFACE('',#11794,0.1543);
#10382=CYLINDRICAL_SURFACE('',#11795,0.1543);
#10383=CYLINDRICAL_SURFACE('',#11796,0.1543);
#10384=CYLINDRICAL_SURFACE('',#11797,0.1543);
#10385=CYLINDRICAL_SURFACE('',#11798,0.1543);
#10386=CYLINDRICAL_SURFACE('',#11799,0.1543);
#10387=CYLINDRICAL_SURFACE('',#11801,0.1543);
#10388=CYLINDRICAL_SURFACE('',#11803,0.1543);
#10389=CYLINDRICAL_SURFACE('',#11804,0.1543);
#10390=CYLINDRICAL_SURFACE('',#11805,0.1543);
#10391=CYLINDRICAL_SURFACE('',#11806,0.1543);
#10392=CYLINDRICAL_SURFACE('',#11807,0.1543);
#10393=CYLINDRICAL_SURFACE('',#11808,0.1543);
#10394=CYLINDRICAL_SURFACE('',#11809,0.1543);
#10395=CYLINDRICAL_SURFACE('',#11811,0.1543);
#10396=CYLINDRICAL_SURFACE('',#11814,0.1543);
#10397=CYLINDRICAL_SURFACE('',#11815,0.12645);
#10398=CYLINDRICAL_SURFACE('',#11816,0.12645);
#10399=CYLINDRICAL_SURFACE('',#11818,0.205475);
#10400=CYLINDRICAL_SURFACE('',#11819,0.1666);
#10401=CYLINDRICAL_SURFACE('',#11825,0.6);
#10402=CYLINDRICAL_SURFACE('',#11830,0.6);
#10403=CYLINDRICAL_SURFACE('',#11838,1.);
#10404=CYLINDRICAL_SURFACE('',#11839,0.6);
#10405=CYLINDRICAL_SURFACE('',#11845,1.);
#10406=CYLINDRICAL_SURFACE('',#11847,0.6);
#10407=CYLINDRICAL_SURFACE('',#11856,2.2);
#10408=CYLINDRICAL_SURFACE('',#11868,0.4);
#10409=CYLINDRICAL_SURFACE('',#11872,0.25);
#10410=CYLINDRICAL_SURFACE('',#11873,0.6);
#10411=CYLINDRICAL_SURFACE('',#11875,1.);
#10412=CYLINDRICAL_SURFACE('',#11879,0.2);
#10413=CYLINDRICAL_SURFACE('',#11882,0.2);
#10414=CYLINDRICAL_SURFACE('',#11897,0.1666);
#10415=CYLINDRICAL_SURFACE('',#11900,0.1666);
#10416=CYLINDRICAL_SURFACE('',#11901,0.1666);
#10417=CYLINDRICAL_SURFACE('',#11902,0.1666);
#10418=CYLINDRICAL_SURFACE('',#11903,0.1666);
#10419=CYLINDRICAL_SURFACE('',#11904,0.1666);
#10420=CYLINDRICAL_SURFACE('',#11905,0.1666);
#10421=CYLINDRICAL_SURFACE('',#11906,0.1666);
#10422=CYLINDRICAL_SURFACE('',#11907,0.1666);
#10423=CYLINDRICAL_SURFACE('',#11908,0.1666);
#10424=CYLINDRICAL_SURFACE('',#11909,0.1666);
#10425=CYLINDRICAL_SURFACE('',#11910,0.1666);
#10426=CYLINDRICAL_SURFACE('',#11912,0.205475);
#10427=CYLINDRICAL_SURFACE('',#11914,0.205475);
#10428=CYLINDRICAL_SURFACE('',#11915,0.205475);
#10429=CYLINDRICAL_SURFACE('',#11916,0.205475);
#10430=CYLINDRICAL_SURFACE('',#11917,0.205475);
#10431=CYLINDRICAL_SURFACE('',#11918,0.205475);
#10432=CYLINDRICAL_SURFACE('',#11919,0.205475);
#10433=CYLINDRICAL_SURFACE('',#11920,0.205475);
#10434=CYLINDRICAL_SURFACE('',#11921,0.205475);
#10435=CYLINDRICAL_SURFACE('',#11922,0.205475);
#10436=CYLINDRICAL_SURFACE('',#11923,0.205475);
#10437=CYLINDRICAL_SURFACE('',#11924,0.205475);
#10438=CYLINDRICAL_SURFACE('',#11925,0.205475);
#10439=CYLINDRICAL_SURFACE('',#11927,0.12645);
#10440=CYLINDRICAL_SURFACE('',#11931,0.12645);
#10441=CYLINDRICAL_SURFACE('',#11932,0.12645);
#10442=CYLINDRICAL_SURFACE('',#11933,0.12645);
#10443=CYLINDRICAL_SURFACE('',#11934,0.12645);
#10444=CYLINDRICAL_SURFACE('',#11935,0.12645);
#10445=CYLINDRICAL_SURFACE('',#11936,0.12645);
#10446=CYLINDRICAL_SURFACE('',#11937,0.12645);
#10447=CYLINDRICAL_SURFACE('',#11938,0.12645);
#10448=CYLINDRICAL_SURFACE('',#11939,0.12645);
#10449=CYLINDRICAL_SURFACE('',#11940,0.12645);
#10450=CYLINDRICAL_SURFACE('',#11941,0.12645);
#10451=CYLINDRICAL_SURFACE('',#11942,0.12645);
#10452=CYLINDRICAL_SURFACE('',#11943,0.12645);
#10453=CYLINDRICAL_SURFACE('',#11944,0.12645);
#10454=CYLINDRICAL_SURFACE('',#11945,0.12645);
#10455=CYLINDRICAL_SURFACE('',#11946,0.12645);
#10456=CYLINDRICAL_SURFACE('',#11947,0.12645);
#10457=CYLINDRICAL_SURFACE('',#11949,0.1543);
#10458=CYLINDRICAL_SURFACE('',#11951,0.1543);
#10459=CYLINDRICAL_SURFACE('',#11952,0.1543);
#10460=CYLINDRICAL_SURFACE('',#11953,0.1543);
#10461=CYLINDRICAL_SURFACE('',#11954,0.1543);
#10462=CYLINDRICAL_SURFACE('',#11955,0.1543);
#10463=CYLINDRICAL_SURFACE('',#11956,0.1543);
#10464=CYLINDRICAL_SURFACE('',#11957,0.1543);
#10465=CYLINDRICAL_SURFACE('',#11958,0.1543);
#10466=CYLINDRICAL_SURFACE('',#11959,0.1543);
#10467=CYLINDRICAL_SURFACE('',#11960,0.1543);
#10468=CYLINDRICAL_SURFACE('',#11961,0.1543);
#10469=CYLINDRICAL_SURFACE('',#11962,0.1543);
#10470=CYLINDRICAL_SURFACE('',#11963,0.1543);
#10471=CYLINDRICAL_SURFACE('',#11964,0.1543);
#10472=CYLINDRICAL_SURFACE('',#11965,0.1543);
#10473=CYLINDRICAL_SURFACE('',#11966,0.1543);
#10474=CYLINDRICAL_SURFACE('',#11967,0.1543);
#10475=CYLINDRICAL_SURFACE('',#11970,0.1543);
#10476=CYLINDRICAL_SURFACE('',#11971,0.12645);
#10477=CYLINDRICAL_SURFACE('',#11974,0.205475);
#10478=CYLINDRICAL_SURFACE('',#11975,0.1666);
#10479=CYLINDRICAL_SURFACE('',#11984,0.12645);
#10480=CYLINDRICAL_SURFACE('',#11988,0.12645);
#10481=CYLINDRICAL_SURFACE('',#11989,0.12645);
#10482=CYLINDRICAL_SURFACE('',#11990,0.12645);
#10483=CYLINDRICAL_SURFACE('',#11991,0.12645);
#10484=CYLINDRICAL_SURFACE('',#11992,0.12645);
#10485=CYLINDRICAL_SURFACE('',#11993,0.12645);
#10486=CYLINDRICAL_SURFACE('',#11994,0.12645);
#10487=CYLINDRICAL_SURFACE('',#11995,0.12645);
#10488=CYLINDRICAL_SURFACE('',#11996,0.12645);
#10489=CYLINDRICAL_SURFACE('',#11998,0.1543);
#10490=CYLINDRICAL_SURFACE('',#12000,0.1543);
#10491=CYLINDRICAL_SURFACE('',#12001,0.1543);
#10492=CYLINDRICAL_SURFACE('',#12002,0.1543);
#10493=CYLINDRICAL_SURFACE('',#12003,0.1543);
#10494=CYLINDRICAL_SURFACE('',#12004,0.1543);
#10495=CYLINDRICAL_SURFACE('',#12005,0.1543);
#10496=CYLINDRICAL_SURFACE('',#12006,0.1543);
#10497=CYLINDRICAL_SURFACE('',#12007,0.1543);
#10498=CYLINDRICAL_SURFACE('',#12008,0.1543);
#10499=CYLINDRICAL_SURFACE('',#12011,0.1543);
#10500=CYLINDRICAL_SURFACE('',#12012,0.12645);
#10501=CYLINDRICAL_SURFACE('',#12014,0.2);
#10502=CYLINDRICAL_SURFACE('',#12026,0.2);
#10503=CYLINDRICAL_SURFACE('',#12042,0.35);
#10504=CYLINDRICAL_SURFACE('',#12045,0.2);
#10505=CYLINDRICAL_SURFACE('',#12054,0.1954);
#10506=CYLINDRICAL_SURFACE('',#12056,0.1954);
#10507=CYLINDRICAL_SURFACE('',#12057,0.1954);
#10508=CYLINDRICAL_SURFACE('',#12058,0.1954);
#10509=CYLINDRICAL_SURFACE('',#12059,0.1954);
#10510=CYLINDRICAL_SURFACE('',#12060,0.1954);
#10511=CYLINDRICAL_SURFACE('',#12061,0.1954);
#10512=CYLINDRICAL_SURFACE('',#12062,0.1954);
#10513=CYLINDRICAL_SURFACE('',#12063,0.1954);
#10514=CYLINDRICAL_SURFACE('',#12064,0.1954);
#10515=CYLINDRICAL_SURFACE('',#12065,0.1954);
#10516=CYLINDRICAL_SURFACE('',#12066,0.1954);
#10517=CYLINDRICAL_SURFACE('',#12067,0.1954);
#10518=CYLINDRICAL_SURFACE('',#12068,0.1954);
#10519=CYLINDRICAL_SURFACE('',#12069,0.1954);
#10520=CYLINDRICAL_SURFACE('',#12070,0.1954);
#10521=CYLINDRICAL_SURFACE('',#12071,0.15555);
#10522=CYLINDRICAL_SURFACE('',#12073,0.15555);
#10523=CYLINDRICAL_SURFACE('',#12074,0.15555);
#10524=CYLINDRICAL_SURFACE('',#12075,0.15555);
#10525=CYLINDRICAL_SURFACE('',#12076,0.15555);
#10526=CYLINDRICAL_SURFACE('',#12077,0.15555);
#10527=CYLINDRICAL_SURFACE('',#12078,0.15555);
#10528=CYLINDRICAL_SURFACE('',#12079,0.15555);
#10529=CYLINDRICAL_SURFACE('',#12080,0.15555);
#10530=CYLINDRICAL_SURFACE('',#12081,0.15555);
#10531=CYLINDRICAL_SURFACE('',#12082,0.15555);
#10532=CYLINDRICAL_SURFACE('',#12083,0.15555);
#10533=CYLINDRICAL_SURFACE('',#12084,0.15555);
#10534=CYLINDRICAL_SURFACE('',#12085,0.15555);
#10535=CYLINDRICAL_SURFACE('',#12086,0.15555);
#10536=CYLINDRICAL_SURFACE('',#12087,0.15555);
#10537=CYLINDRICAL_SURFACE('',#12091,0.15555);
#10538=CYLINDRICAL_SURFACE('',#12093,0.1954);
#10539=CYLINDRICAL_SURFACE('',#12103,0.35);
#10540=CYLINDRICAL_SURFACE('',#12108,0.14635);
#10541=CYLINDRICAL_SURFACE('',#12110,0.14635);
#10542=CYLINDRICAL_SURFACE('',#12111,0.14635);
#10543=CYLINDRICAL_SURFACE('',#12112,0.14635);
#10544=CYLINDRICAL_SURFACE('',#12113,0.14635);
#10545=CYLINDRICAL_SURFACE('',#12114,0.14635);
#10546=CYLINDRICAL_SURFACE('',#12115,0.14635);
#10547=CYLINDRICAL_SURFACE('',#12116,0.14635);
#10548=CYLINDRICAL_SURFACE('',#12117,0.14635);
#10549=CYLINDRICAL_SURFACE('',#12118,0.14635);
#10550=CYLINDRICAL_SURFACE('',#12119,0.117775);
#10551=CYLINDRICAL_SURFACE('',#12121,0.117775);
#10552=CYLINDRICAL_SURFACE('',#12122,0.117775);
#10553=CYLINDRICAL_SURFACE('',#12123,0.117775);
#10554=CYLINDRICAL_SURFACE('',#12124,0.117775);
#10555=CYLINDRICAL_SURFACE('',#12125,0.117775);
#10556=CYLINDRICAL_SURFACE('',#12126,0.117775);
#10557=CYLINDRICAL_SURFACE('',#12127,0.117775);
#10558=CYLINDRICAL_SURFACE('',#12128,0.117775);
#10559=CYLINDRICAL_SURFACE('',#12129,0.117775);
#10560=CYLINDRICAL_SURFACE('',#12133,0.117775);
#10561=CYLINDRICAL_SURFACE('',#12135,0.14635);
#10562=CYLINDRICAL_SURFACE('',#12145,0.3);
#10563=CYLINDRICAL_SURFACE('',#12150,0.14635);
#10564=CYLINDRICAL_SURFACE('',#12152,0.14635);
#10565=CYLINDRICAL_SURFACE('',#12153,0.14635);
#10566=CYLINDRICAL_SURFACE('',#12154,0.14635);
#10567=CYLINDRICAL_SURFACE('',#12155,0.14635);
#10568=CYLINDRICAL_SURFACE('',#12156,0.14635);
#10569=CYLINDRICAL_SURFACE('',#12157,0.14635);
#10570=CYLINDRICAL_SURFACE('',#12158,0.14635);
#10571=CYLINDRICAL_SURFACE('',#12159,0.14635);
#10572=CYLINDRICAL_SURFACE('',#12160,0.14635);
#10573=CYLINDRICAL_SURFACE('',#12161,0.14635);
#10574=CYLINDRICAL_SURFACE('',#12162,0.14635);
#10575=CYLINDRICAL_SURFACE('',#12163,0.14635);
#10576=CYLINDRICAL_SURFACE('',#12164,0.14635);
#10577=CYLINDRICAL_SURFACE('',#12165,0.14635);
#10578=CYLINDRICAL_SURFACE('',#12166,0.14635);
#10579=CYLINDRICAL_SURFACE('',#12167,0.14635);
#10580=CYLINDRICAL_SURFACE('',#12168,0.14635);
#10581=CYLINDRICAL_SURFACE('',#12169,0.117775);
#10582=CYLINDRICAL_SURFACE('',#12171,0.117775);
#10583=CYLINDRICAL_SURFACE('',#12172,0.117775);
#10584=CYLINDRICAL_SURFACE('',#12173,0.117775);
#10585=CYLINDRICAL_SURFACE('',#12174,0.117775);
#10586=CYLINDRICAL_SURFACE('',#12175,0.117775);
#10587=CYLINDRICAL_SURFACE('',#12176,0.117775);
#10588=CYLINDRICAL_SURFACE('',#12177,0.117775);
#10589=CYLINDRICAL_SURFACE('',#12178,0.117775);
#10590=CYLINDRICAL_SURFACE('',#12179,0.117775);
#10591=CYLINDRICAL_SURFACE('',#12180,0.117775);
#10592=CYLINDRICAL_SURFACE('',#12181,0.117775);
#10593=CYLINDRICAL_SURFACE('',#12182,0.117775);
#10594=CYLINDRICAL_SURFACE('',#12183,0.117775);
#10595=CYLINDRICAL_SURFACE('',#12184,0.117775);
#10596=CYLINDRICAL_SURFACE('',#12185,0.117775);
#10597=CYLINDRICAL_SURFACE('',#12186,0.117775);
#10598=CYLINDRICAL_SURFACE('',#12187,0.117775);
#10599=CYLINDRICAL_SURFACE('',#12191,0.117775);
#10600=CYLINDRICAL_SURFACE('',#12193,0.14635);
#10601=CYLINDRICAL_SURFACE('',#12203,0.3);
#10602=CYLINDRICAL_SURFACE('',#12208,0.4925);
#10603=CYLINDRICAL_SURFACE('',#12210,0.4925);
#10604=CYLINDRICAL_SURFACE('',#12211,0.40705);
#10605=CYLINDRICAL_SURFACE('',#12213,0.40705);
#10606=CYLINDRICAL_SURFACE('',#12217,0.40705);
#10607=CYLINDRICAL_SURFACE('',#12219,0.4925);
#10608=CYLINDRICAL_SURFACE('',#12229,0.6);
#10609=ADVANCED_FACE('',(#484),#10183,.F.);
#10610=ADVANCED_FACE('',(#485),#10184,.F.);
#10611=ADVANCED_FACE('',(#486),#10185,.F.);
#10612=ADVANCED_FACE('',(#487),#10186,.F.);
#10613=ADVANCED_FACE('',(#488),#10187,.F.);
#10614=ADVANCED_FACE('',(#489),#10188,.F.);
#10615=ADVANCED_FACE('',(#490),#10189,.F.);
#10616=ADVANCED_FACE('',(#491),#10190,.F.);
#10617=ADVANCED_FACE('',(#492),#10191,.F.);
#10618=ADVANCED_FACE('',(#493),#10192,.F.);
#10619=ADVANCED_FACE('',(#494),#10193,.F.);
#10620=ADVANCED_FACE('',(#495),#10194,.F.);
#10621=ADVANCED_FACE('',(#496),#10195,.F.);
#10622=ADVANCED_FACE('',(#497),#10196,.F.);
#10623=ADVANCED_FACE('',(#498),#10197,.F.);
#10624=ADVANCED_FACE('',(#499),#10198,.F.);
#10625=ADVANCED_FACE('',(#500),#10199,.F.);
#10626=ADVANCED_FACE('',(#501),#10200,.F.);
#10627=ADVANCED_FACE('',(#502),#10201,.F.);
#10628=ADVANCED_FACE('',(#503),#10202,.F.);
#10629=ADVANCED_FACE('',(#504),#10203,.F.);
#10630=ADVANCED_FACE('',(#505),#10204,.F.);
#10631=ADVANCED_FACE('',(#506),#10205,.F.);
#10632=ADVANCED_FACE('',(#507),#10206,.F.);
#10633=ADVANCED_FACE('',(#508),#10207,.F.);
#10634=ADVANCED_FACE('',(#509),#10208,.F.);
#10635=ADVANCED_FACE('',(#510),#10209,.F.);
#10636=ADVANCED_FACE('',(#511),#10210,.F.);
#10637=ADVANCED_FACE('',(#512),#10211,.F.);
#10638=ADVANCED_FACE('',(#513),#10212,.F.);
#10639=ADVANCED_FACE('',(#514),#10213,.F.);
#10640=ADVANCED_FACE('',(#515),#10214,.F.);
#10641=ADVANCED_FACE('',(#516),#10215,.F.);
#10642=ADVANCED_FACE('',(#517),#10216,.F.);
#10643=ADVANCED_FACE('',(#518),#10217,.F.);
#10644=ADVANCED_FACE('',(#519),#10218,.F.);
#10645=ADVANCED_FACE('',(#520),#10219,.F.);
#10646=ADVANCED_FACE('',(#521),#10220,.F.);
#10647=ADVANCED_FACE('',(#522),#10221,.F.);
#10648=ADVANCED_FACE('',(#523),#10222,.F.);
#10649=ADVANCED_FACE('',(#524),#10223,.F.);
#10650=ADVANCED_FACE('',(#525),#10224,.F.);
#10651=ADVANCED_FACE('',(#526),#10225,.F.);
#10652=ADVANCED_FACE('',(#527),#10226,.F.);
#10653=ADVANCED_FACE('',(#528),#10227,.F.);
#10654=ADVANCED_FACE('',(#529),#10228,.F.);
#10655=ADVANCED_FACE('',(#530),#10229,.F.);
#10656=ADVANCED_FACE('',(#531),#10230,.F.);
#10657=ADVANCED_FACE('',(#532),#10231,.F.);
#10658=ADVANCED_FACE('',(#533),#10232,.F.);
#10659=ADVANCED_FACE('',(#534),#10233,.F.);
#10660=ADVANCED_FACE('',(#535),#10234,.F.);
#10661=ADVANCED_FACE('',(#536),#10235,.F.);
#10662=ADVANCED_FACE('',(#537),#10236,.F.);
#10663=ADVANCED_FACE('',(#538),#10237,.F.);
#10664=ADVANCED_FACE('',(#539),#10238,.F.);
#10665=ADVANCED_FACE('',(#540),#10239,.F.);
#10666=ADVANCED_FACE('',(#541),#10240,.F.);
#10667=ADVANCED_FACE('',(#542),#10241,.F.);
#10668=ADVANCED_FACE('',(#543),#10242,.F.);
#10669=ADVANCED_FACE('',(#544),#10243,.F.);
#10670=ADVANCED_FACE('',(#545),#10244,.F.);
#10671=ADVANCED_FACE('',(#546),#10245,.F.);
#10672=ADVANCED_FACE('',(#547),#10246,.F.);
#10673=ADVANCED_FACE('',(#548),#10247,.F.);
#10674=ADVANCED_FACE('',(#549),#10248,.F.);
#10675=ADVANCED_FACE('',(#550),#10249,.F.);
#10676=ADVANCED_FACE('',(#551),#10250,.F.);
#10677=ADVANCED_FACE('',(#552),#10251,.F.);
#10678=ADVANCED_FACE('',(#553),#10252,.F.);
#10679=ADVANCED_FACE('',(#554),#10253,.F.);
#10680=ADVANCED_FACE('',(#555),#10254,.F.);
#10681=ADVANCED_FACE('',(#556),#10255,.F.);
#10682=ADVANCED_FACE('',(#557),#10256,.F.);
#10683=ADVANCED_FACE('',(#558),#10257,.F.);
#10684=ADVANCED_FACE('',(#559),#10258,.F.);
#10685=ADVANCED_FACE('',(#560),#10259,.F.);
#10686=ADVANCED_FACE('',(#561),#10260,.F.);
#10687=ADVANCED_FACE('',(#562),#10261,.F.);
#10688=ADVANCED_FACE('',(#563),#10262,.F.);
#10689=ADVANCED_FACE('',(#564),#10263,.F.);
#10690=ADVANCED_FACE('',(#565),#10264,.F.);
#10691=ADVANCED_FACE('',(#566),#10265,.F.);
#10692=ADVANCED_FACE('',(#567),#10266,.F.);
#10693=ADVANCED_FACE('',(#568),#10267,.F.);
#10694=ADVANCED_FACE('',(#569),#10268,.F.);
#10695=ADVANCED_FACE('',(#570),#10269,.F.);
#10696=ADVANCED_FACE('',(#571),#10270,.F.);
#10697=ADVANCED_FACE('',(#572),#10271,.F.);
#10698=ADVANCED_FACE('',(#573),#10272,.F.);
#10699=ADVANCED_FACE('',(#574),#10273,.F.);
#10700=ADVANCED_FACE('',(#575),#10274,.F.);
#10701=ADVANCED_FACE('',(#576),#10275,.F.);
#10702=ADVANCED_FACE('',(#577),#10276,.F.);
#10703=ADVANCED_FACE('',(#578),#10277,.F.);
#10704=ADVANCED_FACE('',(#579),#10278,.F.);
#10705=ADVANCED_FACE('',(#580),#10279,.F.);
#10706=ADVANCED_FACE('',(#581),#10280,.F.);
#10707=ADVANCED_FACE('',(#582),#10281,.F.);
#10708=ADVANCED_FACE('',(#583),#10282,.F.);
#10709=ADVANCED_FACE('',(#584),#10283,.F.);
#10710=ADVANCED_FACE('',(#585,#258),#331,.F.);
#10711=ADVANCED_FACE('',(#586),#10284,.F.);
#10712=ADVANCED_FACE('',(#587),#10285,.F.);
#10713=ADVANCED_FACE('',(#588,#259),#332,.F.);
#10714=ADVANCED_FACE('',(#589),#10286,.F.);
#10715=ADVANCED_FACE('',(#590),#10287,.F.);
#10716=ADVANCED_FACE('',(#591),#333,.T.);
#10717=ADVANCED_FACE('',(#592),#10288,.F.);
#10718=ADVANCED_FACE('',(#593),#224,.F.);
#10719=ADVANCED_FACE('',(#594),#225,.F.);
#10720=ADVANCED_FACE('',(#595),#10289,.F.);
#10721=ADVANCED_FACE('',(#596),#334,.T.);
#10722=ADVANCED_FACE('',(#597),#10290,.F.);
#10723=ADVANCED_FACE('',(#598),#226,.F.);
#10724=ADVANCED_FACE('',(#599),#227,.F.);
#10725=ADVANCED_FACE('',(#600),#10291,.F.);
#10726=ADVANCED_FACE('',(#601),#335,.T.);
#10727=ADVANCED_FACE('',(#602),#10292,.F.);
#10728=ADVANCED_FACE('',(#603),#228,.F.);
#10729=ADVANCED_FACE('',(#604),#229,.F.);
#10730=ADVANCED_FACE('',(#605),#10293,.F.);
#10731=ADVANCED_FACE('',(#606),#336,.T.);
#10732=ADVANCED_FACE('',(#607),#10294,.F.);
#10733=ADVANCED_FACE('',(#608),#230,.F.);
#10734=ADVANCED_FACE('',(#609),#231,.F.);
#10735=ADVANCED_FACE('',(#610),#10295,.F.);
#10736=ADVANCED_FACE('',(#611),#337,.F.);
#10737=ADVANCED_FACE('',(#612),#338,.F.);
#10738=ADVANCED_FACE('',(#613),#339,.F.);
#10739=ADVANCED_FACE('',(#614),#340,.F.);
#10740=ADVANCED_FACE('',(#615),#10296,.F.);
#10741=ADVANCED_FACE('',(#616),#10297,.F.);
#10742=ADVANCED_FACE('',(#617),#341,.T.);
#10743=ADVANCED_FACE('',(#618),#342,.T.);
#10744=ADVANCED_FACE('',(#619),#343,.T.);
#10745=ADVANCED_FACE('',(#620,#260),#344,.T.);
#10746=ADVANCED_FACE('',(#621),#345,.T.);
#10747=ADVANCED_FACE('',(#622),#346,.T.);
#10748=ADVANCED_FACE('',(#623),#347,.T.);
#10749=ADVANCED_FACE('',(#624,#261),#348,.T.);
#10750=ADVANCED_FACE('',(#625),#10298,.F.);
#10751=ADVANCED_FACE('',(#626),#10299,.T.);
#10752=ADVANCED_FACE('',(#627,#262),#349,.T.);
#10753=ADVANCED_FACE('',(#628,#263,#264,#265),#350,.F.);
#10754=ADVANCED_FACE('',(#629),#10300,.F.);
#10755=ADVANCED_FACE('',(#630),#351,.F.);
#10756=ADVANCED_FACE('',(#631),#10301,.F.);
#10757=ADVANCED_FACE('',(#632),#352,.F.);
#10758=ADVANCED_FACE('',(#633),#10302,.F.);
#10759=ADVANCED_FACE('',(#634),#353,.F.);
#10760=ADVANCED_FACE('',(#635,#266),#354,.F.);
#10761=ADVANCED_FACE('',(#636),#10303,.F.);
#10762=ADVANCED_FACE('',(#637),#355,.F.);
#10763=ADVANCED_FACE('',(#638),#356,.T.);
#10764=ADVANCED_FACE('',(#639),#357,.T.);
#10765=ADVANCED_FACE('',(#640,#267),#358,.T.);
#10766=ADVANCED_FACE('',(#641),#359,.T.);
#10767=ADVANCED_FACE('',(#642,#268,#269,#270,#271,#272),#360,.T.);
#10768=ADVANCED_FACE('',(#643,#273,#274,#275,#276),#361,.F.);
#10769=ADVANCED_FACE('',(#644),#10304,.F.);
#10770=ADVANCED_FACE('',(#645),#10305,.F.);
#10771=ADVANCED_FACE('',(#646),#10306,.F.);
#10772=ADVANCED_FACE('',(#647),#10307,.F.);
#10773=ADVANCED_FACE('',(#648),#10308,.F.);
#10774=ADVANCED_FACE('',(#649),#10309,.F.);
#10775=ADVANCED_FACE('',(#650),#10310,.F.);
#10776=ADVANCED_FACE('',(#651),#10311,.F.);
#10777=ADVANCED_FACE('',(#652),#10312,.F.);
#10778=ADVANCED_FACE('',(#653),#10313,.F.);
#10779=ADVANCED_FACE('',(#654),#10314,.F.);
#10780=ADVANCED_FACE('',(#655),#10315,.F.);
#10781=ADVANCED_FACE('',(#656),#10316,.F.);
#10782=ADVANCED_FACE('',(#657),#10317,.F.);
#10783=ADVANCED_FACE('',(#658),#362,.T.);
#10784=ADVANCED_FACE('',(#659),#363,.T.);
#10785=ADVANCED_FACE('',(#660),#364,.T.);
#10786=ADVANCED_FACE('',(#661),#365,.T.);
#10787=ADVANCED_FACE('',(#662),#366,.T.);
#10788=ADVANCED_FACE('',(#663),#367,.T.);
#10789=ADVANCED_FACE('',(#664),#368,.T.);
#10790=ADVANCED_FACE('',(#665),#369,.T.);
#10791=ADVANCED_FACE('',(#666,#277),#370,.T.);
#10792=ADVANCED_FACE('',(#667),#371,.T.);
#10793=ADVANCED_FACE('',(#668),#10318,.F.);
#10794=ADVANCED_FACE('',(#669),#232,.F.);
#10795=ADVANCED_FACE('',(#670),#233,.F.);
#10796=ADVANCED_FACE('',(#671),#10319,.F.);
#10797=ADVANCED_FACE('',(#672),#234,.F.);
#10798=ADVANCED_FACE('',(#673),#235,.F.);
#10799=ADVANCED_FACE('',(#674),#10320,.F.);
#10800=ADVANCED_FACE('',(#675,#278),#372,.F.);
#10801=ADVANCED_FACE('',(#676),#10321,.F.);
#10802=ADVANCED_FACE('',(#677,#279),#373,.F.);
#10803=ADVANCED_FACE('',(#678),#10322,.F.);
#10804=ADVANCED_FACE('',(#679),#10323,.T.);
#10805=ADVANCED_FACE('',(#680),#374,.F.);
#10806=ADVANCED_FACE('',(#681,#280),#375,.T.);
#10807=ADVANCED_FACE('',(#682,#281,#282,#283,#284,#285),#376,.T.);
#10808=ADVANCED_FACE('',(#683),#10324,.T.);
#10809=ADVANCED_FACE('',(#684),#10325,.F.);
#10810=ADVANCED_FACE('',(#685,#286),#377,.F.);
#10811=ADVANCED_FACE('',(#686),#10326,.F.);
#10812=ADVANCED_FACE('',(#687,#287),#378,.F.);
#10813=ADVANCED_FACE('',(#688),#10327,.F.);
#10814=ADVANCED_FACE('',(#689,#288),#379,.F.);
#10815=ADVANCED_FACE('',(#690),#10328,.T.);
#10816=ADVANCED_FACE('',(#691),#10329,.T.);
#10817=ADVANCED_FACE('',(#692),#10330,.F.);
#10818=ADVANCED_FACE('',(#693),#10331,.F.);
#10819=ADVANCED_FACE('',(#694),#10332,.F.);
#10820=ADVANCED_FACE('',(#695),#10333,.F.);
#10821=ADVANCED_FACE('',(#696,#289),#10334,.F.);
#10822=ADVANCED_FACE('',(#697),#380,.T.);
#10823=ADVANCED_FACE('',(#698),#381,.T.);
#10824=ADVANCED_FACE('',(#699),#382,.T.);
#10825=ADVANCED_FACE('',(#700),#383,.T.);
#10826=ADVANCED_FACE('',(#701,#290,#291,#292,#293,#294),#384,.F.);
#10827=ADVANCED_FACE('',(#702,#295),#385,.T.);
#10828=ADVANCED_FACE('',(#703),#10335,.T.);
#10829=ADVANCED_FACE('',(#704,#296),#386,.F.);
#10830=ADVANCED_FACE('',(#705),#10336,.F.);
#10831=ADVANCED_FACE('',(#706),#10337,.T.);
#10832=ADVANCED_FACE('',(#707,#297),#387,.T.);
#10833=ADVANCED_FACE('',(#708),#10338,.F.);
#10834=ADVANCED_FACE('',(#709),#10339,.F.);
#10835=ADVANCED_FACE('',(#710),#10340,.F.);
#10836=ADVANCED_FACE('',(#711),#10341,.F.);
#10837=ADVANCED_FACE('',(#712),#10342,.F.);
#10838=ADVANCED_FACE('',(#713),#10343,.F.);
#10839=ADVANCED_FACE('',(#714),#10344,.F.);
#10840=ADVANCED_FACE('',(#715),#10345,.F.);
#10841=ADVANCED_FACE('',(#716),#10346,.F.);
#10842=ADVANCED_FACE('',(#717),#10347,.F.);
#10843=ADVANCED_FACE('',(#718),#10348,.F.);
#10844=ADVANCED_FACE('',(#719),#10349,.F.);
#10845=ADVANCED_FACE('',(#720),#10350,.F.);
#10846=ADVANCED_FACE('',(#721),#10351,.F.);
#10847=ADVANCED_FACE('',(#722),#10352,.F.);
#10848=ADVANCED_FACE('',(#723),#10353,.F.);
#10849=ADVANCED_FACE('',(#724),#10354,.F.);
#10850=ADVANCED_FACE('',(#725),#10355,.F.);
#10851=ADVANCED_FACE('',(#726),#10356,.F.);
#10852=ADVANCED_FACE('',(#727),#10357,.F.);
#10853=ADVANCED_FACE('',(#728),#10358,.F.);
#10854=ADVANCED_FACE('',(#729),#10359,.F.);
#10855=ADVANCED_FACE('',(#730),#10360,.F.);
#10856=ADVANCED_FACE('',(#731),#10361,.F.);
#10857=ADVANCED_FACE('',(#732),#10362,.F.);
#10858=ADVANCED_FACE('',(#733),#10363,.F.);
#10859=ADVANCED_FACE('',(#734),#10364,.F.);
#10860=ADVANCED_FACE('',(#735),#10365,.F.);
#10861=ADVANCED_FACE('',(#736),#10366,.F.);
#10862=ADVANCED_FACE('',(#737),#10367,.F.);
#10863=ADVANCED_FACE('',(#738),#10368,.F.);
#10864=ADVANCED_FACE('',(#739),#10369,.F.);
#10865=ADVANCED_FACE('',(#740),#10370,.F.);
#10866=ADVANCED_FACE('',(#741),#10371,.F.);
#10867=ADVANCED_FACE('',(#742),#10372,.F.);
#10868=ADVANCED_FACE('',(#743),#10373,.F.);
#10869=ADVANCED_FACE('',(#744),#10374,.F.);
#10870=ADVANCED_FACE('',(#745),#10375,.F.);
#10871=ADVANCED_FACE('',(#746),#10376,.F.);
#10872=ADVANCED_FACE('',(#747),#10377,.F.);
#10873=ADVANCED_FACE('',(#748),#10378,.F.);
#10874=ADVANCED_FACE('',(#749),#10379,.F.);
#10875=ADVANCED_FACE('',(#750),#10380,.F.);
#10876=ADVANCED_FACE('',(#751),#10381,.F.);
#10877=ADVANCED_FACE('',(#752),#10382,.F.);
#10878=ADVANCED_FACE('',(#753),#10383,.F.);
#10879=ADVANCED_FACE('',(#754),#10384,.F.);
#10880=ADVANCED_FACE('',(#755),#10385,.F.);
#10881=ADVANCED_FACE('',(#756),#10386,.F.);
#10882=ADVANCED_FACE('',(#757),#10387,.F.);
#10883=ADVANCED_FACE('',(#758),#10388,.F.);
#10884=ADVANCED_FACE('',(#759),#10389,.F.);
#10885=ADVANCED_FACE('',(#760),#10390,.F.);
#10886=ADVANCED_FACE('',(#761),#10391,.F.);
#10887=ADVANCED_FACE('',(#762),#10392,.F.);
#10888=ADVANCED_FACE('',(#763),#10393,.F.);
#10889=ADVANCED_FACE('',(#764),#10394,.F.);
#10890=ADVANCED_FACE('',(#765),#10395,.F.);
#10891=ADVANCED_FACE('',(#766),#236,.F.);
#10892=ADVANCED_FACE('',(#767),#237,.F.);
#10893=ADVANCED_FACE('',(#768,#298,#299),#388,.F.);
#10894=ADVANCED_FACE('',(#769),#10396,.F.);
#10895=ADVANCED_FACE('',(#770),#238,.F.);
#10896=ADVANCED_FACE('',(#771),#239,.F.);
#10897=ADVANCED_FACE('',(#772),#10397,.F.);
#10898=ADVANCED_FACE('',(#773),#10398,.F.);
#10899=ADVANCED_FACE('',(#774),#389,.T.);
#10900=ADVANCED_FACE('',(#775),#10399,.F.);
#10901=ADVANCED_FACE('',(#776),#240,.F.);
#10902=ADVANCED_FACE('',(#777),#241,.F.);
#10903=ADVANCED_FACE('',(#778),#10400,.F.);
#10904=ADVANCED_FACE('',(#779),#390,.F.);
#10905=ADVANCED_FACE('',(#780),#152,.F.);
#10906=ADVANCED_FACE('',(#781),#10401,.T.);
#10907=ADVANCED_FACE('',(#782),#153,.F.);
#10908=ADVANCED_FACE('',(#783),#10402,.T.);
#10909=ADVANCED_FACE('',(#784,#300),#391,.T.);
#10910=ADVANCED_FACE('',(#785,#301),#392,.F.);
#10911=ADVANCED_FACE('',(#786),#10403,.T.);
#10912=ADVANCED_FACE('',(#787),#10404,.T.);
#10913=ADVANCED_FACE('',(#788),#393,.T.);
#10914=ADVANCED_FACE('',(#789),#394,.T.);
#10915=ADVANCED_FACE('',(#790),#395,.T.);
#10916=ADVANCED_FACE('',(#791),#396,.T.);
#10917=ADVANCED_FACE('',(#792),#397,.T.);
#10918=ADVANCED_FACE('',(#793),#10405,.T.);
#10919=ADVANCED_FACE('',(#794),#10406,.T.);
#10920=ADVANCED_FACE('',(#795,#302),#398,.T.);
#10921=ADVANCED_FACE('',(#796,#303,#304,#305),#399,.T.);
#10922=ADVANCED_FACE('',(#797),#154,.T.);
#10923=ADVANCED_FACE('',(#798),#10407,.T.);
#10924=ADVANCED_FACE('',(#799,#306),#400,.T.);
#10925=ADVANCED_FACE('',(#800),#155,.T.);
#10926=ADVANCED_FACE('',(#801,#307),#401,.F.);
#10927=ADVANCED_FACE('',(#802,#308),#402,.F.);
#10928=ADVANCED_FACE('',(#803),#10408,.F.);
#10929=ADVANCED_FACE('',(#804,#309),#403,.F.);
#10930=ADVANCED_FACE('',(#805),#10409,.F.);
#10931=ADVANCED_FACE('',(#806),#10410,.F.);
#10932=ADVANCED_FACE('',(#807),#10411,.T.);
#10933=ADVANCED_FACE('',(#808,#310),#404,.F.);
#10934=ADVANCED_FACE('',(#809),#10412,.F.);
#10935=ADVANCED_FACE('',(#810),#10413,.F.);
#10936=ADVANCED_FACE('',(#811),#405,.T.);
#10937=ADVANCED_FACE('',(#812),#406,.T.);
#10938=ADVANCED_FACE('',(#813),#407,.T.);
#10939=ADVANCED_FACE('',(#814),#408,.T.);
#10940=ADVANCED_FACE('',(#815,#311,#312),#409,.T.);
#10941=ADVANCED_FACE('',(#816,#313,#314),#410,.F.);
#10942=ADVANCED_FACE('',(#817),#242,.T.);
#10943=ADVANCED_FACE('',(#818),#411,.F.);
#10944=ADVANCED_FACE('',(#819),#412,.T.);
#10945=ADVANCED_FACE('',(#820),#10414,.F.);
#10946=ADVANCED_FACE('',(#821),#10415,.F.);
#10947=ADVANCED_FACE('',(#822),#10416,.F.);
#10948=ADVANCED_FACE('',(#823),#10417,.F.);
#10949=ADVANCED_FACE('',(#824),#10418,.F.);
#10950=ADVANCED_FACE('',(#825),#10419,.F.);
#10951=ADVANCED_FACE('',(#826),#10420,.F.);
#10952=ADVANCED_FACE('',(#827),#10421,.F.);
#10953=ADVANCED_FACE('',(#828),#10422,.F.);
#10954=ADVANCED_FACE('',(#829),#10423,.F.);
#10955=ADVANCED_FACE('',(#830),#10424,.F.);
#10956=ADVANCED_FACE('',(#831),#10425,.F.);
#10957=ADVANCED_FACE('',(#832),#10426,.F.);
#10958=ADVANCED_FACE('',(#833),#10427,.F.);
#10959=ADVANCED_FACE('',(#834),#10428,.F.);
#10960=ADVANCED_FACE('',(#835),#10429,.F.);
#10961=ADVANCED_FACE('',(#836),#10430,.F.);
#10962=ADVANCED_FACE('',(#837),#10431,.F.);
#10963=ADVANCED_FACE('',(#838),#10432,.F.);
#10964=ADVANCED_FACE('',(#839),#10433,.F.);
#10965=ADVANCED_FACE('',(#840),#10434,.F.);
#10966=ADVANCED_FACE('',(#841),#10435,.F.);
#10967=ADVANCED_FACE('',(#842),#10436,.F.);
#10968=ADVANCED_FACE('',(#843),#10437,.F.);
#10969=ADVANCED_FACE('',(#844),#10438,.F.);
#10970=ADVANCED_FACE('',(#845),#10439,.F.);
#10971=ADVANCED_FACE('',(#846),#10440,.F.);
#10972=ADVANCED_FACE('',(#847),#10441,.F.);
#10973=ADVANCED_FACE('',(#848),#10442,.F.);
#10974=ADVANCED_FACE('',(#849),#10443,.F.);
#10975=ADVANCED_FACE('',(#850),#10444,.F.);
#10976=ADVANCED_FACE('',(#851),#10445,.F.);
#10977=ADVANCED_FACE('',(#852),#10446,.F.);
#10978=ADVANCED_FACE('',(#853),#10447,.F.);
#10979=ADVANCED_FACE('',(#854),#10448,.F.);
#10980=ADVANCED_FACE('',(#855),#10449,.F.);
#10981=ADVANCED_FACE('',(#856),#10450,.F.);
#10982=ADVANCED_FACE('',(#857),#10451,.F.);
#10983=ADVANCED_FACE('',(#858),#10452,.F.);
#10984=ADVANCED_FACE('',(#859),#10453,.F.);
#10985=ADVANCED_FACE('',(#860),#10454,.F.);
#10986=ADVANCED_FACE('',(#861),#10455,.F.);
#10987=ADVANCED_FACE('',(#862),#10456,.F.);
#10988=ADVANCED_FACE('',(#863),#10457,.F.);
#10989=ADVANCED_FACE('',(#864),#10458,.F.);
#10990=ADVANCED_FACE('',(#865),#10459,.F.);
#10991=ADVANCED_FACE('',(#866),#10460,.F.);
#10992=ADVANCED_FACE('',(#867),#10461,.F.);
#10993=ADVANCED_FACE('',(#868),#10462,.F.);
#10994=ADVANCED_FACE('',(#869),#10463,.F.);
#10995=ADVANCED_FACE('',(#870),#10464,.F.);
#10996=ADVANCED_FACE('',(#871),#10465,.F.);
#10997=ADVANCED_FACE('',(#872),#10466,.F.);
#10998=ADVANCED_FACE('',(#873),#10467,.F.);
#10999=ADVANCED_FACE('',(#874),#10468,.F.);
#11000=ADVANCED_FACE('',(#875),#10469,.F.);
#11001=ADVANCED_FACE('',(#876),#10470,.F.);
#11002=ADVANCED_FACE('',(#877),#10471,.F.);
#11003=ADVANCED_FACE('',(#878),#10472,.F.);
#11004=ADVANCED_FACE('',(#879),#10473,.F.);
#11005=ADVANCED_FACE('',(#880),#10474,.F.);
#11006=ADVANCED_FACE('',(#881),#413,.T.);
#11007=ADVANCED_FACE('',(#882),#10475,.F.);
#11008=ADVANCED_FACE('',(#883),#243,.F.);
#11009=ADVANCED_FACE('',(#884),#244,.F.);
#11010=ADVANCED_FACE('',(#885),#10476,.F.);
#11011=ADVANCED_FACE('',(#886),#414,.F.);
#11012=ADVANCED_FACE('',(#887),#415,.F.);
#11013=ADVANCED_FACE('',(#888),#10477,.F.);
#11014=ADVANCED_FACE('',(#889),#245,.F.);
#11015=ADVANCED_FACE('',(#890),#246,.F.);
#11016=ADVANCED_FACE('',(#891),#10478,.F.);
#11017=ADVANCED_FACE('',(#892),#416,.F.);
#11018=ADVANCED_FACE('',(#893),#417,.T.);
#11019=ADVANCED_FACE('',(#894),#418,.T.);
#11020=ADVANCED_FACE('',(#895),#419,.T.);
#11021=ADVANCED_FACE('',(#896),#420,.T.);
#11022=ADVANCED_FACE('',(#897,#315),#421,.T.);
#11023=ADVANCED_FACE('',(#898,#316),#422,.F.);
#11024=ADVANCED_FACE('',(#899),#10479,.F.);
#11025=ADVANCED_FACE('',(#900),#10480,.F.);
#11026=ADVANCED_FACE('',(#901),#10481,.F.);
#11027=ADVANCED_FACE('',(#902),#10482,.F.);
#11028=ADVANCED_FACE('',(#903),#10483,.F.);
#11029=ADVANCED_FACE('',(#904),#10484,.F.);
#11030=ADVANCED_FACE('',(#905),#10485,.F.);
#11031=ADVANCED_FACE('',(#906),#10486,.F.);
#11032=ADVANCED_FACE('',(#907),#10487,.F.);
#11033=ADVANCED_FACE('',(#908),#10488,.F.);
#11034=ADVANCED_FACE('',(#909),#10489,.F.);
#11035=ADVANCED_FACE('',(#910),#10490,.F.);
#11036=ADVANCED_FACE('',(#911),#10491,.F.);
#11037=ADVANCED_FACE('',(#912),#10492,.F.);
#11038=ADVANCED_FACE('',(#913),#10493,.F.);
#11039=ADVANCED_FACE('',(#914),#10494,.F.);
#11040=ADVANCED_FACE('',(#915),#10495,.F.);
#11041=ADVANCED_FACE('',(#916),#10496,.F.);
#11042=ADVANCED_FACE('',(#917),#10497,.F.);
#11043=ADVANCED_FACE('',(#918),#10498,.F.);
#11044=ADVANCED_FACE('',(#919),#423,.T.);
#11045=ADVANCED_FACE('',(#920),#10499,.F.);
#11046=ADVANCED_FACE('',(#921),#247,.F.);
#11047=ADVANCED_FACE('',(#922),#248,.F.);
#11048=ADVANCED_FACE('',(#923),#10500,.F.);
#11049=ADVANCED_FACE('',(#924),#424,.F.);
#11050=ADVANCED_FACE('',(#925),#10501,.F.);
#11051=ADVANCED_FACE('',(#926),#425,.T.);
#11052=ADVANCED_FACE('',(#927,#317),#426,.F.);
#11053=ADVANCED_FACE('',(#928),#427,.T.);
#11054=ADVANCED_FACE('',(#929),#428,.T.);
#11055=ADVANCED_FACE('',(#930),#429,.T.);
#11056=ADVANCED_FACE('',(#931),#430,.T.);
#11057=ADVANCED_FACE('',(#932,#318,#319),#431,.T.);
#11058=ADVANCED_FACE('',(#933),#432,.F.);
#11059=ADVANCED_FACE('',(#934),#10502,.F.);
#11060=ADVANCED_FACE('',(#935),#433,.T.);
#11061=ADVANCED_FACE('',(#936),#434,.T.);
#11062=ADVANCED_FACE('',(#937),#435,.T.);
#11063=ADVANCED_FACE('',(#938),#436,.T.);
#11064=ADVANCED_FACE('',(#939,#320),#437,.T.);
#11065=ADVANCED_FACE('',(#940,#321),#438,.F.);
#11066=ADVANCED_FACE('',(#941),#151,.T.);
#11067=ADVANCED_FACE('',(#942,#322),#439,.F.);
#11068=ADVANCED_FACE('',(#943),#10503,.T.);
#11069=ADVANCED_FACE('',(#944),#440,.T.);
#11070=ADVANCED_FACE('',(#945),#10504,.T.);
#11071=ADVANCED_FACE('',(#946),#441,.F.);
#11072=ADVANCED_FACE('',(#947),#249,.T.);
#11073=ADVANCED_FACE('',(#948),#442,.F.);
#11074=ADVANCED_FACE('',(#949),#443,.T.);
#11075=ADVANCED_FACE('',(#950),#10505,.T.);
#11076=ADVANCED_FACE('',(#951),#10506,.T.);
#11077=ADVANCED_FACE('',(#952),#10507,.T.);
#11078=ADVANCED_FACE('',(#953),#10508,.T.);
#11079=ADVANCED_FACE('',(#954),#10509,.T.);
#11080=ADVANCED_FACE('',(#955),#10510,.T.);
#11081=ADVANCED_FACE('',(#956),#10511,.T.);
#11082=ADVANCED_FACE('',(#957),#10512,.T.);
#11083=ADVANCED_FACE('',(#958),#10513,.T.);
#11084=ADVANCED_FACE('',(#959),#10514,.T.);
#11085=ADVANCED_FACE('',(#960),#10515,.T.);
#11086=ADVANCED_FACE('',(#961),#10516,.T.);
#11087=ADVANCED_FACE('',(#962),#10517,.T.);
#11088=ADVANCED_FACE('',(#963),#10518,.T.);
#11089=ADVANCED_FACE('',(#964),#10519,.T.);
#11090=ADVANCED_FACE('',(#965),#10520,.T.);
#11091=ADVANCED_FACE('',(#966),#10521,.T.);
#11092=ADVANCED_FACE('',(#967),#10522,.T.);
#11093=ADVANCED_FACE('',(#968),#10523,.T.);
#11094=ADVANCED_FACE('',(#969),#10524,.T.);
#11095=ADVANCED_FACE('',(#970),#10525,.T.);
#11096=ADVANCED_FACE('',(#971),#10526,.T.);
#11097=ADVANCED_FACE('',(#972),#10527,.T.);
#11098=ADVANCED_FACE('',(#973),#10528,.T.);
#11099=ADVANCED_FACE('',(#974),#10529,.T.);
#11100=ADVANCED_FACE('',(#975),#10530,.T.);
#11101=ADVANCED_FACE('',(#976),#10531,.T.);
#11102=ADVANCED_FACE('',(#977),#10532,.T.);
#11103=ADVANCED_FACE('',(#978),#10533,.T.);
#11104=ADVANCED_FACE('',(#979),#10534,.T.);
#11105=ADVANCED_FACE('',(#980),#10535,.T.);
#11106=ADVANCED_FACE('',(#981),#10536,.T.);
#11107=ADVANCED_FACE('',(#982),#147,.T.);
#11108=ADVANCED_FACE('',(#983),#250,.F.);
#11109=ADVANCED_FACE('',(#984),#10537,.T.);
#11110=ADVANCED_FACE('',(#985),#251,.F.);
#11111=ADVANCED_FACE('',(#986),#10538,.T.);
#11112=ADVANCED_FACE('',(#987),#444,.F.);
#11113=ADVANCED_FACE('',(#988),#445,.F.);
#11114=ADVANCED_FACE('',(#989),#446,.F.);
#11115=ADVANCED_FACE('',(#990),#447,.F.);
#11116=ADVANCED_FACE('',(#991),#448,.F.);
#11117=ADVANCED_FACE('',(#992),#449,.F.);
#11118=ADVANCED_FACE('',(#993),#450,.F.);
#11119=ADVANCED_FACE('',(#994,#323),#451,.T.);
#11120=ADVANCED_FACE('',(#995),#10539,.T.);
#11121=ADVANCED_FACE('',(#996,#324),#452,.F.);
#11122=ADVANCED_FACE('',(#997),#453,.T.);
#11123=ADVANCED_FACE('',(#998),#10540,.T.);
#11124=ADVANCED_FACE('',(#999),#10541,.T.);
#11125=ADVANCED_FACE('',(#1000),#10542,.T.);
#11126=ADVANCED_FACE('',(#1001),#10543,.T.);
#11127=ADVANCED_FACE('',(#1002),#10544,.T.);
#11128=ADVANCED_FACE('',(#1003),#10545,.T.);
#11129=ADVANCED_FACE('',(#1004),#10546,.T.);
#11130=ADVANCED_FACE('',(#1005),#10547,.T.);
#11131=ADVANCED_FACE('',(#1006),#10548,.T.);
#11132=ADVANCED_FACE('',(#1007),#10549,.T.);
#11133=ADVANCED_FACE('',(#1008),#10550,.T.);
#11134=ADVANCED_FACE('',(#1009),#10551,.T.);
#11135=ADVANCED_FACE('',(#1010),#10552,.T.);
#11136=ADVANCED_FACE('',(#1011),#10553,.T.);
#11137=ADVANCED_FACE('',(#1012),#10554,.T.);
#11138=ADVANCED_FACE('',(#1013),#10555,.T.);
#11139=ADVANCED_FACE('',(#1014),#10556,.T.);
#11140=ADVANCED_FACE('',(#1015),#10557,.T.);
#11141=ADVANCED_FACE('',(#1016),#10558,.T.);
#11142=ADVANCED_FACE('',(#1017),#10559,.T.);
#11143=ADVANCED_FACE('',(#1018),#148,.T.);
#11144=ADVANCED_FACE('',(#1019),#252,.F.);
#11145=ADVANCED_FACE('',(#1020),#10560,.T.);
#11146=ADVANCED_FACE('',(#1021),#253,.F.);
#11147=ADVANCED_FACE('',(#1022),#10561,.T.);
#11148=ADVANCED_FACE('',(#1023),#454,.F.);
#11149=ADVANCED_FACE('',(#1024),#455,.F.);
#11150=ADVANCED_FACE('',(#1025),#456,.F.);
#11151=ADVANCED_FACE('',(#1026),#457,.F.);
#11152=ADVANCED_FACE('',(#1027),#458,.F.);
#11153=ADVANCED_FACE('',(#1028),#459,.F.);
#11154=ADVANCED_FACE('',(#1029),#460,.F.);
#11155=ADVANCED_FACE('',(#1030,#325),#461,.T.);
#11156=ADVANCED_FACE('',(#1031),#10562,.T.);
#11157=ADVANCED_FACE('',(#1032,#326),#462,.F.);
#11158=ADVANCED_FACE('',(#1033),#463,.T.);
#11159=ADVANCED_FACE('',(#1034),#10563,.T.);
#11160=ADVANCED_FACE('',(#1035),#10564,.T.);
#11161=ADVANCED_FACE('',(#1036),#10565,.T.);
#11162=ADVANCED_FACE('',(#1037),#10566,.T.);
#11163=ADVANCED_FACE('',(#1038),#10567,.T.);
#11164=ADVANCED_FACE('',(#1039),#10568,.T.);
#11165=ADVANCED_FACE('',(#1040),#10569,.T.);
#11166=ADVANCED_FACE('',(#1041),#10570,.T.);
#11167=ADVANCED_FACE('',(#1042),#10571,.T.);
#11168=ADVANCED_FACE('',(#1043),#10572,.T.);
#11169=ADVANCED_FACE('',(#1044),#10573,.T.);
#11170=ADVANCED_FACE('',(#1045),#10574,.T.);
#11171=ADVANCED_FACE('',(#1046),#10575,.T.);
#11172=ADVANCED_FACE('',(#1047),#10576,.T.);
#11173=ADVANCED_FACE('',(#1048),#10577,.T.);
#11174=ADVANCED_FACE('',(#1049),#10578,.T.);
#11175=ADVANCED_FACE('',(#1050),#10579,.T.);
#11176=ADVANCED_FACE('',(#1051),#10580,.T.);
#11177=ADVANCED_FACE('',(#1052),#10581,.T.);
#11178=ADVANCED_FACE('',(#1053),#10582,.T.);
#11179=ADVANCED_FACE('',(#1054),#10583,.T.);
#11180=ADVANCED_FACE('',(#1055),#10584,.T.);
#11181=ADVANCED_FACE('',(#1056),#10585,.T.);
#11182=ADVANCED_FACE('',(#1057),#10586,.T.);
#11183=ADVANCED_FACE('',(#1058),#10587,.T.);
#11184=ADVANCED_FACE('',(#1059),#10588,.T.);
#11185=ADVANCED_FACE('',(#1060),#10589,.T.);
#11186=ADVANCED_FACE('',(#1061),#10590,.T.);
#11187=ADVANCED_FACE('',(#1062),#10591,.T.);
#11188=ADVANCED_FACE('',(#1063),#10592,.T.);
#11189=ADVANCED_FACE('',(#1064),#10593,.T.);
#11190=ADVANCED_FACE('',(#1065),#10594,.T.);
#11191=ADVANCED_FACE('',(#1066),#10595,.T.);
#11192=ADVANCED_FACE('',(#1067),#10596,.T.);
#11193=ADVANCED_FACE('',(#1068),#10597,.T.);
#11194=ADVANCED_FACE('',(#1069),#10598,.T.);
#11195=ADVANCED_FACE('',(#1070),#149,.T.);
#11196=ADVANCED_FACE('',(#1071),#254,.F.);
#11197=ADVANCED_FACE('',(#1072),#10599,.T.);
#11198=ADVANCED_FACE('',(#1073),#255,.F.);
#11199=ADVANCED_FACE('',(#1074),#10600,.T.);
#11200=ADVANCED_FACE('',(#1075),#464,.F.);
#11201=ADVANCED_FACE('',(#1076),#465,.F.);
#11202=ADVANCED_FACE('',(#1077),#466,.F.);
#11203=ADVANCED_FACE('',(#1078),#467,.F.);
#11204=ADVANCED_FACE('',(#1079),#468,.F.);
#11205=ADVANCED_FACE('',(#1080),#469,.F.);
#11206=ADVANCED_FACE('',(#1081),#470,.F.);
#11207=ADVANCED_FACE('',(#1082,#327),#471,.T.);
#11208=ADVANCED_FACE('',(#1083),#10601,.T.);
#11209=ADVANCED_FACE('',(#1084,#328),#472,.F.);
#11210=ADVANCED_FACE('',(#1085),#473,.T.);
#11211=ADVANCED_FACE('',(#1086),#10602,.T.);
#11212=ADVANCED_FACE('',(#1087),#10603,.T.);
#11213=ADVANCED_FACE('',(#1088),#10604,.T.);
#11214=ADVANCED_FACE('',(#1089),#10605,.T.);
#11215=ADVANCED_FACE('',(#1090),#150,.T.);
#11216=ADVANCED_FACE('',(#1091),#256,.F.);
#11217=ADVANCED_FACE('',(#1092),#10606,.T.);
#11218=ADVANCED_FACE('',(#1093),#257,.F.);
#11219=ADVANCED_FACE('',(#1094),#10607,.T.);
#11220=ADVANCED_FACE('',(#1095),#474,.F.);
#11221=ADVANCED_FACE('',(#1096),#475,.F.);
#11222=ADVANCED_FACE('',(#1097),#476,.F.);
#11223=ADVANCED_FACE('',(#1098),#477,.F.);
#11224=ADVANCED_FACE('',(#1099),#478,.F.);
#11225=ADVANCED_FACE('',(#1100),#479,.F.);
#11226=ADVANCED_FACE('',(#1101),#480,.F.);
#11227=ADVANCED_FACE('',(#1102,#329),#481,.T.);
#11228=ADVANCED_FACE('',(#1103),#10608,.T.);
#11229=ADVANCED_FACE('',(#1104,#330),#482,.F.);
#11230=ADVANCED_FACE('',(#1105),#483,.T.);
#11231=CLOSED_SHELL('',(#10609,#10610,#10611,#10612,#10613,#10614,#10615,
#10616,#10617,#10618,#10619,#10620,#10621,#10622,#10623,#10624,#10625,#10626,
#10627,#10628,#10629,#10630,#10631,#10632,#10633,#10634,#10635,#10636,#10637,
#10638,#10639,#10640,#10641,#10642,#10643,#10644,#10645,#10646,#10647,#10648,
#10649,#10650,#10651,#10652,#10653,#10654,#10655,#10656,#10657,#10658,#10659,
#10660,#10661,#10662,#10663,#10664,#10665,#10666,#10667,#10668,#10669,#10670,
#10671,#10672,#10673,#10674,#10675,#10676,#10677,#10678,#10679,#10680,#10681,
#10682,#10683,#10684,#10685,#10686,#10687,#10688,#10689,#10690,#10691,#10692,
#10693,#10694,#10695,#10696,#10697,#10698,#10699,#10700,#10701,#10702,#10703,
#10704,#10705,#10706,#10707,#10708,#10709,#10710,#10711,#10712,#10713,#10714,
#10715,#10716,#10717,#10718,#10719,#10720,#10721,#10722,#10723,#10724,#10725,
#10726,#10727,#10728,#10729,#10730,#10731,#10732,#10733,#10734,#10735,#10736,
#10737,#10738,#10739,#10740,#10741,#10742,#10743,#10744,#10745,#10746,#10747,
#10748,#10749,#10750,#10751,#10752,#10753,#10754,#10755,#10756,#10757,#10758,
#10759,#10760,#10761,#10762,#10763,#10764,#10765,#10766,#10767,#10768));
#11232=CLOSED_SHELL('',(#10769,#10770,#10771,#10772,#10773,#10774,#10775,
#10776,#10777,#10778,#10779,#10780,#10781,#10782,#10783,#10784,#10785,#10786,
#10787,#10788,#10789,#10790,#10791,#10792,#10793,#10794,#10795,#10796,#10797,
#10798,#10799,#10800,#10801,#10802,#10803,#10804,#10805,#10806,#10807,#10808,
#10809,#10810,#10811,#10812,#10813,#10814,#10815,#10816,#10817,#10818,#10819,
#10820,#10821,#10822,#10823,#10824,#10825,#10826));
#11233=CLOSED_SHELL('',(#10827,#10828,#10829,#10830,#10831,#10832));
#11234=CLOSED_SHELL('',(#10833,#10834,#10835,#10836,#10837,#10838,#10839,
#10840,#10841,#10842,#10843,#10844,#10845,#10846,#10847,#10848,#10849,#10850,
#10851,#10852,#10853,#10854,#10855,#10856,#10857,#10858,#10859,#10860,#10861,
#10862,#10863,#10864,#10865,#10866,#10867,#10868,#10869,#10870,#10871,#10872,
#10873,#10874,#10875,#10876,#10877,#10878,#10879,#10880,#10881,#10882,#10883,
#10884,#10885,#10886,#10887,#10888,#10889,#10890,#10891,#10892,#10893,#10894,
#10895,#10896,#10897,#10898,#10899,#10900,#10901,#10902,#10903,#10904,#10905,
#10906,#10907,#10908,#10909,#10910,#10911,#10912,#10913,#10914,#10915,#10916,
#10917,#10918,#10919,#10920,#10921));
#11235=CLOSED_SHELL('',(#10922,#10923,#10924,#10925,#10926,#10927,#10928,
#10929,#10930,#10931,#10932,#10933));
#11236=CLOSED_SHELL('',(#10934,#10935,#10936,#10937,#10938,#10939,#10940,
#10941));
#11237=CLOSED_SHELL('',(#10942,#10943,#10944));
#11238=CLOSED_SHELL('',(#10945,#10946,#10947,#10948,#10949,#10950,#10951,
#10952,#10953,#10954,#10955,#10956,#10957,#10958,#10959,#10960,#10961,#10962,
#10963,#10964,#10965,#10966,#10967,#10968,#10969,#10970,#10971,#10972,#10973,
#10974,#10975,#10976,#10977,#10978,#10979,#10980,#10981,#10982,#10983,#10984,
#10985,#10986,#10987,#10988,#10989,#10990,#10991,#10992,#10993,#10994,#10995,
#10996,#10997,#10998,#10999,#11000,#11001,#11002,#11003,#11004,#11005,#11006,
#11007,#11008,#11009,#11010,#11011,#11012,#11013,#11014,#11015,#11016,#11017,
#11018,#11019,#11020,#11021,#11022,#11023));
#11239=CLOSED_SHELL('',(#11024,#11025,#11026,#11027,#11028,#11029,#11030,
#11031,#11032,#11033,#11034,#11035,#11036,#11037,#11038,#11039,#11040,#11041,
#11042,#11043,#11044,#11045,#11046,#11047,#11048,#11049,#11050,#11051,#11052,
#11053,#11054,#11055,#11056,#11057,#11058));
#11240=CLOSED_SHELL('',(#11059,#11060,#11061,#11062,#11063,#11064,#11065));
#11241=CLOSED_SHELL('',(#11066));
#11242=CLOSED_SHELL('',(#11067,#11068,#11069,#11070,#11071));
#11243=CLOSED_SHELL('',(#11072,#11073,#11074));
#11244=CLOSED_SHELL('',(#11075,#11076,#11077,#11078,#11079,#11080,#11081,
#11082,#11083,#11084,#11085,#11086,#11087,#11088,#11089,#11090,#11091,#11092,
#11093,#11094,#11095,#11096,#11097,#11098,#11099,#11100,#11101,#11102,#11103,
#11104,#11105,#11106,#11107,#11108,#11109,#11110,#11111,#11112,#11113,#11114,
#11115,#11116,#11117,#11118,#11119,#11120,#11121,#11122));
#11245=CLOSED_SHELL('',(#11123,#11124,#11125,#11126,#11127,#11128,#11129,
#11130,#11131,#11132,#11133,#11134,#11135,#11136,#11137,#11138,#11139,#11140,
#11141,#11142,#11143,#11144,#11145,#11146,#11147,#11148,#11149,#11150,#11151,
#11152,#11153,#11154,#11155,#11156,#11157,#11158));
#11246=CLOSED_SHELL('',(#11159,#11160,#11161,#11162,#11163,#11164,#11165,
#11166,#11167,#11168,#11169,#11170,#11171,#11172,#11173,#11174,#11175,#11176,
#11177,#11178,#11179,#11180,#11181,#11182,#11183,#11184,#11185,#11186,#11187,
#11188,#11189,#11190,#11191,#11192,#11193,#11194,#11195,#11196,#11197,#11198,
#11199,#11200,#11201,#11202,#11203,#11204,#11205,#11206,#11207,#11208,#11209,
#11210));
#11247=CLOSED_SHELL('',(#11211,#11212,#11213,#11214,#11215,#11216,#11217,
#11218,#11219,#11220,#11221,#11222,#11223,#11224,#11225,#11226,#11227,#11228,
#11229,#11230));
#11248=DERIVED_UNIT_ELEMENT(#11282,1.);
#11249=DERIVED_UNIT_ELEMENT(#43982,-3.);
#11250=DERIVED_UNIT_ELEMENT(#11282,1.);
#11251=DERIVED_UNIT_ELEMENT(#43982,-3.);
#11252=DERIVED_UNIT_ELEMENT(#11282,1.);
#11253=DERIVED_UNIT_ELEMENT(#43982,-3.);
#11254=DERIVED_UNIT_ELEMENT(#11282,1.);
#11255=DERIVED_UNIT_ELEMENT(#43982,-3.);
#11256=DERIVED_UNIT_ELEMENT(#11282,1.);
#11257=DERIVED_UNIT_ELEMENT(#43982,-3.);
#11258=DERIVED_UNIT_ELEMENT(#11282,1.);
#11259=DERIVED_UNIT_ELEMENT(#43982,-3.);
#11260=DERIVED_UNIT_ELEMENT(#11282,1.);
#11261=DERIVED_UNIT_ELEMENT(#43982,-3.);
#11262=DERIVED_UNIT_ELEMENT(#11282,1.);
#11263=DERIVED_UNIT_ELEMENT(#43982,-3.);
#11264=DERIVED_UNIT_ELEMENT(#11282,1.);
#11265=DERIVED_UNIT_ELEMENT(#43982,-3.);
#11266=DERIVED_UNIT_ELEMENT(#11282,1.);
#11267=DERIVED_UNIT_ELEMENT(#43982,-3.);
#11268=DERIVED_UNIT_ELEMENT(#11282,1.);
#11269=DERIVED_UNIT_ELEMENT(#43982,-3.);
#11270=DERIVED_UNIT_ELEMENT(#11282,1.);
#11271=DERIVED_UNIT_ELEMENT(#43982,-3.);
#11272=DERIVED_UNIT_ELEMENT(#11282,1.);
#11273=DERIVED_UNIT_ELEMENT(#43982,-3.);
#11274=DERIVED_UNIT_ELEMENT(#11282,1.);
#11275=DERIVED_UNIT_ELEMENT(#43982,-3.);
#11276=DERIVED_UNIT_ELEMENT(#11282,1.);
#11277=DERIVED_UNIT_ELEMENT(#43982,-3.);
#11278=DERIVED_UNIT_ELEMENT(#11282,1.);
#11279=DERIVED_UNIT_ELEMENT(#43982,-3.);
#11280=DERIVED_UNIT_ELEMENT(#11282,1.);
#11281=DERIVED_UNIT_ELEMENT(#43982,-3.);
#11282=(
MASS_UNIT()
NAMED_UNIT(*)
SI_UNIT(.KILO.,.GRAM.)
);
#11283=DERIVED_UNIT((#11248,#11249));
#11284=DERIVED_UNIT((#11250,#11251));
#11285=DERIVED_UNIT((#11252,#11253));
#11286=DERIVED_UNIT((#11254,#11255));
#11287=DERIVED_UNIT((#11256,#11257));
#11288=DERIVED_UNIT((#11258,#11259));
#11289=DERIVED_UNIT((#11260,#11261));
#11290=DERIVED_UNIT((#11262,#11263));
#11291=DERIVED_UNIT((#11264,#11265));
#11292=DERIVED_UNIT((#11266,#11267));
#11293=DERIVED_UNIT((#11268,#11269));
#11294=DERIVED_UNIT((#11270,#11271));
#11295=DERIVED_UNIT((#11272,#11273));
#11296=DERIVED_UNIT((#11274,#11275));
#11297=DERIVED_UNIT((#11276,#11277));
#11298=DERIVED_UNIT((#11278,#11279));
#11299=DERIVED_UNIT((#11280,#11281));
#11300=MEASURE_REPRESENTATION_ITEM('density measure',
POSITIVE_RATIO_MEASURE(7850.),#11283);
#11301=MEASURE_REPRESENTATION_ITEM('density measure',
POSITIVE_RATIO_MEASURE(7850.),#11284);
#11302=MEASURE_REPRESENTATION_ITEM('density measure',
POSITIVE_RATIO_MEASURE(1200.),#11285);
#11303=MEASURE_REPRESENTATION_ITEM('density measure',
POSITIVE_RATIO_MEASURE(1425.),#11286);
#11304=MEASURE_REPRESENTATION_ITEM('density measure',
POSITIVE_RATIO_MEASURE(1425.),#11287);
#11305=MEASURE_REPRESENTATION_ITEM('density measure',
POSITIVE_RATIO_MEASURE(8920.),#11288);
#11306=MEASURE_REPRESENTATION_ITEM('density measure',
POSITIVE_RATIO_MEASURE(7850.),#11289);
#11307=MEASURE_REPRESENTATION_ITEM('density measure',
POSITIVE_RATIO_MEASURE(1425.),#11290);
#11308=MEASURE_REPRESENTATION_ITEM('density measure',
POSITIVE_RATIO_MEASURE(8920.),#11291);
#11309=MEASURE_REPRESENTATION_ITEM('density measure',
POSITIVE_RATIO_MEASURE(8920.),#11292);
#11310=MEASURE_REPRESENTATION_ITEM('density measure',
POSITIVE_RATIO_MEASURE(7850.),#11293);
#11311=MEASURE_REPRESENTATION_ITEM('density measure',
POSITIVE_RATIO_MEASURE(7850.),#11294);
#11312=MEASURE_REPRESENTATION_ITEM('density measure',
POSITIVE_RATIO_MEASURE(7850.),#11295);
#11313=MEASURE_REPRESENTATION_ITEM('density measure',
POSITIVE_RATIO_MEASURE(7850.),#11296);
#11314=MEASURE_REPRESENTATION_ITEM('density measure',
POSITIVE_RATIO_MEASURE(7850.),#11297);
#11315=MEASURE_REPRESENTATION_ITEM('density measure',
POSITIVE_RATIO_MEASURE(7850.),#11298);
#11316=MEASURE_REPRESENTATION_ITEM('density measure',
POSITIVE_RATIO_MEASURE(7850.),#11299);
#11317=PROPERTY_DEFINITION_REPRESENTATION(#11402,#11351);
#11318=PROPERTY_DEFINITION_REPRESENTATION(#11403,#11352);
#11319=PROPERTY_DEFINITION_REPRESENTATION(#11404,#11353);
#11320=PROPERTY_DEFINITION_REPRESENTATION(#11405,#11354);
#11321=PROPERTY_DEFINITION_REPRESENTATION(#11406,#11355);
#11322=PROPERTY_DEFINITION_REPRESENTATION(#11407,#11356);
#11323=PROPERTY_DEFINITION_REPRESENTATION(#11408,#11357);
#11324=PROPERTY_DEFINITION_REPRESENTATION(#11409,#11358);
#11325=PROPERTY_DEFINITION_REPRESENTATION(#11410,#11359);
#11326=PROPERTY_DEFINITION_REPRESENTATION(#11411,#11360);
#11327=PROPERTY_DEFINITION_REPRESENTATION(#11412,#11361);
#11328=PROPERTY_DEFINITION_REPRESENTATION(#11413,#11362);
#11329=PROPERTY_DEFINITION_REPRESENTATION(#11414,#11363);
#11330=PROPERTY_DEFINITION_REPRESENTATION(#11415,#11364);
#11331=PROPERTY_DEFINITION_REPRESENTATION(#11416,#11365);
#11332=PROPERTY_DEFINITION_REPRESENTATION(#11417,#11366);
#11333=PROPERTY_DEFINITION_REPRESENTATION(#11418,#11367);
#11334=PROPERTY_DEFINITION_REPRESENTATION(#11419,#11368);
#11335=PROPERTY_DEFINITION_REPRESENTATION(#11420,#11369);
#11336=PROPERTY_DEFINITION_REPRESENTATION(#11421,#11370);
#11337=PROPERTY_DEFINITION_REPRESENTATION(#11422,#11371);
#11338=PROPERTY_DEFINITION_REPRESENTATION(#11423,#11372);
#11339=PROPERTY_DEFINITION_REPRESENTATION(#11424,#11373);
#11340=PROPERTY_DEFINITION_REPRESENTATION(#11425,#11374);
#11341=PROPERTY_DEFINITION_REPRESENTATION(#11426,#11375);
#11342=PROPERTY_DEFINITION_REPRESENTATION(#11427,#11376);
#11343=PROPERTY_DEFINITION_REPRESENTATION(#11428,#11377);
#11344=PROPERTY_DEFINITION_REPRESENTATION(#11429,#11378);
#11345=PROPERTY_DEFINITION_REPRESENTATION(#11430,#11379);
#11346=PROPERTY_DEFINITION_REPRESENTATION(#11431,#11380);
#11347=PROPERTY_DEFINITION_REPRESENTATION(#11432,#11381);
#11348=PROPERTY_DEFINITION_REPRESENTATION(#11433,#11382);
#11349=PROPERTY_DEFINITION_REPRESENTATION(#11434,#11383);
#11350=PROPERTY_DEFINITION_REPRESENTATION(#11435,#11384);
#11351=REPRESENTATION('material name',(#11385),#43963);
#11352=REPRESENTATION('density',(#11300),#43963);
#11353=REPRESENTATION('material name',(#11386),#43964);
#11354=REPRESENTATION('density',(#11301),#43964);
#11355=REPRESENTATION('material name',(#11387),#43965);
#11356=REPRESENTATION('density',(#11302),#43965);
#11357=REPRESENTATION('material name',(#11388),#43966);
#11358=REPRESENTATION('density',(#11303),#43966);
#11359=REPRESENTATION('material name',(#11389),#43967);
#11360=REPRESENTATION('density',(#11304),#43967);
#11361=REPRESENTATION('material name',(#11390),#43968);
#11362=REPRESENTATION('density',(#11305),#43968);
#11363=REPRESENTATION('material name',(#11391),#43969);
#11364=REPRESENTATION('density',(#11306),#43969);
#11365=REPRESENTATION('material name',(#11392),#43970);
#11366=REPRESENTATION('density',(#11307),#43970);
#11367=REPRESENTATION('material name',(#11393),#43971);
#11368=REPRESENTATION('density',(#11308),#43971);
#11369=REPRESENTATION('material name',(#11394),#43972);
#11370=REPRESENTATION('density',(#11309),#43972);
#11371=REPRESENTATION('material name',(#11395),#43973);
#11372=REPRESENTATION('density',(#11310),#43973);
#11373=REPRESENTATION('material name',(#11396),#43974);
#11374=REPRESENTATION('density',(#11311),#43974);
#11375=REPRESENTATION('material name',(#11397),#43975);
#11376=REPRESENTATION('density',(#11312),#43975);
#11377=REPRESENTATION('material name',(#11398),#43976);
#11378=REPRESENTATION('density',(#11313),#43976);
#11379=REPRESENTATION('material name',(#11399),#43977);
#11380=REPRESENTATION('density',(#11314),#43977);
#11381=REPRESENTATION('material name',(#11400),#43978);
#11382=REPRESENTATION('density',(#11315),#43978);
#11383=REPRESENTATION('material name',(#11401),#43979);
#11384=REPRESENTATION('density',(#11316),#43979);
#11385=DESCRIPTIVE_REPRESENTATION_ITEM('Steel','Steel');
#11386=DESCRIPTIVE_REPRESENTATION_ITEM('Steel','Steel');
#11387=DESCRIPTIVE_REPRESENTATION_ITEM('Rubber, Nitrile',
'Rubber, Nitrile');
#11388=DESCRIPTIVE_REPRESENTATION_ITEM('Acetal Resin, White',
'Acetal Resin, White');
#11389=DESCRIPTIVE_REPRESENTATION_ITEM('Acetal Resin, White',
'Acetal Resin, White');
#11390=DESCRIPTIVE_REPRESENTATION_ITEM('Copper, Alloy','Copper, Alloy');
#11391=DESCRIPTIVE_REPRESENTATION_ITEM('Steel','Steel');
#11392=DESCRIPTIVE_REPRESENTATION_ITEM('Acetal Resin, White',
'Acetal Resin, White');
#11393=DESCRIPTIVE_REPRESENTATION_ITEM('Copper, Alloy','Copper, Alloy');
#11394=DESCRIPTIVE_REPRESENTATION_ITEM('Copper, Alloy','Copper, Alloy');
#11395=DESCRIPTIVE_REPRESENTATION_ITEM('Steel','Steel');
#11396=DESCRIPTIVE_REPRESENTATION_ITEM('Steel','Steel');
#11397=DESCRIPTIVE_REPRESENTATION_ITEM('Steel','Steel');
#11398=DESCRIPTIVE_REPRESENTATION_ITEM('Steel','Steel');
#11399=DESCRIPTIVE_REPRESENTATION_ITEM('Steel','Steel');
#11400=DESCRIPTIVE_REPRESENTATION_ITEM('Steel','Steel');
#11401=DESCRIPTIVE_REPRESENTATION_ITEM('Steel','Steel');
#11402=PROPERTY_DEFINITION('material property','material name',#44075);
#11403=PROPERTY_DEFINITION('material property','density of part',#44075);
#11404=PROPERTY_DEFINITION('material property','material name',#44076);
#11405=PROPERTY_DEFINITION('material property','density of part',#44076);
#11406=PROPERTY_DEFINITION('material property','material name',#44077);
#11407=PROPERTY_DEFINITION('material property','density of part',#44077);
#11408=PROPERTY_DEFINITION('material property','material name',#44078);
#11409=PROPERTY_DEFINITION('material property','density of part',#44078);
#11410=PROPERTY_DEFINITION('material property','material name',#44079);
#11411=PROPERTY_DEFINITION('material property','density of part',#44079);
#11412=PROPERTY_DEFINITION('material property','material name',#44080);
#11413=PROPERTY_DEFINITION('material property','density of part',#44080);
#11414=PROPERTY_DEFINITION('material property','material name',#44081);
#11415=PROPERTY_DEFINITION('material property','density of part',#44081);
#11416=PROPERTY_DEFINITION('material property','material name',#44082);
#11417=PROPERTY_DEFINITION('material property','density of part',#44082);
#11418=PROPERTY_DEFINITION('material property','material name',#44083);
#11419=PROPERTY_DEFINITION('material property','density of part',#44083);
#11420=PROPERTY_DEFINITION('material property','material name',#44084);
#11421=PROPERTY_DEFINITION('material property','density of part',#44084);
#11422=PROPERTY_DEFINITION('material property','material name',#44085);
#11423=PROPERTY_DEFINITION('material property','density of part',#44085);
#11424=PROPERTY_DEFINITION('material property','material name',#44086);
#11425=PROPERTY_DEFINITION('material property','density of part',#44086);
#11426=PROPERTY_DEFINITION('material property','material name',#44087);
#11427=PROPERTY_DEFINITION('material property','density of part',#44087);
#11428=PROPERTY_DEFINITION('material property','material name',#44088);
#11429=PROPERTY_DEFINITION('material property','density of part',#44088);
#11430=PROPERTY_DEFINITION('material property','material name',#44089);
#11431=PROPERTY_DEFINITION('material property','density of part',#44089);
#11432=PROPERTY_DEFINITION('material property','material name',#44090);
#11433=PROPERTY_DEFINITION('material property','density of part',#44090);
#11434=PROPERTY_DEFINITION('material property','material name',#44091);
#11435=PROPERTY_DEFINITION('material property','density of part',#44091);
#11436=AXIS2_PLACEMENT_3D('',#14561,#12267,#12268);
#11437=AXIS2_PLACEMENT_3D('',#14562,#12269,#12270);
#11438=AXIS2_PLACEMENT_3D('',#14563,#12271,#12272);
#11439=AXIS2_PLACEMENT_3D('',#14591,#12274,#12275);
#11440=AXIS2_PLACEMENT_3D('',#14602,#12277,#12278);
#11441=AXIS2_PLACEMENT_3D('',#14625,#12279,#12280);
#11442=AXIS2_PLACEMENT_3D('',#14676,#12282,#12283);
#11443=AXIS2_PLACEMENT_3D('',#14724,#12285,#12286);
#11444=AXIS2_PLACEMENT_3D('',#14772,#12288,#12289);
#11445=AXIS2_PLACEMENT_3D('',#14823,#12291,#12292);
#11446=AXIS2_PLACEMENT_3D('',#14871,#12294,#12295);
#11447=AXIS2_PLACEMENT_3D('',#14919,#12297,#12298);
#11448=AXIS2_PLACEMENT_3D('',#14970,#12300,#12301);
#11449=AXIS2_PLACEMENT_3D('',#15021,#12303,#12304);
#11450=AXIS2_PLACEMENT_3D('',#15069,#12306,#12307);
#11451=AXIS2_PLACEMENT_3D('',#15120,#12309,#12310);
#11452=AXIS2_PLACEMENT_3D('',#15139,#12312,#12313);
#11453=AXIS2_PLACEMENT_3D('',#15159,#12314,#12315);
#11454=AXIS2_PLACEMENT_3D('',#15172,#12317,#12318);
#11455=AXIS2_PLACEMENT_3D('',#15181,#12319,#12320);
#11456=AXIS2_PLACEMENT_3D('',#15205,#12322,#12323);
#11457=AXIS2_PLACEMENT_3D('',#15230,#12325,#12326);
#11458=AXIS2_PLACEMENT_3D('',#15255,#12328,#12329);
#11459=AXIS2_PLACEMENT_3D('',#15279,#12331,#12332);
#11460=AXIS2_PLACEMENT_3D('',#15304,#12334,#12335);
#11461=AXIS2_PLACEMENT_3D('',#15328,#12337,#12338);
#11462=AXIS2_PLACEMENT_3D('',#15353,#12340,#12341);
#11463=AXIS2_PLACEMENT_3D('',#15377,#12343,#12344);
#11464=AXIS2_PLACEMENT_3D('',#15402,#12346,#12347);
#11465=AXIS2_PLACEMENT_3D('',#15427,#12349,#12350);
#11466=AXIS2_PLACEMENT_3D('',#15451,#12352,#12353);
#11467=AXIS2_PLACEMENT_3D('',#15462,#12355,#12356);
#11468=AXIS2_PLACEMENT_3D('',#15468,#12357,#12358);
#11469=AXIS2_PLACEMENT_3D('',#15496,#12360,#12361);
#11470=AXIS2_PLACEMENT_3D('',#15507,#12363,#12364);
#11471=AXIS2_PLACEMENT_3D('',#15530,#12365,#12366);
#11472=AXIS2_PLACEMENT_3D('',#15581,#12368,#12369);
#11473=AXIS2_PLACEMENT_3D('',#15629,#12371,#12372);
#11474=AXIS2_PLACEMENT_3D('',#15677,#12374,#12375);
#11475=AXIS2_PLACEMENT_3D('',#15728,#12377,#12378);
#11476=AXIS2_PLACEMENT_3D('',#15776,#12380,#12381);
#11477=AXIS2_PLACEMENT_3D('',#15824,#12383,#12384);
#11478=AXIS2_PLACEMENT_3D('',#15875,#12386,#12387);
#11479=AXIS2_PLACEMENT_3D('',#15926,#12389,#12390);
#11480=AXIS2_PLACEMENT_3D('',#15974,#12392,#12393);
#11481=AXIS2_PLACEMENT_3D('',#16025,#12395,#12396);
#11482=AXIS2_PLACEMENT_3D('',#16044,#12398,#12399);
#11483=AXIS2_PLACEMENT_3D('',#16064,#12400,#12401);
#11484=AXIS2_PLACEMENT_3D('',#16077,#12403,#12404);
#11485=AXIS2_PLACEMENT_3D('',#16086,#12405,#12406);
#11486=AXIS2_PLACEMENT_3D('',#16110,#12408,#12409);
#11487=AXIS2_PLACEMENT_3D('',#16135,#12411,#12412);
#11488=AXIS2_PLACEMENT_3D('',#16160,#12414,#12415);
#11489=AXIS2_PLACEMENT_3D('',#16184,#12417,#12418);
#11490=AXIS2_PLACEMENT_3D('',#16209,#12420,#12421);
#11491=AXIS2_PLACEMENT_3D('',#16233,#12423,#12424);
#11492=AXIS2_PLACEMENT_3D('',#16258,#12426,#12427);
#11493=AXIS2_PLACEMENT_3D('',#16282,#12429,#12430);
#11494=AXIS2_PLACEMENT_3D('',#16307,#12432,#12433);
#11495=AXIS2_PLACEMENT_3D('',#16332,#12435,#12436);
#11496=AXIS2_PLACEMENT_3D('',#16356,#12438,#12439);
#11497=AXIS2_PLACEMENT_3D('',#16367,#12441,#12442);
#11498=AXIS2_PLACEMENT_3D('',#16373,#12443,#12444);
#11499=AXIS2_PLACEMENT_3D('',#16401,#12446,#12447);
#11500=AXIS2_PLACEMENT_3D('',#16412,#12449,#12450);
#11501=AXIS2_PLACEMENT_3D('',#16435,#12451,#12452);
#11502=AXIS2_PLACEMENT_3D('',#16486,#12454,#12455);
#11503=AXIS2_PLACEMENT_3D('',#16534,#12457,#12458);
#11504=AXIS2_PLACEMENT_3D('',#16582,#12460,#12461);
#11505=AXIS2_PLACEMENT_3D('',#16633,#12463,#12464);
#11506=AXIS2_PLACEMENT_3D('',#16681,#12466,#12467);
#11507=AXIS2_PLACEMENT_3D('',#16729,#12469,#12470);
#11508=AXIS2_PLACEMENT_3D('',#16780,#12472,#12473);
#11509=AXIS2_PLACEMENT_3D('',#16831,#12475,#12476);
#11510=AXIS2_PLACEMENT_3D('',#16879,#12478,#12479);
#11511=AXIS2_PLACEMENT_3D('',#16930,#12481,#12482);
#11512=AXIS2_PLACEMENT_3D('',#16949,#12484,#12485);
#11513=AXIS2_PLACEMENT_3D('',#16969,#12486,#12487);
#11514=AXIS2_PLACEMENT_3D('',#16982,#12489,#12490);
#11515=AXIS2_PLACEMENT_3D('',#16991,#12491,#12492);
#11516=AXIS2_PLACEMENT_3D('',#17015,#12494,#12495);
#11517=AXIS2_PLACEMENT_3D('',#17040,#12497,#12498);
#11518=AXIS2_PLACEMENT_3D('',#17065,#12500,#12501);
#11519=AXIS2_PLACEMENT_3D('',#17089,#12503,#12504);
#11520=AXIS2_PLACEMENT_3D('',#17114,#12506,#12507);
#11521=AXIS2_PLACEMENT_3D('',#17138,#12509,#12510);
#11522=AXIS2_PLACEMENT_3D('',#17163,#12512,#12513);
#11523=AXIS2_PLACEMENT_3D('',#17187,#12515,#12516);
#11524=AXIS2_PLACEMENT_3D('',#17212,#12518,#12519);
#11525=AXIS2_PLACEMENT_3D('',#17237,#12521,#12522);
#11526=AXIS2_PLACEMENT_3D('',#17261,#12524,#12525);
#11527=AXIS2_PLACEMENT_3D('',#17272,#12527,#12528);
#11528=AXIS2_PLACEMENT_3D('',#17278,#12529,#12530);
#11529=AXIS2_PLACEMENT_3D('',#17306,#12532,#12533);
#11530=AXIS2_PLACEMENT_3D('',#17317,#12535,#12536);
#11531=AXIS2_PLACEMENT_3D('',#17340,#12537,#12538);
#11532=AXIS2_PLACEMENT_3D('',#17391,#12540,#12541);
#11533=AXIS2_PLACEMENT_3D('',#17439,#12543,#12544);
#11534=AXIS2_PLACEMENT_3D('',#17487,#12546,#12547);
#11535=AXIS2_PLACEMENT_3D('',#17538,#12549,#12550);
#11536=AXIS2_PLACEMENT_3D('',#17586,#12552,#12553);
#11537=AXIS2_PLACEMENT_3D('',#17634,#12555,#12556);
#11538=AXIS2_PLACEMENT_3D('',#17685,#12558,#12559);
#11539=AXIS2_PLACEMENT_3D('',#17736,#12561,#12562);
#11540=AXIS2_PLACEMENT_3D('',#17784,#12564,#12565);
#11541=AXIS2_PLACEMENT_3D('',#17835,#12567,#12568);
#11542=AXIS2_PLACEMENT_3D('',#17854,#12570,#12571);
#11543=AXIS2_PLACEMENT_3D('',#17874,#12572,#12573);
#11544=AXIS2_PLACEMENT_3D('',#17887,#12575,#12576);
#11545=AXIS2_PLACEMENT_3D('',#17896,#12577,#12578);
#11546=AXIS2_PLACEMENT_3D('',#17920,#12580,#12581);
#11547=AXIS2_PLACEMENT_3D('',#17945,#12583,#12584);
#11548=AXIS2_PLACEMENT_3D('',#17970,#12586,#12587);
#11549=AXIS2_PLACEMENT_3D('',#17994,#12589,#12590);
#11550=AXIS2_PLACEMENT_3D('',#18019,#12592,#12593);
#11551=AXIS2_PLACEMENT_3D('',#18043,#12595,#12596);
#11552=AXIS2_PLACEMENT_3D('',#18068,#12598,#12599);
#11553=AXIS2_PLACEMENT_3D('',#18092,#12601,#12602);
#11554=AXIS2_PLACEMENT_3D('',#18117,#12604,#12605);
#11555=AXIS2_PLACEMENT_3D('',#18142,#12607,#12608);
#11556=AXIS2_PLACEMENT_3D('',#18166,#12610,#12611);
#11557=AXIS2_PLACEMENT_3D('',#18177,#12613,#12614);
#11558=AXIS2_PLACEMENT_3D('',#18183,#12615,#12616);
#11559=AXIS2_PLACEMENT_3D('',#18185,#12617,#12618);
#11560=AXIS2_PLACEMENT_3D('',#18188,#12620,#12621);
#11561=AXIS2_PLACEMENT_3D('',#18189,#12622,#12623);
#11562=AXIS2_PLACEMENT_3D('',#18191,#12624,#12625);
#11563=AXIS2_PLACEMENT_3D('',#18193,#12626,#12627);
#11564=AXIS2_PLACEMENT_3D('',#18194,#12628,#12629);
#11565=AXIS2_PLACEMENT_3D('',#18196,#12630,#12631);
#11566=AXIS2_PLACEMENT_3D('',#18198,#12633,#12634);
#11567=AXIS2_PLACEMENT_3D('',#18201,#12636,#12637);
#11568=AXIS2_PLACEMENT_3D('',#18202,#12638,#12639);
#11569=AXIS2_PLACEMENT_3D('',#18204,#12640,#12641);
#11570=AXIS2_PLACEMENT_3D('',#18206,#12642,#12643);
#11571=AXIS2_PLACEMENT_3D('',#18207,#12644,#12645);
#11572=AXIS2_PLACEMENT_3D('',#18209,#12646,#12647);
#11573=AXIS2_PLACEMENT_3D('',#18211,#12649,#12650);
#11574=AXIS2_PLACEMENT_3D('',#18214,#12652,#12653);
#11575=AXIS2_PLACEMENT_3D('',#18215,#12654,#12655);
#11576=AXIS2_PLACEMENT_3D('',#18326,#12656,#12657);
#11577=AXIS2_PLACEMENT_3D('',#19187,#12658,#12659);
#11578=AXIS2_PLACEMENT_3D('',#19188,#12660,#12661);
#11579=AXIS2_PLACEMENT_3D('',#19299,#12662,#12663);
#11580=AXIS2_PLACEMENT_3D('',#20160,#12664,#12665);
#11581=AXIS2_PLACEMENT_3D('',#20161,#12666,#12667);
#11582=AXIS2_PLACEMENT_3D('',#20272,#12668,#12669);
#11583=AXIS2_PLACEMENT_3D('',#21133,#12670,#12671);
#11584=AXIS2_PLACEMENT_3D('',#21134,#12672,#12673);
#11585=AXIS2_PLACEMENT_3D('',#21245,#12674,#12675);
#11586=AXIS2_PLACEMENT_3D('',#22106,#12676,#12677);
#11587=AXIS2_PLACEMENT_3D('',#22107,#12678,#12679);
#11588=AXIS2_PLACEMENT_3D('',#22108,#12680,#12681);
#11589=AXIS2_PLACEMENT_3D('',#22109,#12682,#12683);
#11590=AXIS2_PLACEMENT_3D('',#22110,#12684,#12685);
#11591=AXIS2_PLACEMENT_3D('',#22111,#12686,#12687);
#11592=AXIS2_PLACEMENT_3D('',#22113,#12688,#12689);
#11593=AXIS2_PLACEMENT_3D('',#22116,#12691,#12692);
#11594=AXIS2_PLACEMENT_3D('',#22117,#12693,#12694);
#11595=AXIS2_PLACEMENT_3D('',#22119,#12695,#12696);
#11596=AXIS2_PLACEMENT_3D('',#22122,#12698,#12699);
#11597=AXIS2_PLACEMENT_3D('',#22123,#12700,#12701);
#11598=AXIS2_PLACEMENT_3D('',#22132,#12706,#12707);
#11599=AXIS2_PLACEMENT_3D('',#22138,#12711,#12712);
#11600=AXIS2_PLACEMENT_3D('',#22144,#12716,#12717);
#11601=AXIS2_PLACEMENT_3D('',#22146,#12719,#12720);
#11602=AXIS2_PLACEMENT_3D('',#22155,#12725,#12726);
#11603=AXIS2_PLACEMENT_3D('',#22164,#12731,#12732);
#11604=AXIS2_PLACEMENT_3D('',#22167,#12735,#12736);
#11605=AXIS2_PLACEMENT_3D('',#22169,#12738,#12739);
#11606=AXIS2_PLACEMENT_3D('',#22171,#12740,#12741);
#11607=AXIS2_PLACEMENT_3D('',#22174,#12743,#12744);
#11608=AXIS2_PLACEMENT_3D('',#22175,#12745,#12746);
#11609=AXIS2_PLACEMENT_3D('',#22177,#12747,#12748);
#11610=AXIS2_PLACEMENT_3D('',#22180,#12750,#12751);
#11611=AXIS2_PLACEMENT_3D('',#22181,#12752,#12753);
#11612=AXIS2_PLACEMENT_3D('',#22182,#12754,#12755);
#11613=AXIS2_PLACEMENT_3D('',#22185,#12756,#12757);
#11614=AXIS2_PLACEMENT_3D('',#22189,#12759,#12760);
#11615=AXIS2_PLACEMENT_3D('',#22193,#12762,#12763);
#11616=AXIS2_PLACEMENT_3D('',#22197,#12765,#12766);
#11617=AXIS2_PLACEMENT_3D('',#22199,#12768,#12769);
#11618=AXIS2_PLACEMENT_3D('',#22203,#12771,#12772);
#11619=AXIS2_PLACEMENT_3D('',#22205,#12774,#12775);
#11620=AXIS2_PLACEMENT_3D('',#22209,#12778,#12779);
#11621=AXIS2_PLACEMENT_3D('',#22212,#12781,#12782);
#11622=AXIS2_PLACEMENT_3D('',#22213,#12783,#12784);
#11623=AXIS2_PLACEMENT_3D('',#22217,#12787,#12788);
#11624=AXIS2_PLACEMENT_3D('',#22221,#12790,#12791);
#11625=AXIS2_PLACEMENT_3D('',#22223,#12793,#12794);
#11626=AXIS2_PLACEMENT_3D('',#22224,#12795,#12796);
#11627=AXIS2_PLACEMENT_3D('',#22228,#12799,#12800);
#11628=AXIS2_PLACEMENT_3D('',#22229,#12801,#12802);
#11629=AXIS2_PLACEMENT_3D('',#22230,#12803,#12804);
#11630=AXIS2_PLACEMENT_3D('',#22232,#12806,#12807);
#11631=AXIS2_PLACEMENT_3D('',#22241,#12812,#12813);
#11632=AXIS2_PLACEMENT_3D('',#22248,#12818,#12819);
#11633=AXIS2_PLACEMENT_3D('',#22254,#12823,#12824);
#11634=AXIS2_PLACEMENT_3D('',#22258,#12828,#12829);
#11635=AXIS2_PLACEMENT_3D('',#22259,#12830,#12831);
#11636=AXIS2_PLACEMENT_3D('',#22260,#12832,#12833);
#11637=AXIS2_PLACEMENT_3D('',#22261,#12834,#12835);
#11638=AXIS2_PLACEMENT_3D('',#22286,#12837,#12838);
#11639=AXIS2_PLACEMENT_3D('',#22318,#12839,#12840);
#11640=AXIS2_PLACEMENT_3D('',#22405,#12842,#12843);
#11641=AXIS2_PLACEMENT_3D('',#22436,#12845,#12846);
#11642=AXIS2_PLACEMENT_3D('',#22474,#12847,#12848);
#11643=AXIS2_PLACEMENT_3D('',#22499,#12850,#12851);
#11644=AXIS2_PLACEMENT_3D('',#22531,#12852,#12853);
#11645=AXIS2_PLACEMENT_3D('',#22618,#12855,#12856);
#11646=AXIS2_PLACEMENT_3D('',#22649,#12858,#12859);
#11647=AXIS2_PLACEMENT_3D('',#22687,#12860,#12861);
#11648=AXIS2_PLACEMENT_3D('',#22697,#12863,#12864);
#11649=AXIS2_PLACEMENT_3D('',#22703,#12865,#12866);
#11650=AXIS2_PLACEMENT_3D('',#22741,#12868,#12869);
#11651=AXIS2_PLACEMENT_3D('',#22777,#12871,#12872);
#11652=AXIS2_PLACEMENT_3D('',#22789,#12874,#12875);
#11653=AXIS2_PLACEMENT_3D('',#22797,#12876,#12877);
#11654=AXIS2_PLACEMENT_3D('',#22807,#12879,#12880);
#11655=AXIS2_PLACEMENT_3D('',#22813,#12881,#12882);
#11656=AXIS2_PLACEMENT_3D('',#22851,#12884,#12885);
#11657=AXIS2_PLACEMENT_3D('',#22887,#12887,#12888);
#11658=AXIS2_PLACEMENT_3D('',#22899,#12890,#12891);
#11659=AXIS2_PLACEMENT_3D('',#22907,#12892,#12893);
#11660=AXIS2_PLACEMENT_3D('',#22910,#12894,#12895);
#11661=AXIS2_PLACEMENT_3D('',#22914,#12898,#12899);
#11662=AXIS2_PLACEMENT_3D('',#22917,#12900,#12901);
#11663=AXIS2_PLACEMENT_3D('',#22921,#12904,#12905);
#11664=AXIS2_PLACEMENT_3D('',#22930,#12910,#12911);
#11665=AXIS2_PLACEMENT_3D('',#22939,#12916,#12917);
#11666=AXIS2_PLACEMENT_3D('',#22941,#12918,#12919);
#11667=AXIS2_PLACEMENT_3D('',#22943,#12921,#12922);
#11668=AXIS2_PLACEMENT_3D('',#22949,#12926,#12927);
#11669=AXIS2_PLACEMENT_3D('',#22955,#12931,#12932);
#11670=AXIS2_PLACEMENT_3D('',#22957,#12933,#12934);
#11671=AXIS2_PLACEMENT_3D('',#22959,#12936,#12937);
#11672=AXIS2_PLACEMENT_3D('',#22961,#12939,#12940);
#11673=AXIS2_PLACEMENT_3D('',#22963,#12942,#12943);
#11674=AXIS2_PLACEMENT_3D('',#22965,#12944,#12945);
#11675=AXIS2_PLACEMENT_3D('',#22966,#12946,#12947);
#11676=AXIS2_PLACEMENT_3D('',#22967,#12948,#12949);
#11677=AXIS2_PLACEMENT_3D('',#22968,#12950,#12951);
#11678=AXIS2_PLACEMENT_3D('',#23761,#12952,#12953);
#11679=AXIS2_PLACEMENT_3D('',#24554,#12954,#12955);
#11680=AXIS2_PLACEMENT_3D('',#24555,#12956,#12957);
#11681=AXIS2_PLACEMENT_3D('',#24557,#12958,#12959);
#11682=AXIS2_PLACEMENT_3D('',#24558,#12960,#12961);
#11683=AXIS2_PLACEMENT_3D('',#24561,#12963,#12964);
#11684=AXIS2_PLACEMENT_3D('',#24562,#12965,#12966);
#11685=AXIS2_PLACEMENT_3D('',#24564,#12967,#12968);
#11686=AXIS2_PLACEMENT_3D('',#24565,#12969,#12970);
#11687=AXIS2_PLACEMENT_3D('',#24605,#12972,#12973);
#11688=AXIS2_PLACEMENT_3D('',#24622,#12975,#12976);
#11689=AXIS2_PLACEMENT_3D('',#24638,#12978,#12979);
#11690=AXIS2_PLACEMENT_3D('',#24639,#12980,#12981);
#11691=AXIS2_PLACEMENT_3D('',#24640,#12982,#12983);
#11692=AXIS2_PLACEMENT_3D('',#24642,#12985,#12986);
#11693=AXIS2_PLACEMENT_3D('',#24652,#12991,#12992);
#11694=AXIS2_PLACEMENT_3D('',#24654,#12993,#12994);
#11695=AXIS2_PLACEMENT_3D('',#24656,#12995,#12996);
#11696=AXIS2_PLACEMENT_3D('',#24658,#12997,#12998);
#11697=AXIS2_PLACEMENT_3D('',#24660,#12999,#13000);
#11698=AXIS2_PLACEMENT_3D('',#24667,#13004,#13005);
#11699=AXIS2_PLACEMENT_3D('',#24668,#13006,#13007);
#11700=AXIS2_PLACEMENT_3D('',#24682,#13008,#13009);
#11701=AXIS2_PLACEMENT_3D('',#24683,#13010,#13011);
#11702=AXIS2_PLACEMENT_3D('',#24685,#13012,#13013);
#11703=AXIS2_PLACEMENT_3D('',#24686,#13014,#13015);
#11704=AXIS2_PLACEMENT_3D('',#24689,#13017,#13018);
#11705=AXIS2_PLACEMENT_3D('',#24690,#13019,#13020);
#11706=AXIS2_PLACEMENT_3D('',#24692,#13021,#13022);
#11707=AXIS2_PLACEMENT_3D('',#24693,#13023,#13024);
#11708=AXIS2_PLACEMENT_3D('',#24739,#13026,#13027);
#11709=AXIS2_PLACEMENT_3D('',#24740,#13028,#13029);
#11710=AXIS2_PLACEMENT_3D('',#24741,#13030,#13031);
#11711=AXIS2_PLACEMENT_3D('',#24754,#13032,#13033);
#11712=AXIS2_PLACEMENT_3D('',#24755,#13034,#13035);
#11713=AXIS2_PLACEMENT_3D('',#24758,#13037,#13038);
#11714=AXIS2_PLACEMENT_3D('',#24759,#13039,#13040);
#11715=AXIS2_PLACEMENT_3D('',#24762,#13042,#13043);
#11716=AXIS2_PLACEMENT_3D('',#24763,#13044,#13045);
#11717=AXIS2_PLACEMENT_3D('',#24766,#13047,#13048);
#11718=AXIS2_PLACEMENT_3D('',#24767,#13049,#13050);
#11719=AXIS2_PLACEMENT_3D('',#24770,#13052,#13053);
#11720=AXIS2_PLACEMENT_3D('',#24771,#13054,#13055);
#11721=AXIS2_PLACEMENT_3D('',#24775,#13058,#13059);
#11722=AXIS2_PLACEMENT_3D('',#24776,#13060,#13061);
#11723=AXIS2_PLACEMENT_3D('',#24782,#13065,#13066);
#11724=AXIS2_PLACEMENT_3D('',#24786,#13069,#13070);
#11725=AXIS2_PLACEMENT_3D('',#24790,#13073,#13074);
#11726=AXIS2_PLACEMENT_3D('',#24792,#13076,#13077);
#11727=AXIS2_PLACEMENT_3D('',#24793,#13078,#13079);
#11728=AXIS2_PLACEMENT_3D('',#24794,#13080,#13081);
#11729=AXIS2_PLACEMENT_3D('',#24796,#13082,#13083);
#11730=AXIS2_PLACEMENT_3D('',#24798,#13084,#13085);
#11731=AXIS2_PLACEMENT_3D('',#24799,#13086,#13087);
#11732=AXIS2_PLACEMENT_3D('',#24802,#13089,#13090);
#11733=AXIS2_PLACEMENT_3D('',#24803,#13091,#13092);
#11734=AXIS2_PLACEMENT_3D('',#24805,#13093,#13094);
#11735=AXIS2_PLACEMENT_3D('',#24806,#13095,#13096);
#11736=AXIS2_PLACEMENT_3D('',#24808,#13097,#13098);
#11737=AXIS2_PLACEMENT_3D('',#24810,#13100,#13101);
#11738=AXIS2_PLACEMENT_3D('',#24812,#13102,#13103);
#11739=AXIS2_PLACEMENT_3D('',#24814,#13105,#13106);
#11740=AXIS2_PLACEMENT_3D('',#24815,#13107,#13108);
#11741=AXIS2_PLACEMENT_3D('',#24816,#13109,#13110);
#11742=AXIS2_PLACEMENT_3D('',#24844,#13112,#13113);
#11743=AXIS2_PLACEMENT_3D('',#24855,#13115,#13116);
#11744=AXIS2_PLACEMENT_3D('',#24878,#13117,#13118);
#11745=AXIS2_PLACEMENT_3D('',#24929,#13120,#13121);
#11746=AXIS2_PLACEMENT_3D('',#24977,#13123,#13124);
#11747=AXIS2_PLACEMENT_3D('',#25025,#13126,#13127);
#11748=AXIS2_PLACEMENT_3D('',#25076,#13129,#13130);
#11749=AXIS2_PLACEMENT_3D('',#25124,#13132,#13133);
#11750=AXIS2_PLACEMENT_3D('',#25172,#13135,#13136);
#11751=AXIS2_PLACEMENT_3D('',#25223,#13138,#13139);
#11752=AXIS2_PLACEMENT_3D('',#25274,#13141,#13142);
#11753=AXIS2_PLACEMENT_3D('',#25322,#13144,#13145);
#11754=AXIS2_PLACEMENT_3D('',#25373,#13147,#13148);
#11755=AXIS2_PLACEMENT_3D('',#25392,#13150,#13151);
#11756=AXIS2_PLACEMENT_3D('',#25412,#13152,#13153);
#11757=AXIS2_PLACEMENT_3D('',#25425,#13155,#13156);
#11758=AXIS2_PLACEMENT_3D('',#25434,#13157,#13158);
#11759=AXIS2_PLACEMENT_3D('',#25458,#13160,#13161);
#11760=AXIS2_PLACEMENT_3D('',#25483,#13163,#13164);
#11761=AXIS2_PLACEMENT_3D('',#25508,#13166,#13167);
#11762=AXIS2_PLACEMENT_3D('',#25532,#13169,#13170);
#11763=AXIS2_PLACEMENT_3D('',#25557,#13172,#13173);
#11764=AXIS2_PLACEMENT_3D('',#25581,#13175,#13176);
#11765=AXIS2_PLACEMENT_3D('',#25606,#13178,#13179);
#11766=AXIS2_PLACEMENT_3D('',#25630,#13181,#13182);
#11767=AXIS2_PLACEMENT_3D('',#25655,#13184,#13185);
#11768=AXIS2_PLACEMENT_3D('',#25680,#13187,#13188);
#11769=AXIS2_PLACEMENT_3D('',#25704,#13190,#13191);
#11770=AXIS2_PLACEMENT_3D('',#25715,#13193,#13194);
#11771=AXIS2_PLACEMENT_3D('',#25721,#13195,#13196);
#11772=AXIS2_PLACEMENT_3D('',#25731,#13198,#13199);
#11773=AXIS2_PLACEMENT_3D('',#25742,#13200,#13201);
#11774=AXIS2_PLACEMENT_3D('',#25793,#13203,#13204);
#11775=AXIS2_PLACEMENT_3D('',#25844,#13206,#13207);
#11776=AXIS2_PLACEMENT_3D('',#25892,#13209,#13210);
#11777=AXIS2_PLACEMENT_3D('',#25943,#13212,#13213);
#11778=AXIS2_PLACEMENT_3D('',#25994,#13215,#13216);
#11779=AXIS2_PLACEMENT_3D('',#26042,#13218,#13219);
#11780=AXIS2_PLACEMENT_3D('',#26061,#13221,#13222);
#11781=AXIS2_PLACEMENT_3D('',#26081,#13223,#13224);
#11782=AXIS2_PLACEMENT_3D('',#26091,#13226,#13227);
#11783=AXIS2_PLACEMENT_3D('',#26102,#13228,#13229);
#11784=AXIS2_PLACEMENT_3D('',#26153,#13231,#13232);
#11785=AXIS2_PLACEMENT_3D('',#26204,#13234,#13235);
#11786=AXIS2_PLACEMENT_3D('',#26252,#13237,#13238);
#11787=AXIS2_PLACEMENT_3D('',#26303,#13240,#13241);
#11788=AXIS2_PLACEMENT_3D('',#26354,#13243,#13244);
#11789=AXIS2_PLACEMENT_3D('',#26402,#13246,#13247);
#11790=AXIS2_PLACEMENT_3D('',#26421,#13249,#13250);
#11791=AXIS2_PLACEMENT_3D('',#26441,#13251,#13252);
#11792=AXIS2_PLACEMENT_3D('',#26455,#13254,#13255);
#11793=AXIS2_PLACEMENT_3D('',#26465,#13256,#13257);
#11794=AXIS2_PLACEMENT_3D('',#26489,#13259,#13260);
#11795=AXIS2_PLACEMENT_3D('',#26514,#13262,#13263);
#11796=AXIS2_PLACEMENT_3D('',#26539,#13265,#13266);
#11797=AXIS2_PLACEMENT_3D('',#26563,#13268,#13269);
#11798=AXIS2_PLACEMENT_3D('',#26588,#13271,#13272);
#11799=AXIS2_PLACEMENT_3D('',#26613,#13274,#13275);
#11800=AXIS2_PLACEMENT_3D('',#26624,#13277,#13278);
#11801=AXIS2_PLACEMENT_3D('',#26630,#13279,#13280);
#11802=AXIS2_PLACEMENT_3D('',#26644,#13282,#13283);
#11803=AXIS2_PLACEMENT_3D('',#26654,#13284,#13285);
#11804=AXIS2_PLACEMENT_3D('',#26678,#13287,#13288);
#11805=AXIS2_PLACEMENT_3D('',#26703,#13290,#13291);
#11806=AXIS2_PLACEMENT_3D('',#26728,#13293,#13294);
#11807=AXIS2_PLACEMENT_3D('',#26752,#13296,#13297);
#11808=AXIS2_PLACEMENT_3D('',#26777,#13299,#13300);
#11809=AXIS2_PLACEMENT_3D('',#26802,#13302,#13303);
#11810=AXIS2_PLACEMENT_3D('',#26813,#13305,#13306);
#11811=AXIS2_PLACEMENT_3D('',#26819,#13307,#13308);
#11812=AXIS2_PLACEMENT_3D('',#27541,#13309,#13310);
#11813=AXIS2_PLACEMENT_3D('',#27544,#13311,#13312);
#11814=AXIS2_PLACEMENT_3D('',#27655,#13318,#13319);
#11815=AXIS2_PLACEMENT_3D('',#28276,#13320,#13321);
#11816=AXIS2_PLACEMENT_3D('',#28277,#13322,#13323);
#11817=AXIS2_PLACEMENT_3D('',#28278,#13324,#13325);
#11818=AXIS2_PLACEMENT_3D('',#28389,#13326,#13327);
#11819=AXIS2_PLACEMENT_3D('',#29250,#13328,#13329);
#11820=AXIS2_PLACEMENT_3D('',#29251,#13330,#13331);
#11821=AXIS2_PLACEMENT_3D('',#29252,#13332,#13333);
#11822=AXIS2_PLACEMENT_3D('',#29254,#13334,#13335);
#11823=AXIS2_PLACEMENT_3D('',#29256,#13336,#13337);
#11824=AXIS2_PLACEMENT_3D('',#29257,#13338,#13339);
#11825=AXIS2_PLACEMENT_3D('',#29258,#13340,#13341);
#11826=AXIS2_PLACEMENT_3D('',#29261,#13343,#13344);
#11827=AXIS2_PLACEMENT_3D('',#29262,#13345,#13346);
#11828=AXIS2_PLACEMENT_3D('',#29264,#13347,#13348);
#11829=AXIS2_PLACEMENT_3D('',#29265,#13349,#13350);
#11830=AXIS2_PLACEMENT_3D('',#29266,#13351,#13352);
#11831=AXIS2_PLACEMENT_3D('',#29269,#13354,#13355);
#11832=AXIS2_PLACEMENT_3D('',#29270,#13356,#13357);
#11833=AXIS2_PLACEMENT_3D('',#29272,#13358,#13359);
#11834=AXIS2_PLACEMENT_3D('',#29274,#13360,#13361);
#11835=AXIS2_PLACEMENT_3D('',#29275,#13362,#13363);
#11836=AXIS2_PLACEMENT_3D('',#29277,#13364,#13365);
#11837=AXIS2_PLACEMENT_3D('',#29279,#13366,#13367);
#11838=AXIS2_PLACEMENT_3D('',#29280,#13368,#13369);
#11839=AXIS2_PLACEMENT_3D('',#29282,#13371,#13372);
#11840=AXIS2_PLACEMENT_3D('',#29284,#13374,#13375);
#11841=AXIS2_PLACEMENT_3D('',#29290,#13379,#13380);
#11842=AXIS2_PLACEMENT_3D('',#29296,#13384,#13385);
#11843=AXIS2_PLACEMENT_3D('',#29298,#13387,#13388);
#11844=AXIS2_PLACEMENT_3D('',#29304,#13392,#13393);
#11845=AXIS2_PLACEMENT_3D('',#29306,#13395,#13396);
#11846=AXIS2_PLACEMENT_3D('',#29307,#13397,#13398);
#11847=AXIS2_PLACEMENT_3D('',#29308,#13399,#13400);
#11848=AXIS2_PLACEMENT_3D('',#29310,#13401,#13402);
#11849=AXIS2_PLACEMENT_3D('',#29312,#13404,#13405);
#11850=AXIS2_PLACEMENT_3D('',#29313,#13406,#13407);
#11851=AXIS2_PLACEMENT_3D('',#29314,#13408,#13409);
#11852=AXIS2_PLACEMENT_3D('',#29315,#13410,#13411);
#11853=AXIS2_PLACEMENT_3D('',#29317,#13412,#13413);
#11854=AXIS2_PLACEMENT_3D('',#29319,#13414,#13415);
#11855=AXIS2_PLACEMENT_3D('',#29320,#13416,#13417);
#11856=AXIS2_PLACEMENT_3D('',#29321,#13418,#13419);
#11857=AXIS2_PLACEMENT_3D('',#29324,#13421,#13422);
#11858=AXIS2_PLACEMENT_3D('',#29325,#13423,#13424);
#11859=AXIS2_PLACEMENT_3D('',#29327,#13425,#13426);
#11860=AXIS2_PLACEMENT_3D('',#29328,#13427,#13428);
#11861=AXIS2_PLACEMENT_3D('',#29330,#13429,#13430);
#11862=AXIS2_PLACEMENT_3D('',#29331,#13431,#13432);
#11863=AXIS2_PLACEMENT_3D('',#29332,#13433,#13434);
#11864=AXIS2_PLACEMENT_3D('',#29334,#13435,#13436);
#11865=AXIS2_PLACEMENT_3D('',#29335,#13437,#13438);
#11866=AXIS2_PLACEMENT_3D('',#29337,#13439,#13440);
#11867=AXIS2_PLACEMENT_3D('',#29339,#13441,#13442);
#11868=AXIS2_PLACEMENT_3D('',#29340,#13443,#13444);
#11869=AXIS2_PLACEMENT_3D('',#29342,#13446,#13447);
#11870=AXIS2_PLACEMENT_3D('',#29344,#13448,#13449);
#11871=AXIS2_PLACEMENT_3D('',#29346,#13450,#13451);
#11872=AXIS2_PLACEMENT_3D('',#29347,#13452,#13453);
#11873=AXIS2_PLACEMENT_3D('',#29349,#13455,#13456);
#11874=AXIS2_PLACEMENT_3D('',#29352,#13458,#13459);
#11875=AXIS2_PLACEMENT_3D('',#29353,#13460,#13461);
#11876=AXIS2_PLACEMENT_3D('',#29356,#13463,#13464);
#11877=AXIS2_PLACEMENT_3D('',#29357,#13465,#13466);
#11878=AXIS2_PLACEMENT_3D('',#29358,#13467,#13468);
#11879=AXIS2_PLACEMENT_3D('',#29359,#13469,#13470);
#11880=AXIS2_PLACEMENT_3D('',#29361,#13471,#13472);
#11881=AXIS2_PLACEMENT_3D('',#29364,#13474,#13475);
#11882=AXIS2_PLACEMENT_3D('',#29365,#13476,#13477);
#11883=AXIS2_PLACEMENT_3D('',#29367,#13478,#13479);
#11884=AXIS2_PLACEMENT_3D('',#29370,#13481,#13482);
#11885=AXIS2_PLACEMENT_3D('',#29371,#13483,#13484);
#11886=AXIS2_PLACEMENT_3D('',#29380,#13489,#13490);
#11887=AXIS2_PLACEMENT_3D('',#29386,#13494,#13495);
#11888=AXIS2_PLACEMENT_3D('',#29392,#13499,#13500);
#11889=AXIS2_PLACEMENT_3D('',#29395,#13503,#13504);
#11890=AXIS2_PLACEMENT_3D('',#29396,#13505,#13506);
#11891=AXIS2_PLACEMENT_3D('',#29397,#13507,#13508);
#11892=AXIS2_PLACEMENT_3D('',#29809,#13509,#13510);
#11893=AXIS2_PLACEMENT_3D('',#29852,#13511,#13512);
#11894=AXIS2_PLACEMENT_3D('',#29853,#13513,#13514);
#11895=AXIS2_PLACEMENT_3D('',#29854,#13515,#13516);
#11896=AXIS2_PLACEMENT_3D('',#29855,#13517,#13518);
#11897=AXIS2_PLACEMENT_3D('',#29856,#13519,#13520);
#11898=AXIS2_PLACEMENT_3D('',#29884,#13522,#13523);
#11899=AXIS2_PLACEMENT_3D('',#29895,#13525,#13526);
#11900=AXIS2_PLACEMENT_3D('',#29918,#13527,#13528);
#11901=AXIS2_PLACEMENT_3D('',#29969,#13530,#13531);
#11902=AXIS2_PLACEMENT_3D('',#30017,#13533,#13534);
#11903=AXIS2_PLACEMENT_3D('',#30065,#13536,#13537);
#11904=AXIS2_PLACEMENT_3D('',#30116,#13539,#13540);
#11905=AXIS2_PLACEMENT_3D('',#30164,#13542,#13543);
#11906=AXIS2_PLACEMENT_3D('',#30212,#13545,#13546);
#11907=AXIS2_PLACEMENT_3D('',#30263,#13548,#13549);
#11908=AXIS2_PLACEMENT_3D('',#30314,#13551,#13552);
#11909=AXIS2_PLACEMENT_3D('',#30362,#13554,#13555);
#11910=AXIS2_PLACEMENT_3D('',#30413,#13557,#13558);
#11911=AXIS2_PLACEMENT_3D('',#30432,#13560,#13561);
#11912=AXIS2_PLACEMENT_3D('',#30452,#13562,#13563);
#11913=AXIS2_PLACEMENT_3D('',#30465,#13565,#13566);
#11914=AXIS2_PLACEMENT_3D('',#30474,#13567,#13568);
#11915=AXIS2_PLACEMENT_3D('',#30498,#13570,#13571);
#11916=AXIS2_PLACEMENT_3D('',#30523,#13573,#13574);
#11917=AXIS2_PLACEMENT_3D('',#30548,#13576,#13577);
#11918=AXIS2_PLACEMENT_3D('',#30572,#13579,#13580);
#11919=AXIS2_PLACEMENT_3D('',#30597,#13582,#13583);
#11920=AXIS2_PLACEMENT_3D('',#30621,#13585,#13586);
#11921=AXIS2_PLACEMENT_3D('',#30646,#13588,#13589);
#11922=AXIS2_PLACEMENT_3D('',#30670,#13591,#13592);
#11923=AXIS2_PLACEMENT_3D('',#30695,#13594,#13595);
#11924=AXIS2_PLACEMENT_3D('',#30720,#13597,#13598);
#11925=AXIS2_PLACEMENT_3D('',#30744,#13600,#13601);
#11926=AXIS2_PLACEMENT_3D('',#30755,#13603,#13604);
#11927=AXIS2_PLACEMENT_3D('',#30761,#13605,#13606);
#11928=AXIS2_PLACEMENT_3D('',#30771,#13608,#13609);
#11929=AXIS2_PLACEMENT_3D('',#30774,#13611,#13612);
#11930=AXIS2_PLACEMENT_3D('',#30776,#13613,#13614);
#11931=AXIS2_PLACEMENT_3D('',#30787,#13615,#13616);
#11932=AXIS2_PLACEMENT_3D('',#30838,#13618,#13619);
#11933=AXIS2_PLACEMENT_3D('',#30889,#13621,#13622);
#11934=AXIS2_PLACEMENT_3D('',#30937,#13624,#13625);
#11935=AXIS2_PLACEMENT_3D('',#30988,#13627,#13628);
#11936=AXIS2_PLACEMENT_3D('',#31039,#13630,#13631);
#11937=AXIS2_PLACEMENT_3D('',#31087,#13633,#13634);
#11938=AXIS2_PLACEMENT_3D('',#31138,#13636,#13637);
#11939=AXIS2_PLACEMENT_3D('',#31189,#13639,#13640);
#11940=AXIS2_PLACEMENT_3D('',#31237,#13642,#13643);
#11941=AXIS2_PLACEMENT_3D('',#31288,#13645,#13646);
#11942=AXIS2_PLACEMENT_3D('',#31339,#13648,#13649);
#11943=AXIS2_PLACEMENT_3D('',#31387,#13651,#13652);
#11944=AXIS2_PLACEMENT_3D('',#31438,#13654,#13655);
#11945=AXIS2_PLACEMENT_3D('',#31489,#13657,#13658);
#11946=AXIS2_PLACEMENT_3D('',#31537,#13660,#13661);
#11947=AXIS2_PLACEMENT_3D('',#31588,#13663,#13664);
#11948=AXIS2_PLACEMENT_3D('',#31607,#13666,#13667);
#11949=AXIS2_PLACEMENT_3D('',#31627,#13668,#13669);
#11950=AXIS2_PLACEMENT_3D('',#31641,#13671,#13672);
#11951=AXIS2_PLACEMENT_3D('',#31651,#13673,#13674);
#11952=AXIS2_PLACEMENT_3D('',#31675,#13676,#13677);
#11953=AXIS2_PLACEMENT_3D('',#31700,#13679,#13680);
#11954=AXIS2_PLACEMENT_3D('',#31725,#13682,#13683);
#11955=AXIS2_PLACEMENT_3D('',#31749,#13685,#13686);
#11956=AXIS2_PLACEMENT_3D('',#31774,#13688,#13689);
#11957=AXIS2_PLACEMENT_3D('',#31799,#13691,#13692);
#11958=AXIS2_PLACEMENT_3D('',#31823,#13694,#13695);
#11959=AXIS2_PLACEMENT_3D('',#31848,#13697,#13698);
#11960=AXIS2_PLACEMENT_3D('',#31873,#13700,#13701);
#11961=AXIS2_PLACEMENT_3D('',#31897,#13703,#13704);
#11962=AXIS2_PLACEMENT_3D('',#31922,#13706,#13707);
#11963=AXIS2_PLACEMENT_3D('',#31947,#13709,#13710);
#11964=AXIS2_PLACEMENT_3D('',#31971,#13712,#13713);
#11965=AXIS2_PLACEMENT_3D('',#31996,#13715,#13716);
#11966=AXIS2_PLACEMENT_3D('',#32021,#13718,#13719);
#11967=AXIS2_PLACEMENT_3D('',#32045,#13721,#13722);
#11968=AXIS2_PLACEMENT_3D('',#32056,#13724,#13725);
#11969=AXIS2_PLACEMENT_3D('',#32062,#13726,#13727);
#11970=AXIS2_PLACEMENT_3D('',#32170,#13728,#13729);
#11971=AXIS2_PLACEMENT_3D('',#33289,#13730,#13731);
#11972=AXIS2_PLACEMENT_3D('',#33290,#13732,#13733);
#11973=AXIS2_PLACEMENT_3D('',#33291,#13734,#13735);
#11974=AXIS2_PLACEMENT_3D('',#33402,#13736,#13737);
#11975=AXIS2_PLACEMENT_3D('',#34263,#13738,#13739);
#11976=AXIS2_PLACEMENT_3D('',#34264,#13740,#13741);
#11977=AXIS2_PLACEMENT_3D('',#34265,#13742,#13743);
#11978=AXIS2_PLACEMENT_3D('',#34274,#13748,#13749);
#11979=AXIS2_PLACEMENT_3D('',#34280,#13753,#13754);
#11980=AXIS2_PLACEMENT_3D('',#34286,#13758,#13759);
#11981=AXIS2_PLACEMENT_3D('',#34289,#13762,#13763);
#11982=AXIS2_PLACEMENT_3D('',#34290,#13764,#13765);
#11983=AXIS2_PLACEMENT_3D('',#34291,#13766,#13767);
#11984=AXIS2_PLACEMENT_3D('',#34292,#13768,#13769);
#11985=AXIS2_PLACEMENT_3D('',#34302,#13771,#13772);
#11986=AXIS2_PLACEMENT_3D('',#34305,#13774,#13775);
#11987=AXIS2_PLACEMENT_3D('',#34307,#13776,#13777);
#11988=AXIS2_PLACEMENT_3D('',#34318,#13778,#13779);
#11989=AXIS2_PLACEMENT_3D('',#34369,#13781,#13782);
#11990=AXIS2_PLACEMENT_3D('',#34420,#13784,#13785);
#11991=AXIS2_PLACEMENT_3D('',#34468,#13787,#13788);
#11992=AXIS2_PLACEMENT_3D('',#34516,#13790,#13791);
#11993=AXIS2_PLACEMENT_3D('',#34567,#13793,#13794);
#11994=AXIS2_PLACEMENT_3D('',#34618,#13796,#13797);
#11995=AXIS2_PLACEMENT_3D('',#34666,#13799,#13800);
#11996=AXIS2_PLACEMENT_3D('',#34717,#13802,#13803);
#11997=AXIS2_PLACEMENT_3D('',#34736,#13805,#13806);
#11998=AXIS2_PLACEMENT_3D('',#34756,#13807,#13808);
#11999=AXIS2_PLACEMENT_3D('',#34770,#13810,#13811);
#12000=AXIS2_PLACEMENT_3D('',#34780,#13812,#13813);
#12001=AXIS2_PLACEMENT_3D('',#34804,#13815,#13816);
#12002=AXIS2_PLACEMENT_3D('',#34829,#13818,#13819);
#12003=AXIS2_PLACEMENT_3D('',#34853,#13821,#13822);
#12004=AXIS2_PLACEMENT_3D('',#34878,#13824,#13825);
#12005=AXIS2_PLACEMENT_3D('',#34902,#13827,#13828);
#12006=AXIS2_PLACEMENT_3D('',#34927,#13830,#13831);
#12007=AXIS2_PLACEMENT_3D('',#34952,#13833,#13834);
#12008=AXIS2_PLACEMENT_3D('',#34976,#13836,#13837);
#12009=AXIS2_PLACEMENT_3D('',#34987,#13839,#13840);
#12010=AXIS2_PLACEMENT_3D('',#34993,#13841,#13842);
#12011=AXIS2_PLACEMENT_3D('',#35101,#13843,#13844);
#12012=AXIS2_PLACEMENT_3D('',#35812,#13845,#13846);
#12013=AXIS2_PLACEMENT_3D('',#35813,#13847,#13848);
#12014=AXIS2_PLACEMENT_3D('',#35814,#13849,#13850);
#12015=AXIS2_PLACEMENT_3D('',#35816,#13851,#13852);
#12016=AXIS2_PLACEMENT_3D('',#35819,#13854,#13855);
#12017=AXIS2_PLACEMENT_3D('',#35820,#13856,#13857);
#12018=AXIS2_PLACEMENT_3D('',#35829,#13862,#13863);
#12019=AXIS2_PLACEMENT_3D('',#35835,#13867,#13868);
#12020=AXIS2_PLACEMENT_3D('',#35843,#13873,#13874);
#12021=AXIS2_PLACEMENT_3D('',#35847,#13877,#13878);
#12022=AXIS2_PLACEMENT_3D('',#35853,#13882,#13883);
#12023=AXIS2_PLACEMENT_3D('',#35856,#13886,#13887);
#12024=AXIS2_PLACEMENT_3D('',#35857,#13888,#13889);
#12025=AXIS2_PLACEMENT_3D('',#35858,#13890,#13891);
#12026=AXIS2_PLACEMENT_3D('',#35859,#13892,#13893);
#12027=AXIS2_PLACEMENT_3D('',#35861,#13894,#13895);
#12028=AXIS2_PLACEMENT_3D('',#35864,#13897,#13898);
#12029=AXIS2_PLACEMENT_3D('',#35865,#13899,#13900);
#12030=AXIS2_PLACEMENT_3D('',#35874,#13905,#13906);
#12031=AXIS2_PLACEMENT_3D('',#35880,#13910,#13911);
#12032=AXIS2_PLACEMENT_3D('',#35886,#13915,#13916);
#12033=AXIS2_PLACEMENT_3D('',#35889,#13919,#13920);
#12034=AXIS2_PLACEMENT_3D('',#35890,#13921,#13922);
#12035=AXIS2_PLACEMENT_3D('',#35891,#13923,#13924);
#12036=AXIS2_PLACEMENT_3D('',#35892,#13925,#13926);
#12037=AXIS2_PLACEMENT_3D('',#35895,#13927,#13928);
#12038=AXIS2_PLACEMENT_3D('',#35896,#13929,#13930);
#12039=AXIS2_PLACEMENT_3D('',#35897,#13931,#13932);
#12040=AXIS2_PLACEMENT_3D('',#35899,#13933,#13934);
#12041=AXIS2_PLACEMENT_3D('',#35901,#13935,#13936);
#12042=AXIS2_PLACEMENT_3D('',#35902,#13937,#13938);
#12043=AXIS2_PLACEMENT_3D('',#35904,#13939,#13940);
#12044=AXIS2_PLACEMENT_3D('',#35906,#13942,#13943);
#12045=AXIS2_PLACEMENT_3D('',#35907,#13944,#13945);
#12046=AXIS2_PLACEMENT_3D('',#35910,#13947,#13948);
#12047=AXIS2_PLACEMENT_3D('',#35911,#13949,#13950);
#12048=AXIS2_PLACEMENT_3D('',#35912,#13951,#13952);
#12049=AXIS2_PLACEMENT_3D('',#36324,#13953,#13954);
#12050=AXIS2_PLACEMENT_3D('',#36367,#13955,#13956);
#12051=AXIS2_PLACEMENT_3D('',#36368,#13957,#13958);
#12052=AXIS2_PLACEMENT_3D('',#36369,#13959,#13960);
#12053=AXIS2_PLACEMENT_3D('',#36370,#13961,#13962);
#12054=AXIS2_PLACEMENT_3D('',#36371,#13963,#13964);
#12055=AXIS2_PLACEMENT_3D('',#36387,#13966,#13967);
#12056=AXIS2_PLACEMENT_3D('',#36395,#13968,#13969);
#12057=AXIS2_PLACEMENT_3D('',#36443,#13971,#13972);
#12058=AXIS2_PLACEMENT_3D('',#36491,#13974,#13975);
#12059=AXIS2_PLACEMENT_3D('',#36539,#13977,#13978);
#12060=AXIS2_PLACEMENT_3D('',#36587,#13980,#13981);
#12061=AXIS2_PLACEMENT_3D('',#36635,#13983,#13984);
#12062=AXIS2_PLACEMENT_3D('',#36683,#13986,#13987);
#12063=AXIS2_PLACEMENT_3D('',#36737,#13989,#13990);
#12064=AXIS2_PLACEMENT_3D('',#36785,#13992,#13993);
#12065=AXIS2_PLACEMENT_3D('',#36833,#13995,#13996);
#12066=AXIS2_PLACEMENT_3D('',#36887,#13998,#13999);
#12067=AXIS2_PLACEMENT_3D('',#36935,#14001,#14002);
#12068=AXIS2_PLACEMENT_3D('',#36983,#14004,#14005);
#12069=AXIS2_PLACEMENT_3D('',#37031,#14007,#14008);
#12070=AXIS2_PLACEMENT_3D('',#37082,#14010,#14011);
#12071=AXIS2_PLACEMENT_3D('',#37130,#14013,#14014);
#12072=AXIS2_PLACEMENT_3D('',#37144,#14016,#14017);
#12073=AXIS2_PLACEMENT_3D('',#37152,#14018,#14019);
#12074=AXIS2_PLACEMENT_3D('',#37176,#14021,#14022);
#12075=AXIS2_PLACEMENT_3D('',#37200,#14024,#14025);
#12076=AXIS2_PLACEMENT_3D('',#37226,#14027,#14028);
#12077=AXIS2_PLACEMENT_3D('',#37250,#14030,#14031);
#12078=AXIS2_PLACEMENT_3D('',#37274,#14033,#14034);
#12079=AXIS2_PLACEMENT_3D('',#37299,#14036,#14037);
#12080=AXIS2_PLACEMENT_3D('',#37324,#14039,#14040);
#12081=AXIS2_PLACEMENT_3D('',#37348,#14042,#14043);
#12082=AXIS2_PLACEMENT_3D('',#37373,#14045,#14046);
#12083=AXIS2_PLACEMENT_3D('',#37398,#14048,#14049);
#12084=AXIS2_PLACEMENT_3D('',#37422,#14051,#14052);
#12085=AXIS2_PLACEMENT_3D('',#37446,#14054,#14055);
#12086=AXIS2_PLACEMENT_3D('',#37471,#14057,#14058);
#12087=AXIS2_PLACEMENT_3D('',#37496,#14060,#14061);
#12088=AXIS2_PLACEMENT_3D('',#37520,#14063,#14064);
#12089=AXIS2_PLACEMENT_3D('',#37637,#14065,#14066);
#12090=AXIS2_PLACEMENT_3D('',#37704,#14068,#14069);
#12091=AXIS2_PLACEMENT_3D('',#38209,#14070,#14071);
#12092=AXIS2_PLACEMENT_3D('',#38220,#14072,#14073);
#12093=AXIS2_PLACEMENT_3D('',#38721,#14074,#14075);
#12094=AXIS2_PLACEMENT_3D('',#38722,#14076,#14077);
#12095=AXIS2_PLACEMENT_3D('',#38731,#14082,#14083);
#12096=AXIS2_PLACEMENT_3D('',#38737,#14087,#14088);
#12097=AXIS2_PLACEMENT_3D('',#38743,#14092,#14093);
#12098=AXIS2_PLACEMENT_3D('',#38749,#14097,#14098);
#12099=AXIS2_PLACEMENT_3D('',#38755,#14102,#14103);
#12100=AXIS2_PLACEMENT_3D('',#38758,#14106,#14107);
#12101=AXIS2_PLACEMENT_3D('',#38759,#14108,#14109);
#12102=AXIS2_PLACEMENT_3D('',#38761,#14110,#14111);
#12103=AXIS2_PLACEMENT_3D('',#38762,#14112,#14113);
#12104=AXIS2_PLACEMENT_3D('',#38765,#14115,#14116);
#12105=AXIS2_PLACEMENT_3D('',#38766,#14117,#14118);
#12106=AXIS2_PLACEMENT_3D('',#38767,#14119,#14120);
#12107=AXIS2_PLACEMENT_3D('',#38768,#14121,#14122);
#12108=AXIS2_PLACEMENT_3D('',#38769,#14123,#14124);
#12109=AXIS2_PLACEMENT_3D('',#38785,#14126,#14127);
#12110=AXIS2_PLACEMENT_3D('',#38793,#14128,#14129);
#12111=AXIS2_PLACEMENT_3D('',#38841,#14131,#14132);
#12112=AXIS2_PLACEMENT_3D('',#38889,#14134,#14135);
#12113=AXIS2_PLACEMENT_3D('',#38937,#14137,#14138);
#12114=AXIS2_PLACEMENT_3D('',#38991,#14140,#14141);
#12115=AXIS2_PLACEMENT_3D('',#39039,#14143,#14144);
#12116=AXIS2_PLACEMENT_3D('',#39087,#14146,#14147);
#12117=AXIS2_PLACEMENT_3D('',#39141,#14149,#14150);
#12118=AXIS2_PLACEMENT_3D('',#39189,#14152,#14153);
#12119=AXIS2_PLACEMENT_3D('',#39237,#14155,#14156);
#12120=AXIS2_PLACEMENT_3D('',#39253,#14158,#14159);
#12121=AXIS2_PLACEMENT_3D('',#39263,#14160,#14161);
#12122=AXIS2_PLACEMENT_3D('',#39287,#14163,#14164);
#12123=AXIS2_PLACEMENT_3D('',#39311,#14166,#14167);
#12124=AXIS2_PLACEMENT_3D('',#39336,#14169,#14170);
#12125=AXIS2_PLACEMENT_3D('',#39361,#14172,#14173);
#12126=AXIS2_PLACEMENT_3D('',#39385,#14175,#14176);
#12127=AXIS2_PLACEMENT_3D('',#39410,#14178,#14179);
#12128=AXIS2_PLACEMENT_3D('',#39435,#14181,#14182);
#12129=AXIS2_PLACEMENT_3D('',#39459,#14184,#14185);
#12130=AXIS2_PLACEMENT_3D('',#39483,#14187,#14188);
#12131=AXIS2_PLACEMENT_3D('',#39648,#14189,#14190);
#12132=AXIS2_PLACEMENT_3D('',#39667,#14192,#14193);
#12133=AXIS2_PLACEMENT_3D('',#40025,#14194,#14195);
#12134=AXIS2_PLACEMENT_3D('',#40036,#14196,#14197);
#12135=AXIS2_PLACEMENT_3D('',#40399,#14198,#14199);
#12136=AXIS2_PLACEMENT_3D('',#40400,#14200,#14201);
#12137=AXIS2_PLACEMENT_3D('',#40409,#14206,#14207);
#12138=AXIS2_PLACEMENT_3D('',#40415,#14211,#14212);
#12139=AXIS2_PLACEMENT_3D('',#40421,#14216,#14217);
#12140=AXIS2_PLACEMENT_3D('',#40427,#14221,#14222);
#12141=AXIS2_PLACEMENT_3D('',#40433,#14226,#14227);
#12142=AXIS2_PLACEMENT_3D('',#40436,#14230,#14231);
#12143=AXIS2_PLACEMENT_3D('',#40437,#14232,#14233);
#12144=AXIS2_PLACEMENT_3D('',#40439,#14234,#14235);
#12145=AXIS2_PLACEMENT_3D('',#40440,#14236,#14237);
#12146=AXIS2_PLACEMENT_3D('',#40443,#14239,#14240);
#12147=AXIS2_PLACEMENT_3D('',#40444,#14241,#14242);
#12148=AXIS2_PLACEMENT_3D('',#40445,#14243,#14244);
#12149=AXIS2_PLACEMENT_3D('',#40446,#14245,#14246);
#12150=AXIS2_PLACEMENT_3D('',#40447,#14247,#14248);
#12151=AXIS2_PLACEMENT_3D('',#40463,#14250,#14251);
#12152=AXIS2_PLACEMENT_3D('',#40471,#14252,#14253);
#12153=AXIS2_PLACEMENT_3D('',#40519,#14255,#14256);
#12154=AXIS2_PLACEMENT_3D('',#40567,#14258,#14259);
#12155=AXIS2_PLACEMENT_3D('',#40621,#14261,#14262);
#12156=AXIS2_PLACEMENT_3D('',#40669,#14264,#14265);
#12157=AXIS2_PLACEMENT_3D('',#40717,#14267,#14268);
#12158=AXIS2_PLACEMENT_3D('',#40771,#14270,#14271);
#12159=AXIS2_PLACEMENT_3D('',#40819,#14273,#14274);
#12160=AXIS2_PLACEMENT_3D('',#40867,#14276,#14277);
#12161=AXIS2_PLACEMENT_3D('',#40921,#14279,#14280);
#12162=AXIS2_PLACEMENT_3D('',#40969,#14282,#14283);
#12163=AXIS2_PLACEMENT_3D('',#41017,#14285,#14286);
#12164=AXIS2_PLACEMENT_3D('',#41071,#14288,#14289);
#12165=AXIS2_PLACEMENT_3D('',#41119,#14291,#14292);
#12166=AXIS2_PLACEMENT_3D('',#41167,#14294,#14295);
#12167=AXIS2_PLACEMENT_3D('',#41218,#14297,#14298);
#12168=AXIS2_PLACEMENT_3D('',#41266,#14300,#14301);
#12169=AXIS2_PLACEMENT_3D('',#41314,#14303,#14304);
#12170=AXIS2_PLACEMENT_3D('',#41330,#14306,#14307);
#12171=AXIS2_PLACEMENT_3D('',#41340,#14308,#14309);
#12172=AXIS2_PLACEMENT_3D('',#41364,#14311,#14312);
#12173=AXIS2_PLACEMENT_3D('',#41388,#14314,#14315);
#12174=AXIS2_PLACEMENT_3D('',#41414,#14317,#14318);
#12175=AXIS2_PLACEMENT_3D('',#41438,#14320,#14321);
#12176=AXIS2_PLACEMENT_3D('',#41462,#14323,#14324);
#12177=AXIS2_PLACEMENT_3D('',#41487,#14326,#14327);
#12178=AXIS2_PLACEMENT_3D('',#41512,#14329,#14330);
#12179=AXIS2_PLACEMENT_3D('',#41536,#14332,#14333);
#12180=AXIS2_PLACEMENT_3D('',#41561,#14335,#14336);
#12181=AXIS2_PLACEMENT_3D('',#41586,#14338,#14339);
#12182=AXIS2_PLACEMENT_3D('',#41610,#14341,#14342);
#12183=AXIS2_PLACEMENT_3D('',#41635,#14344,#14345);
#12184=AXIS2_PLACEMENT_3D('',#41660,#14347,#14348);
#12185=AXIS2_PLACEMENT_3D('',#41684,#14350,#14351);
#12186=AXIS2_PLACEMENT_3D('',#41709,#14353,#14354);
#12187=AXIS2_PLACEMENT_3D('',#41734,#14356,#14357);
#12188=AXIS2_PLACEMENT_3D('',#41758,#14359,#14360);
#12189=AXIS2_PLACEMENT_3D('',#41917,#14361,#14362);
#12190=AXIS2_PLACEMENT_3D('',#41936,#14364,#14365);
#12191=AXIS2_PLACEMENT_3D('',#42504,#14366,#14367);
#12192=AXIS2_PLACEMENT_3D('',#42515,#14368,#14369);
#12193=AXIS2_PLACEMENT_3D('',#43082,#14370,#14371);
#12194=AXIS2_PLACEMENT_3D('',#43083,#14372,#14373);
#12195=AXIS2_PLACEMENT_3D('',#43092,#14378,#14379);
#12196=AXIS2_PLACEMENT_3D('',#43098,#14383,#14384);
#12197=AXIS2_PLACEMENT_3D('',#43104,#14388,#14389);
#12198=AXIS2_PLACEMENT_3D('',#43110,#14393,#14394);
#12199=AXIS2_PLACEMENT_3D('',#43116,#14398,#14399);
#12200=AXIS2_PLACEMENT_3D('',#43119,#14402,#14403);
#12201=AXIS2_PLACEMENT_3D('',#43120,#14404,#14405);
#12202=AXIS2_PLACEMENT_3D('',#43122,#14406,#14407);
#12203=AXIS2_PLACEMENT_3D('',#43123,#14408,#14409);
#12204=AXIS2_PLACEMENT_3D('',#43126,#14411,#14412);
#12205=AXIS2_PLACEMENT_3D('',#43127,#14413,#14414);
#12206=AXIS2_PLACEMENT_3D('',#43128,#14415,#14416);
#12207=AXIS2_PLACEMENT_3D('',#43129,#14417,#14418);
#12208=AXIS2_PLACEMENT_3D('',#43130,#14419,#14420);
#12209=AXIS2_PLACEMENT_3D('',#43146,#14422,#14423);
#12210=AXIS2_PLACEMENT_3D('',#43157,#14424,#14425);
#12211=AXIS2_PLACEMENT_3D('',#43205,#14427,#14428);
#12212=AXIS2_PLACEMENT_3D('',#43222,#14430,#14431);
#12213=AXIS2_PLACEMENT_3D('',#43232,#14432,#14433);
#12214=AXIS2_PLACEMENT_3D('',#43257,#14435,#14436);
#12215=AXIS2_PLACEMENT_3D('',#43458,#14437,#14438);
#12216=AXIS2_PLACEMENT_3D('',#43486,#14440,#14441);
#12217=AXIS2_PLACEMENT_3D('',#43668,#14442,#14443);
#12218=AXIS2_PLACEMENT_3D('',#43679,#14444,#14445);
#12219=AXIS2_PLACEMENT_3D('',#43862,#14446,#14447);
#12220=AXIS2_PLACEMENT_3D('',#43863,#14448,#14449);
#12221=AXIS2_PLACEMENT_3D('',#43872,#14454,#14455);
#12222=AXIS2_PLACEMENT_3D('',#43878,#14459,#14460);
#12223=AXIS2_PLACEMENT_3D('',#43884,#14464,#14465);
#12224=AXIS2_PLACEMENT_3D('',#43890,#14469,#14470);
#12225=AXIS2_PLACEMENT_3D('',#43896,#14474,#14475);
#12226=AXIS2_PLACEMENT_3D('',#43899,#14478,#14479);
#12227=AXIS2_PLACEMENT_3D('',#43900,#14480,#14481);
#12228=AXIS2_PLACEMENT_3D('',#43902,#14482,#14483);
#12229=AXIS2_PLACEMENT_3D('',#43903,#14484,#14485);
#12230=AXIS2_PLACEMENT_3D('',#43906,#14487,#14488);
#12231=AXIS2_PLACEMENT_3D('',#43907,#14489,#14490);
#12232=AXIS2_PLACEMENT_3D('',#43908,#14491,#14492);
#12233=AXIS2_PLACEMENT_3D('',#43909,#14493,#14494);
#12234=AXIS2_PLACEMENT_3D('',#43910,#14495,#14496);
#12235=AXIS2_PLACEMENT_3D('',#43911,#14497,#14498);
#12236=AXIS2_PLACEMENT_3D('',#43912,#14499,#14500);
#12237=AXIS2_PLACEMENT_3D('',#43913,#14501,#14502);
#12238=AXIS2_PLACEMENT_3D('',#43914,#14503,#14504);
#12239=AXIS2_PLACEMENT_3D('',#43915,#14505,#14506);
#12240=AXIS2_PLACEMENT_3D('',#43916,#14507,#14508);
#12241=AXIS2_PLACEMENT_3D('',#43917,#14509,#14510);
#12242=AXIS2_PLACEMENT_3D('',#43918,#14511,#14512);
#12243=AXIS2_PLACEMENT_3D('',#43919,#14513,#14514);
#12244=AXIS2_PLACEMENT_3D('',#43920,#14515,#14516);
#12245=AXIS2_PLACEMENT_3D('',#43921,#14517,#14518);
#12246=AXIS2_PLACEMENT_3D('',#43922,#14519,#14520);
#12247=AXIS2_PLACEMENT_3D('',#43923,#14521,#14522);
#12248=AXIS2_PLACEMENT_3D('',#43924,#14523,#14524);
#12249=AXIS2_PLACEMENT_3D('',#43925,#14525,#14526);
#12250=AXIS2_PLACEMENT_3D('',#43926,#14527,#14528);
#12251=AXIS2_PLACEMENT_3D('',#43927,#14529,#14530);
#12252=AXIS2_PLACEMENT_3D('',#43928,#14531,#14532);
#12253=AXIS2_PLACEMENT_3D('',#43929,#14533,#14534);
#12254=AXIS2_PLACEMENT_3D('',#43930,#14535,#14536);
#12255=AXIS2_PLACEMENT_3D('',#43931,#14537,#14538);
#12256=AXIS2_PLACEMENT_3D('',#43932,#14539,#14540);
#12257=AXIS2_PLACEMENT_3D('',#43933,#14541,#14542);
#12258=AXIS2_PLACEMENT_3D('',#43934,#14543,#14544);
#12259=AXIS2_PLACEMENT_3D('',#43935,#14545,#14546);
#12260=AXIS2_PLACEMENT_3D('',#43936,#14547,#14548);
#12261=AXIS2_PLACEMENT_3D('',#43937,#14549,#14550);
#12262=AXIS2_PLACEMENT_3D('',#43938,#14551,#14552);
#12263=AXIS2_PLACEMENT_3D('',#43939,#14553,#14554);
#12264=AXIS2_PLACEMENT_3D('',#43940,#14555,#14556);
#12265=AXIS2_PLACEMENT_3D('',#43941,#14557,#14558);
#12266=AXIS2_PLACEMENT_3D('',#43942,#14559,#14560);
#12267=DIRECTION('axis',(0.,0.,1.));
#12268=DIRECTION('refdir',(1.,0.,0.));
#12269=DIRECTION('axis',(0.,0.,1.));
#12270=DIRECTION('refdir',(1.,0.,0.));
#12271=DIRECTION('center_axis',(0.,0.,-1.));
#12272=DIRECTION('ref_axis',(1.,0.,0.));
#12273=DIRECTION('',(0.,0.,-1.));
#12274=DIRECTION('center_axis',(0.,0.,1.));
#12275=DIRECTION('ref_axis',(1.,0.,0.));
#12276=DIRECTION('',(0.,0.,-1.));
#12277=DIRECTION('center_axis',(0.,0.,1.));
#12278=DIRECTION('ref_axis',(1.,0.,0.));
#12279=DIRECTION('center_axis',(0.,0.,-1.));
#12280=DIRECTION('ref_axis',(1.,0.,0.));
#12281=DIRECTION('',(0.,0.,-1.));
#12282=DIRECTION('center_axis',(0.,0.,-1.));
#12283=DIRECTION('ref_axis',(1.,0.,0.));
#12284=DIRECTION('',(0.,0.,-1.));
#12285=DIRECTION('center_axis',(0.,0.,-1.));
#12286=DIRECTION('ref_axis',(1.,0.,0.));
#12287=DIRECTION('',(0.,0.,-1.));
#12288=DIRECTION('center_axis',(0.,0.,-1.));
#12289=DIRECTION('ref_axis',(1.,0.,0.));
#12290=DIRECTION('',(0.,0.,-1.));
#12291=DIRECTION('center_axis',(0.,0.,-1.));
#12292=DIRECTION('ref_axis',(1.,0.,0.));
#12293=DIRECTION('',(0.,0.,-1.));
#12294=DIRECTION('center_axis',(0.,0.,-1.));
#12295=DIRECTION('ref_axis',(1.,0.,0.));
#12296=DIRECTION('',(0.,0.,-1.));
#12297=DIRECTION('center_axis',(0.,0.,-1.));
#12298=DIRECTION('ref_axis',(1.,0.,0.));
#12299=DIRECTION('',(0.,0.,-1.));
#12300=DIRECTION('center_axis',(0.,0.,-1.));
#12301=DIRECTION('ref_axis',(1.,0.,0.));
#12302=DIRECTION('',(0.,0.,-1.));
#12303=DIRECTION('center_axis',(0.,0.,-1.));
#12304=DIRECTION('ref_axis',(1.,0.,0.));
#12305=DIRECTION('',(0.,0.,-1.));
#12306=DIRECTION('center_axis',(0.,0.,-1.));
#12307=DIRECTION('ref_axis',(1.,0.,0.));
#12308=DIRECTION('',(0.,0.,-1.));
#12309=DIRECTION('center_axis',(0.,0.,-1.));
#12310=DIRECTION('ref_axis',(0.938438617144983,-0.345446033196231,0.));
#12311=DIRECTION('',(0.,0.,-1.));
#12312=DIRECTION('center_axis',(0.,0.,-1.));
#12313=DIRECTION('ref_axis',(1.,0.,0.));
#12314=DIRECTION('center_axis',(0.,0.,-1.));
#12315=DIRECTION('ref_axis',(0.450153067737633,0.892951407192126,0.));
#12316=DIRECTION('',(1.22464679914735E-16,-6.89669277429462E-30,-1.));
#12317=DIRECTION('center_axis',(0.,0.,1.));
#12318=DIRECTION('ref_axis',(1.,-5.61933055413145E-14,0.));
#12319=DIRECTION('center_axis',(0.,0.,-1.));
#12320=DIRECTION('ref_axis',(1.,-5.61933055413145E-14,0.));
#12321=DIRECTION('',(1.22464679914735E-16,-6.89669277429462E-30,-1.));
#12322=DIRECTION('center_axis',(0.,0.,-1.));
#12323=DIRECTION('ref_axis',(1.,-5.61933055413145E-14,0.));
#12324=DIRECTION('',(1.22464679914735E-16,-6.89669277429462E-30,-1.));
#12325=DIRECTION('center_axis',(0.,0.,-1.));
#12326=DIRECTION('ref_axis',(1.,-5.61933055413145E-14,0.));
#12327=DIRECTION('',(1.22464679914735E-16,-6.89669277429462E-30,-1.));
#12328=DIRECTION('center_axis',(0.,0.,-1.));
#12329=DIRECTION('ref_axis',(1.,-5.61933055413145E-14,0.));
#12330=DIRECTION('',(1.22464679914735E-16,-6.89669277429462E-30,-1.));
#12331=DIRECTION('center_axis',(0.,0.,-1.));
#12332=DIRECTION('ref_axis',(1.,-5.61933055413145E-14,0.));
#12333=DIRECTION('',(1.22464679914735E-16,-6.89669277429462E-30,-1.));
#12334=DIRECTION('center_axis',(0.,0.,-1.));
#12335=DIRECTION('ref_axis',(1.,-5.61933055413145E-14,0.));
#12336=DIRECTION('',(1.22464679914735E-16,-6.89669277429462E-30,-1.));
#12337=DIRECTION('center_axis',(0.,0.,-1.));
#12338=DIRECTION('ref_axis',(1.,-5.61933055413145E-14,0.));
#12339=DIRECTION('',(1.22464679914735E-16,-6.89669277429462E-30,-1.));
#12340=DIRECTION('center_axis',(0.,0.,-1.));
#12341=DIRECTION('ref_axis',(1.,-5.61933055413145E-14,0.));
#12342=DIRECTION('',(1.22464679914735E-16,-6.89669277429462E-30,-1.));
#12343=DIRECTION('center_axis',(0.,0.,-1.));
#12344=DIRECTION('ref_axis',(1.,-5.61933055413145E-14,0.));
#12345=DIRECTION('',(1.22464679914735E-16,-6.89669277429462E-30,-1.));
#12346=DIRECTION('center_axis',(0.,0.,-1.));
#12347=DIRECTION('ref_axis',(1.,-5.61933055413145E-14,0.));
#12348=DIRECTION('',(1.22464679914735E-16,-6.89669277429462E-30,-1.));
#12349=DIRECTION('center_axis',(0.,0.,-1.));
#12350=DIRECTION('ref_axis',(1.,-5.61933055413145E-14,0.));
#12351=DIRECTION('',(1.22464679914735E-16,-6.89669277429462E-30,-1.));
#12352=DIRECTION('center_axis',(0.,0.,-1.));
#12353=DIRECTION('ref_axis',(-0.609341520949359,-0.79290788295181,0.));
#12354=DIRECTION('',(1.22464679914735E-16,-6.89669277429462E-30,-1.));
#12355=DIRECTION('center_axis',(0.,0.,-1.));
#12356=DIRECTION('ref_axis',(1.,-5.61933055413145E-14,0.));
#12357=DIRECTION('center_axis',(0.,0.,-1.));
#12358=DIRECTION('ref_axis',(1.,0.,0.));
#12359=DIRECTION('',(0.,0.,-1.));
#12360=DIRECTION('center_axis',(0.,0.,1.));
#12361=DIRECTION('ref_axis',(1.,0.,0.));
#12362=DIRECTION('',(0.,0.,-1.));
#12363=DIRECTION('center_axis',(0.,0.,1.));
#12364=DIRECTION('ref_axis',(1.,0.,0.));
#12365=DIRECTION('center_axis',(0.,0.,-1.));
#12366=DIRECTION('ref_axis',(1.,0.,0.));
#12367=DIRECTION('',(0.,0.,-1.));
#12368=DIRECTION('center_axis',(0.,0.,-1.));
#12369=DIRECTION('ref_axis',(1.,0.,0.));
#12370=DIRECTION('',(0.,0.,-1.));
#12371=DIRECTION('center_axis',(0.,0.,-1.));
#12372=DIRECTION('ref_axis',(1.,0.,0.));
#12373=DIRECTION('',(0.,0.,-1.));
#12374=DIRECTION('center_axis',(0.,0.,-1.));
#12375=DIRECTION('ref_axis',(1.,0.,0.));
#12376=DIRECTION('',(0.,0.,-1.));
#12377=DIRECTION('center_axis',(0.,0.,-1.));
#12378=DIRECTION('ref_axis',(1.,0.,0.));
#12379=DIRECTION('',(0.,0.,-1.));
#12380=DIRECTION('center_axis',(0.,0.,-1.));
#12381=DIRECTION('ref_axis',(1.,0.,0.));
#12382=DIRECTION('',(0.,0.,-1.));
#12383=DIRECTION('center_axis',(0.,0.,-1.));
#12384=DIRECTION('ref_axis',(1.,0.,0.));
#12385=DIRECTION('',(0.,0.,-1.));
#12386=DIRECTION('center_axis',(0.,0.,-1.));
#12387=DIRECTION('ref_axis',(1.,0.,0.));
#12388=DIRECTION('',(0.,0.,-1.));
#12389=DIRECTION('center_axis',(0.,0.,-1.));
#12390=DIRECTION('ref_axis',(1.,0.,0.));
#12391=DIRECTION('',(0.,0.,-1.));
#12392=DIRECTION('center_axis',(0.,0.,-1.));
#12393=DIRECTION('ref_axis',(1.,0.,0.));
#12394=DIRECTION('',(0.,0.,-1.));
#12395=DIRECTION('center_axis',(0.,0.,-1.));
#12396=DIRECTION('ref_axis',(0.938438595705222,-0.345446091439475,0.));
#12397=DIRECTION('',(0.,0.,-1.));
#12398=DIRECTION('center_axis',(0.,0.,-1.));
#12399=DIRECTION('ref_axis',(1.,0.,0.));
#12400=DIRECTION('center_axis',(0.,0.,-1.));
#12401=DIRECTION('ref_axis',(0.450153019553355,0.892951431482697,0.));
#12402=DIRECTION('',(1.22464679914735E-16,-6.89669277429462E-30,-1.));
#12403=DIRECTION('center_axis',(0.,0.,1.));
#12404=DIRECTION('ref_axis',(1.,-5.61933055413145E-14,0.));
#12405=DIRECTION('center_axis',(0.,0.,-1.));
#12406=DIRECTION('ref_axis',(1.,-5.61933055413145E-14,0.));
#12407=DIRECTION('',(1.22464679914735E-16,-6.89669277429462E-30,-1.));
#12408=DIRECTION('center_axis',(0.,0.,-1.));
#12409=DIRECTION('ref_axis',(1.,-5.61933055413145E-14,0.));
#12410=DIRECTION('',(1.22464679914735E-16,-6.89669277429462E-30,-1.));
#12411=DIRECTION('center_axis',(0.,0.,-1.));
#12412=DIRECTION('ref_axis',(1.,-5.61933055413145E-14,0.));
#12413=DIRECTION('',(1.22464679914735E-16,-6.89669277429462E-30,-1.));
#12414=DIRECTION('center_axis',(0.,0.,-1.));
#12415=DIRECTION('ref_axis',(1.,-5.61933055413145E-14,0.));
#12416=DIRECTION('',(1.22464679914735E-16,-6.89669277429462E-30,-1.));
#12417=DIRECTION('center_axis',(0.,0.,-1.));
#12418=DIRECTION('ref_axis',(1.,-5.61933055413145E-14,0.));
#12419=DIRECTION('',(1.22464679914735E-16,-6.89669277429462E-30,-1.));
#12420=DIRECTION('center_axis',(0.,0.,-1.));
#12421=DIRECTION('ref_axis',(1.,-5.61933055413145E-14,0.));
#12422=DIRECTION('',(1.22464679914735E-16,-6.89669277429462E-30,-1.));
#12423=DIRECTION('center_axis',(0.,0.,-1.));
#12424=DIRECTION('ref_axis',(1.,-5.61933055413145E-14,0.));
#12425=DIRECTION('',(1.22464679914735E-16,-6.89669277429462E-30,-1.));
#12426=DIRECTION('center_axis',(0.,0.,-1.));
#12427=DIRECTION('ref_axis',(1.,-5.61933055413145E-14,0.));
#12428=DIRECTION('',(1.22464679914735E-16,-6.89669277429462E-30,-1.));
#12429=DIRECTION('center_axis',(0.,0.,-1.));
#12430=DIRECTION('ref_axis',(1.,-5.61933055413145E-14,0.));
#12431=DIRECTION('',(1.22464679914735E-16,-6.89669277429462E-30,-1.));
#12432=DIRECTION('center_axis',(0.,0.,-1.));
#12433=DIRECTION('ref_axis',(1.,-5.61933055413145E-14,0.));
#12434=DIRECTION('',(1.22464679914735E-16,-6.89669277429462E-30,-1.));
#12435=DIRECTION('center_axis',(0.,0.,-1.));
#12436=DIRECTION('ref_axis',(1.,-5.61933055413145E-14,0.));
#12437=DIRECTION('',(1.22464679914735E-16,-6.89669277429462E-30,-1.));
#12438=DIRECTION('center_axis',(0.,0.,-1.));
#12439=DIRECTION('ref_axis',(-0.609341511570002,-0.792907890159749,0.));
#12440=DIRECTION('',(1.22464679914735E-16,-6.89669277429462E-30,-1.));
#12441=DIRECTION('center_axis',(0.,0.,-1.));
#12442=DIRECTION('ref_axis',(1.,-5.61933055413145E-14,0.));
#12443=DIRECTION('center_axis',(0.,0.,-1.));
#12444=DIRECTION('ref_axis',(1.,0.,0.));
#12445=DIRECTION('',(0.,0.,-1.));
#12446=DIRECTION('center_axis',(0.,0.,1.));
#12447=DIRECTION('ref_axis',(1.,0.,0.));
#12448=DIRECTION('',(0.,0.,-1.));
#12449=DIRECTION('center_axis',(0.,0.,1.));
#12450=DIRECTION('ref_axis',(1.,0.,0.));
#12451=DIRECTION('center_axis',(0.,0.,-1.));
#12452=DIRECTION('ref_axis',(1.,0.,0.));
#12453=DIRECTION('',(0.,0.,-1.));
#12454=DIRECTION('center_axis',(0.,0.,-1.));
#12455=DIRECTION('ref_axis',(1.,0.,0.));
#12456=DIRECTION('',(0.,0.,-1.));
#12457=DIRECTION('center_axis',(0.,0.,-1.));
#12458=DIRECTION('ref_axis',(1.,0.,0.));
#12459=DIRECTION('',(0.,0.,-1.));
#12460=DIRECTION('center_axis',(0.,0.,-1.));
#12461=DIRECTION('ref_axis',(1.,0.,0.));
#12462=DIRECTION('',(0.,0.,-1.));
#12463=DIRECTION('center_axis',(0.,0.,-1.));
#12464=DIRECTION('ref_axis',(1.,0.,0.));
#12465=DIRECTION('',(0.,0.,-1.));
#12466=DIRECTION('center_axis',(0.,0.,-1.));
#12467=DIRECTION('ref_axis',(1.,0.,0.));
#12468=DIRECTION('',(0.,0.,-1.));
#12469=DIRECTION('center_axis',(0.,0.,-1.));
#12470=DIRECTION('ref_axis',(1.,0.,0.));
#12471=DIRECTION('',(0.,0.,-1.));
#12472=DIRECTION('center_axis',(0.,0.,-1.));
#12473=DIRECTION('ref_axis',(1.,0.,0.));
#12474=DIRECTION('',(0.,0.,-1.));
#12475=DIRECTION('center_axis',(0.,0.,-1.));
#12476=DIRECTION('ref_axis',(1.,0.,0.));
#12477=DIRECTION('',(0.,0.,-1.));
#12478=DIRECTION('center_axis',(0.,0.,-1.));
#12479=DIRECTION('ref_axis',(1.,0.,0.));
#12480=DIRECTION('',(0.,0.,-1.));
#12481=DIRECTION('center_axis',(0.,0.,-1.));
#12482=DIRECTION('ref_axis',(0.938438601292299,-0.345446076261625,0.));
#12483=DIRECTION('',(0.,0.,-1.));
#12484=DIRECTION('center_axis',(0.,0.,-1.));
#12485=DIRECTION('ref_axis',(1.,0.,0.));
#12486=DIRECTION('center_axis',(0.,0.,-1.));
#12487=DIRECTION('ref_axis',(0.450153040552508,0.892951420896642,0.));
#12488=DIRECTION('',(1.22464679914735E-16,-7.42605394171526E-30,-1.));
#12489=DIRECTION('center_axis',(0.,0.,1.));
#12490=DIRECTION('ref_axis',(1.,-6.05158675060312E-14,0.));
#12491=DIRECTION('center_axis',(0.,0.,-1.));
#12492=DIRECTION('ref_axis',(1.,-6.05158675060312E-14,0.));
#12493=DIRECTION('',(1.22464679914735E-16,-7.42605394171526E-30,-1.));
#12494=DIRECTION('center_axis',(0.,0.,-1.));
#12495=DIRECTION('ref_axis',(1.,-6.05158675060312E-14,0.));
#12496=DIRECTION('',(1.22464679914735E-16,-7.42605394171526E-30,-1.));
#12497=DIRECTION('center_axis',(0.,0.,-1.));
#12498=DIRECTION('ref_axis',(1.,-6.05158675060312E-14,0.));
#12499=DIRECTION('',(1.22464679914735E-16,-7.42605394171526E-30,-1.));
#12500=DIRECTION('center_axis',(0.,0.,-1.));
#12501=DIRECTION('ref_axis',(1.,-6.05158675060312E-14,0.));
#12502=DIRECTION('',(1.22464679914735E-16,-7.42605394171526E-30,-1.));
#12503=DIRECTION('center_axis',(0.,0.,-1.));
#12504=DIRECTION('ref_axis',(1.,-6.05158675060312E-14,0.));
#12505=DIRECTION('',(1.22464679914735E-16,-7.42605394171526E-30,-1.));
#12506=DIRECTION('center_axis',(0.,0.,-1.));
#12507=DIRECTION('ref_axis',(1.,-6.05158675060312E-14,0.));
#12508=DIRECTION('',(1.22464679914735E-16,-7.42605394171526E-30,-1.));
#12509=DIRECTION('center_axis',(0.,0.,-1.));
#12510=DIRECTION('ref_axis',(1.,-6.05158675060312E-14,0.));
#12511=DIRECTION('',(1.22464679914735E-16,-7.42605394171526E-30,-1.));
#12512=DIRECTION('center_axis',(0.,0.,-1.));
#12513=DIRECTION('ref_axis',(1.,-6.05158675060312E-14,0.));
#12514=DIRECTION('',(1.22464679914735E-16,-7.42605394171526E-30,-1.));
#12515=DIRECTION('center_axis',(0.,0.,-1.));
#12516=DIRECTION('ref_axis',(1.,-6.05158675060312E-14,0.));
#12517=DIRECTION('',(1.22464679914735E-16,-7.42605394171526E-30,-1.));
#12518=DIRECTION('center_axis',(0.,0.,-1.));
#12519=DIRECTION('ref_axis',(1.,-6.05158675060312E-14,0.));
#12520=DIRECTION('',(1.22464679914735E-16,-7.42605394171526E-30,-1.));
#12521=DIRECTION('center_axis',(0.,0.,-1.));
#12522=DIRECTION('ref_axis',(1.,-6.05158675060312E-14,0.));
#12523=DIRECTION('',(1.22464679914735E-16,-7.42605394171526E-30,-1.));
#12524=DIRECTION('center_axis',(0.,0.,-1.));
#12525=DIRECTION('ref_axis',(-0.609341503082739,-0.792907896682123,0.));
#12526=DIRECTION('',(1.22464679914735E-16,-7.42605394171526E-30,-1.));
#12527=DIRECTION('center_axis',(0.,0.,-1.));
#12528=DIRECTION('ref_axis',(1.,-6.05158675060312E-14,0.));
#12529=DIRECTION('center_axis',(0.,0.,-1.));
#12530=DIRECTION('ref_axis',(1.,0.,0.));
#12531=DIRECTION('',(0.,0.,-1.));
#12532=DIRECTION('center_axis',(0.,0.,1.));
#12533=DIRECTION('ref_axis',(1.,0.,0.));
#12534=DIRECTION('',(0.,0.,-1.));
#12535=DIRECTION('center_axis',(0.,0.,1.));
#12536=DIRECTION('ref_axis',(1.,0.,0.));
#12537=DIRECTION('center_axis',(0.,0.,-1.));
#12538=DIRECTION('ref_axis',(1.,0.,0.));
#12539=DIRECTION('',(0.,0.,-1.));
#12540=DIRECTION('center_axis',(0.,0.,-1.));
#12541=DIRECTION('ref_axis',(1.,0.,0.));
#12542=DIRECTION('',(0.,0.,-1.));
#12543=DIRECTION('center_axis',(0.,0.,-1.));
#12544=DIRECTION('ref_axis',(1.,0.,0.));
#12545=DIRECTION('',(0.,0.,-1.));
#12546=DIRECTION('center_axis',(0.,0.,-1.));
#12547=DIRECTION('ref_axis',(1.,0.,0.));
#12548=DIRECTION('',(0.,0.,-1.));
#12549=DIRECTION('center_axis',(0.,0.,-1.));
#12550=DIRECTION('ref_axis',(1.,0.,0.));
#12551=DIRECTION('',(0.,0.,-1.));
#12552=DIRECTION('center_axis',(0.,0.,-1.));
#12553=DIRECTION('ref_axis',(1.,0.,0.));
#12554=DIRECTION('',(0.,0.,-1.));
#12555=DIRECTION('center_axis',(0.,0.,-1.));
#12556=DIRECTION('ref_axis',(1.,0.,0.));
#12557=DIRECTION('',(0.,0.,-1.));
#12558=DIRECTION('center_axis',(0.,0.,-1.));
#12559=DIRECTION('ref_axis',(1.,0.,0.));
#12560=DIRECTION('',(0.,0.,-1.));
#12561=DIRECTION('center_axis',(0.,0.,-1.));
#12562=DIRECTION('ref_axis',(1.,0.,0.));
#12563=DIRECTION('',(0.,0.,-1.));
#12564=DIRECTION('center_axis',(0.,0.,-1.));
#12565=DIRECTION('ref_axis',(1.,0.,0.));
#12566=DIRECTION('',(0.,0.,-1.));
#12567=DIRECTION('center_axis',(0.,0.,-1.));
#12568=DIRECTION('ref_axis',(0.938438612980319,-0.345446044509957,0.));
#12569=DIRECTION('',(0.,0.,-1.));
#12570=DIRECTION('center_axis',(0.,0.,-1.));
#12571=DIRECTION('ref_axis',(1.,0.,0.));
#12572=DIRECTION('center_axis',(0.,0.,-1.));
#12573=DIRECTION('ref_axis',(0.450153049056661,0.892951416609544,0.));
#12574=DIRECTION('',(1.22464679914735E-16,-7.42605394171526E-30,-1.));
#12575=DIRECTION('center_axis',(0.,0.,1.));
#12576=DIRECTION('ref_axis',(1.,-6.05158675060312E-14,0.));
#12577=DIRECTION('center_axis',(0.,0.,-1.));
#12578=DIRECTION('ref_axis',(1.,-6.05158675060312E-14,0.));
#12579=DIRECTION('',(1.22464679914735E-16,-7.42605394171526E-30,-1.));
#12580=DIRECTION('center_axis',(0.,0.,-1.));
#12581=DIRECTION('ref_axis',(1.,-6.05158675060312E-14,0.));
#12582=DIRECTION('',(1.22464679914735E-16,-7.42605394171526E-30,-1.));
#12583=DIRECTION('center_axis',(0.,0.,-1.));
#12584=DIRECTION('ref_axis',(1.,-6.05158675060312E-14,0.));
#12585=DIRECTION('',(1.22464679914735E-16,-7.42605394171526E-30,-1.));
#12586=DIRECTION('center_axis',(0.,0.,-1.));
#12587=DIRECTION('ref_axis',(1.,-6.05158675060312E-14,0.));
#12588=DIRECTION('',(1.22464679914735E-16,-7.42605394171526E-30,-1.));
#12589=DIRECTION('center_axis',(0.,0.,-1.));
#12590=DIRECTION('ref_axis',(1.,-6.05158675060312E-14,0.));
#12591=DIRECTION('',(1.22464679914735E-16,-7.42605394171526E-30,-1.));
#12592=DIRECTION('center_axis',(0.,0.,-1.));
#12593=DIRECTION('ref_axis',(1.,-6.05158675060312E-14,0.));
#12594=DIRECTION('',(1.22464679914735E-16,-7.42605394171526E-30,-1.));
#12595=DIRECTION('center_axis',(0.,0.,-1.));
#12596=DIRECTION('ref_axis',(1.,-6.05158675060312E-14,0.));
#12597=DIRECTION('',(1.22464679914735E-16,-7.42605394171526E-30,-1.));
#12598=DIRECTION('center_axis',(0.,0.,-1.));
#12599=DIRECTION('ref_axis',(1.,-6.05158675060312E-14,0.));
#12600=DIRECTION('',(1.22464679914735E-16,-7.42605394171526E-30,-1.));
#12601=DIRECTION('center_axis',(0.,0.,-1.));
#12602=DIRECTION('ref_axis',(1.,-6.05158675060312E-14,0.));
#12603=DIRECTION('',(1.22464679914735E-16,-7.42605394171526E-30,-1.));
#12604=DIRECTION('center_axis',(0.,0.,-1.));
#12605=DIRECTION('ref_axis',(1.,-6.05158675060312E-14,0.));
#12606=DIRECTION('',(1.22464679914735E-16,-7.42605394171526E-30,-1.));
#12607=DIRECTION('center_axis',(0.,0.,-1.));
#12608=DIRECTION('ref_axis',(1.,-6.05158675060312E-14,0.));
#12609=DIRECTION('',(1.22464679914735E-16,-7.42605394171526E-30,-1.));
#12610=DIRECTION('center_axis',(0.,0.,-1.));
#12611=DIRECTION('ref_axis',(-0.609341531225801,-0.792907875054471,0.));
#12612=DIRECTION('',(1.22464679914735E-16,-7.42605394171526E-30,-1.));
#12613=DIRECTION('center_axis',(0.,0.,-1.));
#12614=DIRECTION('ref_axis',(1.,-6.05158675060312E-14,0.));
#12615=DIRECTION('center_axis',(0.,1.,0.));
#12616=DIRECTION('ref_axis',(0.,0.,-1.));
#12617=DIRECTION('center_axis',(0.,1.,0.));
#12618=DIRECTION('ref_axis',(0.,0.,-1.));
#12619=DIRECTION('',(0.,1.,0.));
#12620=DIRECTION('center_axis',(0.,-1.,0.));
#12621=DIRECTION('ref_axis',(0.,0.,-1.));
#12622=DIRECTION('center_axis',(0.,0.,1.));
#12623=DIRECTION('ref_axis',(-1.,0.,0.));
#12624=DIRECTION('center_axis',(0.,0.,1.));
#12625=DIRECTION('ref_axis',(-1.,0.,0.));
#12626=DIRECTION('center_axis',(0.,0.,1.));
#12627=DIRECTION('ref_axis',(-1.,0.,0.));
#12628=DIRECTION('center_axis',(0.,0.,1.));
#12629=DIRECTION('ref_axis',(-1.,0.,0.));
#12630=DIRECTION('center_axis',(0.,0.,1.));
#12631=DIRECTION('ref_axis',(-1.,0.,0.));
#12632=DIRECTION('',(0.,0.,1.));
#12633=DIRECTION('center_axis',(0.,0.,1.));
#12634=DIRECTION('ref_axis',(-1.,0.,0.));
#12635=DIRECTION('',(0.,0.,1.));
#12636=DIRECTION('center_axis',(0.,0.,-1.));
#12637=DIRECTION('ref_axis',(-1.,0.,0.));
#12638=DIRECTION('center_axis',(0.,0.,1.));
#12639=DIRECTION('ref_axis',(-1.,0.,0.));
#12640=DIRECTION('center_axis',(0.,0.,1.));
#12641=DIRECTION('ref_axis',(-1.,0.,0.));
#12642=DIRECTION('center_axis',(0.,0.,1.));
#12643=DIRECTION('ref_axis',(-1.,0.,0.));
#12644=DIRECTION('center_axis',(0.,0.,1.));
#12645=DIRECTION('ref_axis',(-1.,0.,0.));
#12646=DIRECTION('center_axis',(0.,0.,1.));
#12647=DIRECTION('ref_axis',(-1.,0.,0.));
#12648=DIRECTION('',(0.,0.,1.));
#12649=DIRECTION('center_axis',(0.,0.,1.));
#12650=DIRECTION('ref_axis',(-1.,0.,0.));
#12651=DIRECTION('',(0.,0.,1.));
#12652=DIRECTION('center_axis',(0.,0.,-1.));
#12653=DIRECTION('ref_axis',(-1.,0.,0.));
#12654=DIRECTION('center_axis',(0.,0.,1.));
#12655=DIRECTION('ref_axis',(1.,0.,0.));
#12656=DIRECTION('center_axis',(0.,0.,-1.));
#12657=DIRECTION('ref_axis',(1.,-6.05158675060312E-14,0.));
#12658=DIRECTION('center_axis',(0.,0.,-1.));
#12659=DIRECTION('ref_axis',(1.,0.,0.));
#12660=DIRECTION('center_axis',(0.,0.,1.));
#12661=DIRECTION('ref_axis',(1.,0.,0.));
#12662=DIRECTION('center_axis',(0.,0.,-1.));
#12663=DIRECTION('ref_axis',(1.,-6.05158675060312E-14,0.));
#12664=DIRECTION('center_axis',(0.,0.,-1.));
#12665=DIRECTION('ref_axis',(1.,0.,0.));
#12666=DIRECTION('center_axis',(0.,0.,1.));
#12667=DIRECTION('ref_axis',(1.,0.,0.));
#12668=DIRECTION('center_axis',(0.,0.,-1.));
#12669=DIRECTION('ref_axis',(1.,-5.61933055413145E-14,0.));
#12670=DIRECTION('center_axis',(0.,0.,-1.));
#12671=DIRECTION('ref_axis',(1.,0.,0.));
#12672=DIRECTION('center_axis',(0.,0.,1.));
#12673=DIRECTION('ref_axis',(1.,0.,0.));
#12674=DIRECTION('center_axis',(0.,0.,-1.));
#12675=DIRECTION('ref_axis',(1.,-5.61933055413145E-14,0.));
#12676=DIRECTION('center_axis',(0.,0.,-1.));
#12677=DIRECTION('ref_axis',(1.,0.,0.));
#12678=DIRECTION('center_axis',(0.,0.,-1.));
#12679=DIRECTION('ref_axis',(1.,0.,0.));
#12680=DIRECTION('center_axis',(0.,0.,-1.));
#12681=DIRECTION('ref_axis',(1.,0.,0.));
#12682=DIRECTION('center_axis',(0.,0.,-1.));
#12683=DIRECTION('ref_axis',(1.,0.,0.));
#12684=DIRECTION('center_axis',(0.,0.,-1.));
#12685=DIRECTION('ref_axis',(1.,0.,0.));
#12686=DIRECTION('center_axis',(0.,0.,-1.));
#12687=DIRECTION('ref_axis',(1.,0.,0.));
#12688=DIRECTION('center_axis',(0.,0.,-1.));
#12689=DIRECTION('ref_axis',(1.,0.,0.));
#12690=DIRECTION('',(0.,0.,-1.));
#12691=DIRECTION('center_axis',(0.,0.,1.));
#12692=DIRECTION('ref_axis',(1.,0.,0.));
#12693=DIRECTION('center_axis',(0.,0.,-1.));
#12694=DIRECTION('ref_axis',(1.,0.,0.));
#12695=DIRECTION('center_axis',(0.,0.,-1.));
#12696=DIRECTION('ref_axis',(1.,0.,0.));
#12697=DIRECTION('',(0.,0.,-1.));
#12698=DIRECTION('center_axis',(0.,0.,1.));
#12699=DIRECTION('ref_axis',(1.,0.,0.));
#12700=DIRECTION('center_axis',(0.,1.,0.));
#12701=DIRECTION('ref_axis',(-1.,0.,0.));
#12702=DIRECTION('',(-1.,0.,0.));
#12703=DIRECTION('',(0.,0.,-1.));
#12704=DIRECTION('',(-1.,0.,0.));
#12705=DIRECTION('',(0.,0.,1.));
#12706=DIRECTION('center_axis',(1.,0.,0.));
#12707=DIRECTION('ref_axis',(0.,1.,0.));
#12708=DIRECTION('',(0.,1.,0.));
#12709=DIRECTION('',(0.,1.,0.));
#12710=DIRECTION('',(0.,0.,1.));
#12711=DIRECTION('center_axis',(0.,-1.,0.));
#12712=DIRECTION('ref_axis',(1.,0.,0.));
#12713=DIRECTION('',(1.,0.,0.));
#12714=DIRECTION('',(1.,0.,0.));
#12715=DIRECTION('',(0.,0.,1.));
#12716=DIRECTION('center_axis',(0.,0.,1.));
#12717=DIRECTION('ref_axis',(1.,0.,0.));
#12718=DIRECTION('',(0.,1.,0.));
#12719=DIRECTION('center_axis',(0.,1.,0.));
#12720=DIRECTION('ref_axis',(-1.,0.,0.));
#12721=DIRECTION('',(-1.,0.,0.));
#12722=DIRECTION('',(0.,0.,1.));
#12723=DIRECTION('',(-1.,0.,0.));
#12724=DIRECTION('',(0.,0.,1.));
#12725=DIRECTION('center_axis',(0.,-1.,0.));
#12726=DIRECTION('ref_axis',(1.,0.,0.));
#12727=DIRECTION('',(1.,0.,0.));
#12728=DIRECTION('',(0.,0.,-1.));
#12729=DIRECTION('',(1.,0.,0.));
#12730=DIRECTION('',(0.,0.,1.));
#12731=DIRECTION('center_axis',(-1.,0.,0.));
#12732=DIRECTION('ref_axis',(0.,-1.,0.));
#12733=DIRECTION('',(0.,-1.,0.));
#12734=DIRECTION('',(0.,-1.,0.));
#12735=DIRECTION('center_axis',(0.,0.,1.));
#12736=DIRECTION('ref_axis',(1.,0.,0.));
#12737=DIRECTION('',(0.,-1.,0.));
#12738=DIRECTION('center_axis',(0.,0.,1.));
#12739=DIRECTION('ref_axis',(1.,0.,0.));
#12740=DIRECTION('center_axis',(0.,0.,-1.));
#12741=DIRECTION('ref_axis',(1.,0.,0.));
#12742=DIRECTION('',(0.,0.,-1.));
#12743=DIRECTION('center_axis',(0.,0.,1.));
#12744=DIRECTION('ref_axis',(1.,0.,0.));
#12745=DIRECTION('center_axis',(0.,0.,1.));
#12746=DIRECTION('ref_axis',(1.,0.,0.));
#12747=DIRECTION('center_axis',(0.,0.,1.));
#12748=DIRECTION('ref_axis',(1.,0.,0.));
#12749=DIRECTION('',(0.,0.,-1.));
#12750=DIRECTION('center_axis',(0.,0.,-1.));
#12751=DIRECTION('ref_axis',(1.,0.,0.));
#12752=DIRECTION('center_axis',(0.,0.,1.));
#12753=DIRECTION('ref_axis',(1.,0.,0.));
#12754=DIRECTION('center_axis',(0.,0.,-1.));
#12755=DIRECTION('ref_axis',(-1.,0.,0.));
#12756=DIRECTION('center_axis',(0.,0.,1.));
#12757=DIRECTION('ref_axis',(-0.707106781186547,0.707106781186547,0.));
#12758=DIRECTION('',(0.,1.,0.));
#12759=DIRECTION('center_axis',(0.,0.,1.));
#12760=DIRECTION('ref_axis',(-0.707106781186548,-0.707106781186547,0.));
#12761=DIRECTION('',(-1.,0.,0.));
#12762=DIRECTION('center_axis',(0.,0.,1.));
#12763=DIRECTION('ref_axis',(0.707106781186547,-0.707106781186547,0.));
#12764=DIRECTION('',(0.,-1.,0.));
#12765=DIRECTION('center_axis',(0.,0.,1.));
#12766=DIRECTION('ref_axis',(0.707106781186548,0.707106781186547,0.));
#12767=DIRECTION('',(1.,0.,0.));
#12768=DIRECTION('center_axis',(0.,0.,-1.));
#12769=DIRECTION('ref_axis',(-0.707106781186547,0.707106781186547,0.));
#12770=DIRECTION('',(0.,0.,1.));
#12771=DIRECTION('center_axis',(0.,0.,1.));
#12772=DIRECTION('ref_axis',(-0.707106781186547,0.707106781186547,0.));
#12773=DIRECTION('',(0.,0.,-1.));
#12774=DIRECTION('center_axis',(0.,1.,0.));
#12775=DIRECTION('ref_axis',(1.,0.,0.));
#12776=DIRECTION('',(0.,0.,-1.));
#12777=DIRECTION('',(1.,0.,0.));
#12778=DIRECTION('center_axis',(0.,0.,-1.));
#12779=DIRECTION('ref_axis',(0.707106781186548,0.707106781186547,0.));
#12780=DIRECTION('',(0.,0.,1.));
#12781=DIRECTION('center_axis',(0.,0.,1.));
#12782=DIRECTION('ref_axis',(0.707106781186548,0.707106781186547,0.));
#12783=DIRECTION('center_axis',(1.,0.,0.));
#12784=DIRECTION('ref_axis',(0.,-1.,0.));
#12785=DIRECTION('',(0.,0.,-1.));
#12786=DIRECTION('',(0.,-1.,0.));
#12787=DIRECTION('center_axis',(0.,0.,-1.));
#12788=DIRECTION('ref_axis',(-0.707106781186548,-0.707106781186547,0.));
#12789=DIRECTION('',(0.,0.,1.));
#12790=DIRECTION('center_axis',(0.,0.,1.));
#12791=DIRECTION('ref_axis',(-0.707106781186548,-0.707106781186547,0.));
#12792=DIRECTION('',(0.,0.,-1.));
#12793=DIRECTION('center_axis',(0.,0.,-1.));
#12794=DIRECTION('ref_axis',(-1.,0.,0.));
#12795=DIRECTION('center_axis',(0.,-1.,0.));
#12796=DIRECTION('ref_axis',(-1.,0.,0.));
#12797=DIRECTION('',(-1.,0.,0.));
#12798=DIRECTION('',(0.,0.,1.));
#12799=DIRECTION('center_axis',(0.,0.,-1.));
#12800=DIRECTION('ref_axis',(0.707106781186547,-0.707106781186547,0.));
#12801=DIRECTION('center_axis',(0.,0.,1.));
#12802=DIRECTION('ref_axis',(0.707106781186547,-0.707106781186547,0.));
#12803=DIRECTION('center_axis',(-1.,0.,0.));
#12804=DIRECTION('ref_axis',(0.,1.,0.));
#12805=DIRECTION('',(0.,1.,0.));
#12806=DIRECTION('center_axis',(0.,1.,0.));
#12807=DIRECTION('ref_axis',(-1.,0.,0.));
#12808=DIRECTION('',(-1.,0.,0.));
#12809=DIRECTION('',(0.,0.,1.));
#12810=DIRECTION('',(-1.,0.,0.));
#12811=DIRECTION('',(0.,0.,1.));
#12812=DIRECTION('center_axis',(1.,0.,0.));
#12813=DIRECTION('ref_axis',(0.,1.,0.));
#12814=DIRECTION('',(0.,1.,0.));
#12815=DIRECTION('',(0.,1.,0.));
#12816=DIRECTION('',(0.,0.,1.));
#12817=DIRECTION('',(0.,1.,0.));
#12818=DIRECTION('center_axis',(0.,-1.,0.));
#12819=DIRECTION('ref_axis',(1.,0.,0.));
#12820=DIRECTION('',(1.,0.,0.));
#12821=DIRECTION('',(1.,0.,0.));
#12822=DIRECTION('',(0.,0.,1.));
#12823=DIRECTION('center_axis',(-1.,0.,0.));
#12824=DIRECTION('ref_axis',(0.,-1.,0.));
#12825=DIRECTION('',(0.,-1.,0.));
#12826=DIRECTION('',(0.,-1.,0.));
#12827=DIRECTION('',(0.,-1.,0.));
#12828=DIRECTION('center_axis',(0.,0.,1.));
#12829=DIRECTION('ref_axis',(1.,0.,0.));
#12830=DIRECTION('center_axis',(0.,0.,1.));
#12831=DIRECTION('ref_axis',(1.,0.,0.));
#12832=DIRECTION('axis',(0.,0.,1.));
#12833=DIRECTION('refdir',(1.,0.,0.));
#12834=DIRECTION('center_axis',(1.,0.,0.));
#12835=DIRECTION('ref_axis',(0.,-0.63690647534225,0.770941075353436));
#12836=DIRECTION('',(1.,0.,0.));
#12837=DIRECTION('center_axis',(-1.,0.,0.));
#12838=DIRECTION('ref_axis',(0.,-1.,0.));
#12839=DIRECTION('center_axis',(1.,0.,0.));
#12840=DIRECTION('ref_axis',(0.,-1.,0.));
#12841=DIRECTION('',(1.,0.,0.));
#12842=DIRECTION('center_axis',(1.,0.,0.));
#12843=DIRECTION('ref_axis',(0.,-0.937046398851017,-0.349204877400562));
#12844=DIRECTION('',(1.,0.,0.));
#12845=DIRECTION('center_axis',(-1.,0.,0.));
#12846=DIRECTION('ref_axis',(0.,-1.,0.));
#12847=DIRECTION('center_axis',(-1.,0.,0.));
#12848=DIRECTION('ref_axis',(0.,0.63690647534225,0.770941075353436));
#12849=DIRECTION('',(-1.,0.,0.));
#12850=DIRECTION('center_axis',(1.,0.,0.));
#12851=DIRECTION('ref_axis',(0.,1.,0.));
#12852=DIRECTION('center_axis',(-1.,0.,0.));
#12853=DIRECTION('ref_axis',(0.,1.,0.));
#12854=DIRECTION('',(-1.,0.,0.));
#12855=DIRECTION('center_axis',(-1.,0.,0.));
#12856=DIRECTION('ref_axis',(0.,0.937046398851017,-0.349204877400562));
#12857=DIRECTION('',(-1.,0.,0.));
#12858=DIRECTION('center_axis',(-1.,0.,0.));
#12859=DIRECTION('ref_axis',(0.,1.,0.));
#12860=DIRECTION('center_axis',(1.,0.,0.));
#12861=DIRECTION('ref_axis',(0.,0.923761774208712,0.382967602429726));
#12862=DIRECTION('',(1.,-1.22464679914735E-16,-1.49975978266186E-32));
#12863=DIRECTION('center_axis',(-1.,0.,0.));
#12864=DIRECTION('ref_axis',(0.,-1.,0.));
#12865=DIRECTION('center_axis',(1.,0.,0.));
#12866=DIRECTION('ref_axis',(0.,-1.,0.));
#12867=DIRECTION('',(1.,-1.22464679914735E-16,-1.49975978266186E-32));
#12868=DIRECTION('center_axis',(1.,0.,0.));
#12869=DIRECTION('ref_axis',(0.,-1.,0.));
#12870=DIRECTION('',(1.,-1.22464679914735E-16,-1.49975978266186E-32));
#12871=DIRECTION('center_axis',(1.,0.,0.));
#12872=DIRECTION('ref_axis',(0.,0.608513123927572,-0.79354380975968));
#12873=DIRECTION('',(1.,-1.22464679914735E-16,-1.49975978266186E-32));
#12874=DIRECTION('center_axis',(1.,0.,0.));
#12875=DIRECTION('ref_axis',(0.,-1.,0.));
#12876=DIRECTION('center_axis',(-1.,0.,0.));
#12877=DIRECTION('ref_axis',(0.,-0.923761774208712,0.382967602429726));
#12878=DIRECTION('',(-1.,1.22464679914735E-16,-1.49975978266186E-32));
#12879=DIRECTION('center_axis',(1.,0.,0.));
#12880=DIRECTION('ref_axis',(0.,1.,0.));
#12881=DIRECTION('center_axis',(-1.,0.,0.));
#12882=DIRECTION('ref_axis',(0.,1.,0.));
#12883=DIRECTION('',(-1.,1.22464679914735E-16,-1.49975978266186E-32));
#12884=DIRECTION('center_axis',(-1.,0.,0.));
#12885=DIRECTION('ref_axis',(0.,1.,0.));
#12886=DIRECTION('',(-1.,1.22464679914735E-16,-1.49975978266186E-32));
#12887=DIRECTION('center_axis',(-1.,0.,0.));
#12888=DIRECTION('ref_axis',(0.,-0.608513123927572,-0.79354380975968));
#12889=DIRECTION('',(-1.,1.22464679914735E-16,-1.49975978266186E-32));
#12890=DIRECTION('center_axis',(-1.,0.,0.));
#12891=DIRECTION('ref_axis',(0.,1.,0.));
#12892=DIRECTION('center_axis',(1.,0.,0.));
#12893=DIRECTION('ref_axis',(0.,1.,0.));
#12894=DIRECTION('center_axis',(1.,0.,0.));
#12895=DIRECTION('ref_axis',(0.,0.,-1.));
#12896=DIRECTION('',(0.,0.,1.));
#12897=DIRECTION('',(0.,1.,0.));
#12898=DIRECTION('center_axis',(-1.,0.,0.));
#12899=DIRECTION('ref_axis',(0.,-1.,0.));
#12900=DIRECTION('center_axis',(1.,0.,0.));
#12901=DIRECTION('ref_axis',(0.,0.,-1.));
#12902=DIRECTION('',(0.,-1.,0.));
#12903=DIRECTION('',(0.,0.,1.));
#12904=DIRECTION('center_axis',(-1.6809537598482E-15,1.,0.));
#12905=DIRECTION('ref_axis',(-1.,-1.6809537598482E-15,0.));
#12906=DIRECTION('',(-1.,0.,0.));
#12907=DIRECTION('',(0.,0.,1.));
#12908=DIRECTION('',(-1.,-1.6809537598482E-15,0.));
#12909=DIRECTION('',(0.,0.,1.));
#12910=DIRECTION('center_axis',(3.3619075196964E-16,1.,0.));
#12911=DIRECTION('ref_axis',(-1.,3.3619075196964E-16,0.));
#12912=DIRECTION('',(-1.,0.,0.));
#12913=DIRECTION('',(0.,0.,1.));
#12914=DIRECTION('',(-1.,3.3619075196964E-16,0.));
#12915=DIRECTION('',(0.,0.,1.));
#12916=DIRECTION('center_axis',(-1.,0.,0.));
#12917=DIRECTION('ref_axis',(0.,-1.,0.));
#12918=DIRECTION('center_axis',(1.,0.,0.));
#12919=DIRECTION('ref_axis',(0.,0.,-1.));
#12920=DIRECTION('',(0.,-1.,0.));
#12921=DIRECTION('center_axis',(2.35333526378748E-15,-1.,0.));
#12922=DIRECTION('ref_axis',(1.,2.35333526378748E-15,0.));
#12923=DIRECTION('',(1.,0.,0.));
#12924=DIRECTION('',(1.,2.35333526378748E-15,0.));
#12925=DIRECTION('',(0.,0.,1.));
#12926=DIRECTION('center_axis',(-3.3619075196964E-16,-1.,0.));
#12927=DIRECTION('ref_axis',(1.,-3.3619075196964E-16,0.));
#12928=DIRECTION('',(1.,0.,0.));
#12929=DIRECTION('',(0.,0.,1.));
#12930=DIRECTION('',(1.,-3.3619075196964E-16,0.));
#12931=DIRECTION('center_axis',(1.,0.,0.));
#12932=DIRECTION('ref_axis',(0.,1.,0.));
#12933=DIRECTION('center_axis',(1.,0.,0.));
#12934=DIRECTION('ref_axis',(0.,0.,-1.));
#12935=DIRECTION('',(0.,1.,0.));
#12936=DIRECTION('center_axis',(0.,0.,1.));
#12937=DIRECTION('ref_axis',(-1.,0.,0.));
#12938=DIRECTION('',(0.,-1.,0.));
#12939=DIRECTION('center_axis',(0.,0.,1.));
#12940=DIRECTION('ref_axis',(0.970931683144254,0.239356776939084,0.));
#12941=DIRECTION('',(0.,1.,0.));
#12942=DIRECTION('center_axis',(0.,0.,1.));
#12943=DIRECTION('ref_axis',(-0.970931683144254,-0.239356776939084,0.));
#12944=DIRECTION('center_axis',(0.,0.,-1.));
#12945=DIRECTION('ref_axis',(-1.,0.,0.));
#12946=DIRECTION('center_axis',(1.,0.,0.));
#12947=DIRECTION('ref_axis',(0.,0.,-1.));
#12948=DIRECTION('center_axis',(1.,0.,0.));
#12949=DIRECTION('ref_axis',(0.,0.,-1.));
#12950=DIRECTION('center_axis',(-1.,0.,0.));
#12951=DIRECTION('ref_axis',(0.,1.,0.));
#12952=DIRECTION('center_axis',(1.,0.,0.));
#12953=DIRECTION('ref_axis',(0.,-1.,0.));
#12954=DIRECTION('center_axis',(-1.,0.,0.));
#12955=DIRECTION('ref_axis',(0.,1.,0.));
#12956=DIRECTION('center_axis',(-1.,0.,0.));
#12957=DIRECTION('ref_axis',(0.,1.,0.));
#12958=DIRECTION('center_axis',(1.,0.,0.));
#12959=DIRECTION('ref_axis',(0.,1.,0.));
#12960=DIRECTION('center_axis',(-1.,0.,0.));
#12961=DIRECTION('ref_axis',(0.,1.,0.));
#12962=DIRECTION('',(-1.,0.,0.));
#12963=DIRECTION('center_axis',(-1.,0.,0.));
#12964=DIRECTION('ref_axis',(0.,1.,0.));
#12965=DIRECTION('center_axis',(-1.,0.,0.));
#12966=DIRECTION('ref_axis',(0.,1.,0.));
#12967=DIRECTION('center_axis',(1.,0.,0.));
#12968=DIRECTION('ref_axis',(0.,1.,0.));
#12969=DIRECTION('center_axis',(-1.,0.,0.));
#12970=DIRECTION('ref_axis',(0.,1.,0.));
#12971=DIRECTION('',(-1.,0.,0.));
#12972=DIRECTION('center_axis',(1.,0.,0.));
#12973=DIRECTION('ref_axis',(0.,1.22464679914735E-16,1.));
#12974=DIRECTION('',(1.,0.,0.));
#12975=DIRECTION('center_axis',(1.,0.,0.));
#12976=DIRECTION('ref_axis',(0.,0.,-1.));
#12977=DIRECTION('',(-1.,0.,0.));
#12978=DIRECTION('center_axis',(1.,0.,0.));
#12979=DIRECTION('ref_axis',(0.,0.,-1.));
#12980=DIRECTION('center_axis',(1.,0.,0.));
#12981=DIRECTION('ref_axis',(0.,0.,-1.));
#12982=DIRECTION('center_axis',(1.,0.,0.));
#12983=DIRECTION('ref_axis',(0.,0.,-1.));
#12984=DIRECTION('',(0.,-1.,0.));
#12985=DIRECTION('center_axis',(0.,0.,1.));
#12986=DIRECTION('ref_axis',(1.,0.,0.));
#12987=DIRECTION('',(0.,-1.,0.));
#12988=DIRECTION('',(1.,0.,0.));
#12989=DIRECTION('',(0.,1.,0.));
#12990=DIRECTION('',(-1.,0.,0.));
#12991=DIRECTION('center_axis',(0.,0.,-1.));
#12992=DIRECTION('ref_axis',(1.,0.,0.));
#12993=DIRECTION('center_axis',(0.,0.,-1.));
#12994=DIRECTION('ref_axis',(1.,0.,0.));
#12995=DIRECTION('center_axis',(0.,0.,-1.));
#12996=DIRECTION('ref_axis',(1.,0.,0.));
#12997=DIRECTION('center_axis',(0.,0.,-1.));
#12998=DIRECTION('ref_axis',(1.,0.,0.));
#12999=DIRECTION('center_axis',(0.,0.,-1.));
#13000=DIRECTION('ref_axis',(1.,0.,0.));
#13001=DIRECTION('',(-1.,0.,0.));
#13002=DIRECTION('',(0.,1.,0.));
#13003=DIRECTION('',(1.,0.,0.));
#13004=DIRECTION('center_axis',(0.,0.,-1.));
#13005=DIRECTION('ref_axis',(1.,0.,0.));
#13006=DIRECTION('center_axis',(0.,0.,1.));
#13007=DIRECTION('ref_axis',(1.,0.,0.));
#13008=DIRECTION('center_axis',(1.,0.,0.));
#13009=DIRECTION('ref_axis',(0.,-1.,0.));
#13010=DIRECTION('center_axis',(1.,0.,0.));
#13011=DIRECTION('ref_axis',(0.,-1.,0.));
#13012=DIRECTION('center_axis',(-1.,0.,0.));
#13013=DIRECTION('ref_axis',(0.,-1.,0.));
#13014=DIRECTION('center_axis',(1.,0.,0.));
#13015=DIRECTION('ref_axis',(0.,-1.,0.));
#13016=DIRECTION('',(1.,0.,0.));
#13017=DIRECTION('center_axis',(1.,0.,0.));
#13018=DIRECTION('ref_axis',(0.,-1.,0.));
#13019=DIRECTION('center_axis',(1.,0.,0.));
#13020=DIRECTION('ref_axis',(0.,-1.,0.));
#13021=DIRECTION('center_axis',(-1.,0.,0.));
#13022=DIRECTION('ref_axis',(0.,-1.,0.));
#13023=DIRECTION('center_axis',(1.,0.,0.));
#13024=DIRECTION('ref_axis',(0.,-1.,0.));
#13025=DIRECTION('',(1.,0.,0.));
#13026=DIRECTION('center_axis',(1.,0.,0.));
#13027=DIRECTION('ref_axis',(0.,0.,-1.));
#13028=DIRECTION('center_axis',(-1.,0.,0.));
#13029=DIRECTION('ref_axis',(0.,0.,-1.));
#13030=DIRECTION('center_axis',(-1.,0.,0.));
#13031=DIRECTION('ref_axis',(0.,1.22464679914735E-16,1.));
#13032=DIRECTION('center_axis',(0.,0.,1.));
#13033=DIRECTION('ref_axis',(1.,0.,0.));
#13034=DIRECTION('center_axis',(0.,0.,-1.));
#13035=DIRECTION('ref_axis',(1.,0.,0.));
#13036=DIRECTION('',(0.,0.,-1.));
#13037=DIRECTION('center_axis',(0.,0.,1.));
#13038=DIRECTION('ref_axis',(1.,0.,0.));
#13039=DIRECTION('center_axis',(0.,0.,-1.));
#13040=DIRECTION('ref_axis',(1.,0.,0.));
#13041=DIRECTION('',(0.,0.,-1.));
#13042=DIRECTION('center_axis',(0.,0.,1.));
#13043=DIRECTION('ref_axis',(1.,0.,0.));
#13044=DIRECTION('center_axis',(0.,0.,-1.));
#13045=DIRECTION('ref_axis',(1.,0.,0.));
#13046=DIRECTION('',(0.,0.,-1.));
#13047=DIRECTION('center_axis',(0.,0.,1.));
#13048=DIRECTION('ref_axis',(1.,0.,0.));
#13049=DIRECTION('center_axis',(0.,0.,-1.));
#13050=DIRECTION('ref_axis',(1.,0.,0.));
#13051=DIRECTION('',(0.,0.,-1.));
#13052=DIRECTION('center_axis',(0.,0.,1.));
#13053=DIRECTION('ref_axis',(1.,0.,0.));
#13054=DIRECTION('center_axis',(0.,0.,-1.));
#13055=DIRECTION('ref_axis',(1.,0.,0.));
#13056=DIRECTION('',(0.,0.,-1.));
#13057=DIRECTION('',(0.,0.,-1.));
#13058=DIRECTION('center_axis',(0.,0.,1.));
#13059=DIRECTION('ref_axis',(1.,0.,0.));
#13060=DIRECTION('center_axis',(0.,1.,0.));
#13061=DIRECTION('ref_axis',(-1.,0.,0.));
#13062=DIRECTION('',(-1.,0.,0.));
#13063=DIRECTION('',(0.,0.,1.));
#13064=DIRECTION('',(0.,0.,1.));
#13065=DIRECTION('center_axis',(1.,0.,0.));
#13066=DIRECTION('ref_axis',(0.,1.,0.));
#13067=DIRECTION('',(0.,1.,0.));
#13068=DIRECTION('',(0.,0.,1.));
#13069=DIRECTION('center_axis',(0.,-1.,0.));
#13070=DIRECTION('ref_axis',(1.,0.,0.));
#13071=DIRECTION('',(1.,0.,0.));
#13072=DIRECTION('',(0.,0.,1.));
#13073=DIRECTION('center_axis',(-1.,0.,0.));
#13074=DIRECTION('ref_axis',(0.,-1.,0.));
#13075=DIRECTION('',(0.,-1.,0.));
#13076=DIRECTION('center_axis',(0.,0.,1.));
#13077=DIRECTION('ref_axis',(1.,0.,0.));
#13078=DIRECTION('axis',(0.,0.,1.));
#13079=DIRECTION('refdir',(1.,0.,0.));
#13080=DIRECTION('center_axis',(0.,0.,1.));
#13081=DIRECTION('ref_axis',(1.,0.,0.));
#13082=DIRECTION('center_axis',(0.,0.,1.));
#13083=DIRECTION('ref_axis',(1.,0.,0.));
#13084=DIRECTION('center_axis',(0.,0.,1.));
#13085=DIRECTION('ref_axis',(1.,0.,0.));
#13086=DIRECTION('center_axis',(0.,0.,1.));
#13087=DIRECTION('ref_axis',(1.,0.,0.));
#13088=DIRECTION('',(0.,0.,-1.));
#13089=DIRECTION('center_axis',(0.,0.,1.));
#13090=DIRECTION('ref_axis',(1.,0.,0.));
#13091=DIRECTION('center_axis',(0.,0.,1.));
#13092=DIRECTION('ref_axis',(1.,0.,0.));
#13093=DIRECTION('center_axis',(0.,0.,-1.));
#13094=DIRECTION('ref_axis',(1.,0.,0.));
#13095=DIRECTION('center_axis',(0.,0.,1.));
#13096=DIRECTION('ref_axis',(1.,0.,0.));
#13097=DIRECTION('center_axis',(0.,0.,-1.));
#13098=DIRECTION('ref_axis',(1.,0.,0.));
#13099=DIRECTION('',(0.,0.,-1.));
#13100=DIRECTION('center_axis',(0.,0.,1.));
#13101=DIRECTION('ref_axis',(1.,0.,0.));
#13102=DIRECTION('center_axis',(0.,0.,1.));
#13103=DIRECTION('ref_axis',(1.,0.,0.));
#13104=DIRECTION('',(0.,0.,-1.));
#13105=DIRECTION('center_axis',(0.,0.,1.));
#13106=DIRECTION('ref_axis',(1.,0.,0.));
#13107=DIRECTION('axis',(0.,0.,1.));
#13108=DIRECTION('refdir',(1.,0.,0.));
#13109=DIRECTION('center_axis',(0.,0.,-1.));
#13110=DIRECTION('ref_axis',(1.,0.,0.));
#13111=DIRECTION('',(0.,0.,-1.));
#13112=DIRECTION('center_axis',(0.,0.,1.));
#13113=DIRECTION('ref_axis',(1.,0.,0.));
#13114=DIRECTION('',(0.,0.,-1.));
#13115=DIRECTION('center_axis',(0.,0.,1.));
#13116=DIRECTION('ref_axis',(1.,0.,0.));
#13117=DIRECTION('center_axis',(0.,0.,-1.));
#13118=DIRECTION('ref_axis',(1.,0.,0.));
#13119=DIRECTION('',(0.,0.,-1.));
#13120=DIRECTION('center_axis',(0.,0.,-1.));
#13121=DIRECTION('ref_axis',(1.,0.,0.));
#13122=DIRECTION('',(0.,0.,-1.));
#13123=DIRECTION('center_axis',(0.,0.,-1.));
#13124=DIRECTION('ref_axis',(1.,0.,0.));
#13125=DIRECTION('',(0.,0.,-1.));
#13126=DIRECTION('center_axis',(0.,0.,-1.));
#13127=DIRECTION('ref_axis',(1.,0.,0.));
#13128=DIRECTION('',(0.,0.,-1.));
#13129=DIRECTION('center_axis',(0.,0.,-1.));
#13130=DIRECTION('ref_axis',(1.,0.,0.));
#13131=DIRECTION('',(0.,0.,-1.));
#13132=DIRECTION('center_axis',(0.,0.,-1.));
#13133=DIRECTION('ref_axis',(1.,0.,0.));
#13134=DIRECTION('',(0.,0.,-1.));
#13135=DIRECTION('center_axis',(0.,0.,-1.));
#13136=DIRECTION('ref_axis',(1.,0.,0.));
#13137=DIRECTION('',(0.,0.,-1.));
#13138=DIRECTION('center_axis',(0.,0.,-1.));
#13139=DIRECTION('ref_axis',(1.,0.,0.));
#13140=DIRECTION('',(0.,0.,-1.));
#13141=DIRECTION('center_axis',(0.,0.,-1.));
#13142=DIRECTION('ref_axis',(1.,0.,0.));
#13143=DIRECTION('',(0.,0.,-1.));
#13144=DIRECTION('center_axis',(0.,0.,-1.));
#13145=DIRECTION('ref_axis',(1.,0.,0.));
#13146=DIRECTION('',(0.,0.,-1.));
#13147=DIRECTION('center_axis',(0.,0.,-1.));
#13148=DIRECTION('ref_axis',(0.938437868794217,-0.345448066158965,0.));
#13149=DIRECTION('',(0.,0.,-1.));
#13150=DIRECTION('center_axis',(0.,0.,-1.));
#13151=DIRECTION('ref_axis',(1.,0.,0.));
#13152=DIRECTION('center_axis',(0.,0.,-1.));
#13153=DIRECTION('ref_axis',(0.45014995938304,0.892952974163504,0.));
#13154=DIRECTION('',(1.22464679914735E-16,-8.10900634611207E-30,-1.));
#13155=DIRECTION('center_axis',(0.,0.,1.));
#13156=DIRECTION('ref_axis',(1.,-6.60925970975535E-14,0.));
#13157=DIRECTION('center_axis',(0.,0.,-1.));
#13158=DIRECTION('ref_axis',(1.,-6.60925970975535E-14,0.));
#13159=DIRECTION('',(1.22464679914735E-16,-8.10900634611207E-30,-1.));
#13160=DIRECTION('center_axis',(0.,0.,-1.));
#13161=DIRECTION('ref_axis',(1.,-6.60925970975535E-14,0.));
#13162=DIRECTION('',(1.22464679914735E-16,-8.10900634611207E-30,-1.));
#13163=DIRECTION('center_axis',(0.,0.,-1.));
#13164=DIRECTION('ref_axis',(1.,-6.60925970975535E-14,0.));
#13165=DIRECTION('',(1.22464679914735E-16,-8.10900634611207E-30,-1.));
#13166=DIRECTION('center_axis',(0.,0.,-1.));
#13167=DIRECTION('ref_axis',(1.,-6.60925970975535E-14,0.));
#13168=DIRECTION('',(1.22464679914735E-16,-8.10900634611207E-30,-1.));
#13169=DIRECTION('center_axis',(0.,0.,-1.));
#13170=DIRECTION('ref_axis',(1.,-6.60925970975535E-14,0.));
#13171=DIRECTION('',(1.22464679914735E-16,-8.10900634611207E-30,-1.));
#13172=DIRECTION('center_axis',(0.,0.,-1.));
#13173=DIRECTION('ref_axis',(1.,-6.60925970975535E-14,0.));
#13174=DIRECTION('',(1.22464679914735E-16,-8.10900634611207E-30,-1.));
#13175=DIRECTION('center_axis',(0.,0.,-1.));
#13176=DIRECTION('ref_axis',(1.,-6.60925970975535E-14,0.));
#13177=DIRECTION('',(1.22464679914735E-16,-8.10900634611207E-30,-1.));
#13178=DIRECTION('center_axis',(0.,0.,-1.));
#13179=DIRECTION('ref_axis',(1.,-6.60925970975535E-14,0.));
#13180=DIRECTION('',(1.22464679914735E-16,-8.10900634611207E-30,-1.));
#13181=DIRECTION('center_axis',(0.,0.,-1.));
#13182=DIRECTION('ref_axis',(1.,-6.60925970975535E-14,0.));
#13183=DIRECTION('',(1.22464679914735E-16,-8.10900634611207E-30,-1.));
#13184=DIRECTION('center_axis',(0.,0.,-1.));
#13185=DIRECTION('ref_axis',(1.,-6.60925970975535E-14,0.));
#13186=DIRECTION('',(1.22464679914735E-16,-8.10900634611207E-30,-1.));
#13187=DIRECTION('center_axis',(0.,0.,-1.));
#13188=DIRECTION('ref_axis',(1.,-6.60925970975535E-14,0.));
#13189=DIRECTION('',(1.22464679914735E-16,-8.10900634611207E-30,-1.));
#13190=DIRECTION('center_axis',(0.,0.,-1.));
#13191=DIRECTION('ref_axis',(-0.609343205350381,-0.792906588504171,0.));
#13192=DIRECTION('',(1.22464679914735E-16,-8.10900634611207E-30,-1.));
#13193=DIRECTION('center_axis',(0.,0.,-1.));
#13194=DIRECTION('ref_axis',(1.,-6.60925970975535E-14,0.));
#13195=DIRECTION('center_axis',(0.,0.,-1.));
#13196=DIRECTION('ref_axis',(-0.348549200809368,0.937290485716755,0.));
#13197=DIRECTION('',(0.,0.,-1.));
#13198=DIRECTION('center_axis',(0.,0.,-1.));
#13199=DIRECTION('ref_axis',(1.,0.,0.));
#13200=DIRECTION('center_axis',(0.,0.,-1.));
#13201=DIRECTION('ref_axis',(1.,0.,0.));
#13202=DIRECTION('',(0.,0.,-1.));
#13203=DIRECTION('center_axis',(0.,0.,-1.));
#13204=DIRECTION('ref_axis',(1.,0.,0.));
#13205=DIRECTION('',(0.,0.,-1.));
#13206=DIRECTION('center_axis',(0.,0.,-1.));
#13207=DIRECTION('ref_axis',(1.,0.,0.));
#13208=DIRECTION('',(0.,0.,-1.));
#13209=DIRECTION('center_axis',(0.,0.,-1.));
#13210=DIRECTION('ref_axis',(1.,0.,0.));
#13211=DIRECTION('',(0.,0.,-1.));
#13212=DIRECTION('center_axis',(0.,0.,-1.));
#13213=DIRECTION('ref_axis',(1.,0.,0.));
#13214=DIRECTION('',(0.,0.,-1.));
#13215=DIRECTION('center_axis',(0.,0.,-1.));
#13216=DIRECTION('ref_axis',(1.,0.,0.));
#13217=DIRECTION('',(0.,0.,-1.));
#13218=DIRECTION('center_axis',(0.,0.,-1.));
#13219=DIRECTION('ref_axis',(0.93737235570927,-0.348328963412538,0.));
#13220=DIRECTION('',(0.,0.,-1.));
#13221=DIRECTION('center_axis',(0.,0.,-1.));
#13222=DIRECTION('ref_axis',(1.,0.,0.));
#13223=DIRECTION('center_axis',(0.,0.,-1.));
#13224=DIRECTION('ref_axis',(-0.348549399150009,0.937290411960011,0.));
#13225=DIRECTION('',(0.,0.,-1.));
#13226=DIRECTION('center_axis',(0.,0.,-1.));
#13227=DIRECTION('ref_axis',(1.,0.,0.));
#13228=DIRECTION('center_axis',(0.,0.,-1.));
#13229=DIRECTION('ref_axis',(1.,0.,0.));
#13230=DIRECTION('',(0.,0.,-1.));
#13231=DIRECTION('center_axis',(0.,0.,-1.));
#13232=DIRECTION('ref_axis',(1.,0.,0.));
#13233=DIRECTION('',(0.,0.,-1.));
#13234=DIRECTION('center_axis',(0.,0.,-1.));
#13235=DIRECTION('ref_axis',(1.,0.,0.));
#13236=DIRECTION('',(0.,0.,-1.));
#13237=DIRECTION('center_axis',(0.,0.,-1.));
#13238=DIRECTION('ref_axis',(1.,0.,0.));
#13239=DIRECTION('',(0.,0.,-1.));
#13240=DIRECTION('center_axis',(0.,0.,-1.));
#13241=DIRECTION('ref_axis',(1.,0.,0.));
#13242=DIRECTION('',(0.,0.,-1.));
#13243=DIRECTION('center_axis',(0.,0.,-1.));
#13244=DIRECTION('ref_axis',(1.,0.,0.));
#13245=DIRECTION('',(0.,0.,-1.));
#13246=DIRECTION('center_axis',(0.,0.,-1.));
#13247=DIRECTION('ref_axis',(0.937372370252713,-0.348328924275332,0.));
#13248=DIRECTION('',(0.,0.,-1.));
#13249=DIRECTION('center_axis',(0.,0.,-1.));
#13250=DIRECTION('ref_axis',(1.,0.,0.));
#13251=DIRECTION('center_axis',(0.,0.,-1.));
#13252=DIRECTION('ref_axis',(0.793241641674985,0.608906969834288,0.));
#13253=DIRECTION('',(1.22464679914735E-16,-2.74659599554882E-30,-1.));
#13254=DIRECTION('center_axis',(0.,0.,1.));
#13255=DIRECTION('ref_axis',(1.,-2.23051936250031E-14,0.));
#13256=DIRECTION('center_axis',(0.,0.,-1.));
#13257=DIRECTION('ref_axis',(1.,-2.23051936250031E-14,0.));
#13258=DIRECTION('',(1.22464679914735E-16,-2.74659599554882E-30,-1.));
#13259=DIRECTION('center_axis',(0.,0.,-1.));
#13260=DIRECTION('ref_axis',(1.,-2.23051936250031E-14,0.));
#13261=DIRECTION('',(1.22464679914735E-16,-2.74659599554882E-30,-1.));
#13262=DIRECTION('center_axis',(0.,0.,-1.));
#13263=DIRECTION('ref_axis',(1.,-2.23051936250031E-14,0.));
#13264=DIRECTION('',(1.22464679914735E-16,-2.74659599554882E-30,-1.));
#13265=DIRECTION('center_axis',(0.,0.,-1.));
#13266=DIRECTION('ref_axis',(1.,-2.23051936250031E-14,0.));
#13267=DIRECTION('',(1.22464679914735E-16,-2.74659599554882E-30,-1.));
#13268=DIRECTION('center_axis',(0.,0.,-1.));
#13269=DIRECTION('ref_axis',(1.,-2.23051936250031E-14,0.));
#13270=DIRECTION('',(1.22464679914735E-16,-2.74659599554882E-30,-1.));
#13271=DIRECTION('center_axis',(0.,0.,-1.));
#13272=DIRECTION('ref_axis',(1.,-2.23051936250031E-14,0.));
#13273=DIRECTION('',(1.22464679914735E-16,-2.74659599554882E-30,-1.));
#13274=DIRECTION('center_axis',(0.,0.,-1.));
#13275=DIRECTION('ref_axis',(-0.609084174586186,-0.793105584565299,0.));
#13276=DIRECTION('',(1.22464679914735E-16,-2.74659599554882E-30,-1.));
#13277=DIRECTION('center_axis',(0.,0.,-1.));
#13278=DIRECTION('ref_axis',(1.,-2.23051936250031E-14,0.));
#13279=DIRECTION('center_axis',(0.,0.,-1.));
#13280=DIRECTION('ref_axis',(0.793241683023816,0.608906915967904,0.));
#13281=DIRECTION('',(1.22464679914735E-16,-2.65847991820295E-30,-1.));
#13282=DIRECTION('center_axis',(0.,0.,1.));
#13283=DIRECTION('ref_axis',(1.,-2.15856712500031E-14,0.));
#13284=DIRECTION('center_axis',(0.,0.,-1.));
#13285=DIRECTION('ref_axis',(1.,-2.15856712500031E-14,0.));
#13286=DIRECTION('',(1.22464679914735E-16,-2.65847991820295E-30,-1.));
#13287=DIRECTION('center_axis',(0.,0.,-1.));
#13288=DIRECTION('ref_axis',(1.,-2.15856712500031E-14,0.));
#13289=DIRECTION('',(1.22464679914735E-16,-2.65847991820295E-30,-1.));
#13290=DIRECTION('center_axis',(0.,0.,-1.));
#13291=DIRECTION('ref_axis',(1.,-2.15856712500031E-14,0.));
#13292=DIRECTION('',(1.22464679914735E-16,-2.65847991820295E-30,-1.));
#13293=DIRECTION('center_axis',(0.,0.,-1.));
#13294=DIRECTION('ref_axis',(1.,-2.15856712500031E-14,0.));
#13295=DIRECTION('',(1.22464679914735E-16,-2.65847991820295E-30,-1.));
#13296=DIRECTION('center_axis',(0.,0.,-1.));
#13297=DIRECTION('ref_axis',(1.,-2.15856712500031E-14,0.));
#13298=DIRECTION('',(1.22464679914735E-16,-2.65847991820295E-30,-1.));
#13299=DIRECTION('center_axis',(0.,0.,-1.));
#13300=DIRECTION('ref_axis',(1.,-2.15856712500031E-14,0.));
#13301=DIRECTION('',(1.22464679914735E-16,-2.65847991820295E-30,-1.));
#13302=DIRECTION('center_axis',(0.,0.,-1.));
#13303=DIRECTION('ref_axis',(-0.609084235810543,-0.793105537546604,0.));
#13304=DIRECTION('',(1.22464679914735E-16,-2.65847991820295E-30,-1.));
#13305=DIRECTION('center_axis',(0.,0.,-1.));
#13306=DIRECTION('ref_axis',(1.,-2.15856712500031E-14,0.));
#13307=DIRECTION('center_axis',(0.,0.,-1.));
#13308=DIRECTION('ref_axis',(1.,-2.15856712500031E-14,0.));
#13309=DIRECTION('center_axis',(0.,0.,1.));
#13310=DIRECTION('ref_axis',(1.,0.,0.));
#13311=DIRECTION('center_axis',(0.,0.,1.));
#13312=DIRECTION('ref_axis',(1.,0.,0.));
#13313=DIRECTION('',(1.,0.,0.));
#13314=DIRECTION('',(0.,-1.,0.));
#13315=DIRECTION('',(-1.,0.,0.));
#13316=DIRECTION('',(0.,1.,0.));
#13317=DIRECTION('',(1.,0.,0.));
#13318=DIRECTION('center_axis',(0.,0.,-1.));
#13319=DIRECTION('ref_axis',(1.,-2.23051936250031E-14,0.));
#13320=DIRECTION('center_axis',(0.,0.,-1.));
#13321=DIRECTION('ref_axis',(1.,0.,0.));
#13322=DIRECTION('center_axis',(0.,0.,-1.));
#13323=DIRECTION('ref_axis',(1.,0.,0.));
#13324=DIRECTION('center_axis',(0.,0.,1.));
#13325=DIRECTION('ref_axis',(1.,0.,0.));
#13326=DIRECTION('center_axis',(0.,0.,-1.));
#13327=DIRECTION('ref_axis',(1.,-6.60925970975535E-14,0.));
#13328=DIRECTION('center_axis',(0.,0.,-1.));
#13329=DIRECTION('ref_axis',(1.,0.,0.));
#13330=DIRECTION('center_axis',(0.,0.,-1.));
#13331=DIRECTION('ref_axis',(1.,0.,0.));
#13332=DIRECTION('center_axis',(0.,0.,1.));
#13333=DIRECTION('ref_axis',(1.,0.,0.));
#13334=DIRECTION('center_axis',(0.,0.,1.));
#13335=DIRECTION('ref_axis',(1.,0.,0.));
#13336=DIRECTION('center_axis',(-1.22464679914735E-16,1.,0.));
#13337=DIRECTION('ref_axis',(-1.,-1.22464679914735E-16,0.));
#13338=DIRECTION('center_axis',(0.,0.,-1.));
#13339=DIRECTION('ref_axis',(1.,0.,0.));
#13340=DIRECTION('center_axis',(0.,0.,1.));
#13341=DIRECTION('ref_axis',(1.,0.,0.));
#13342=DIRECTION('',(0.,0.,-1.));
#13343=DIRECTION('center_axis',(0.,0.,1.));
#13344=DIRECTION('ref_axis',(1.,0.,0.));
#13345=DIRECTION('center_axis',(0.,0.,1.));
#13346=DIRECTION('ref_axis',(1.,0.,0.));
#13347=DIRECTION('center_axis',(-1.22464679914735E-16,1.,0.));
#13348=DIRECTION('ref_axis',(-1.,-1.22464679914735E-16,0.));
#13349=DIRECTION('center_axis',(0.,0.,-1.));
#13350=DIRECTION('ref_axis',(1.,0.,0.));
#13351=DIRECTION('center_axis',(0.,0.,1.));
#13352=DIRECTION('ref_axis',(1.,0.,0.));
#13353=DIRECTION('',(0.,0.,-1.));
#13354=DIRECTION('center_axis',(0.,0.,-1.));
#13355=DIRECTION('ref_axis',(1.,0.,0.));
#13356=DIRECTION('center_axis',(0.,0.,1.));
#13357=DIRECTION('ref_axis',(1.,0.,0.));
#13358=DIRECTION('center_axis',(0.,0.,1.));
#13359=DIRECTION('ref_axis',(1.,0.,0.));
#13360=DIRECTION('center_axis',(0.,0.,1.));
#13361=DIRECTION('ref_axis',(1.,0.,0.));
#13362=DIRECTION('center_axis',(0.,0.,1.));
#13363=DIRECTION('ref_axis',(1.,0.,0.));
#13364=DIRECTION('center_axis',(0.,0.,1.));
#13365=DIRECTION('ref_axis',(1.,0.,0.));
#13366=DIRECTION('center_axis',(0.,0.,-1.));
#13367=DIRECTION('ref_axis',(1.,0.,0.));
#13368=DIRECTION('center_axis',(0.,0.,1.));
#13369=DIRECTION('ref_axis',(1.,0.,0.));
#13370=DIRECTION('',(0.,0.,-1.));
#13371=DIRECTION('center_axis',(0.,0.,1.));
#13372=DIRECTION('ref_axis',(1.,0.,0.));
#13373=DIRECTION('',(0.,0.,-1.));
#13374=DIRECTION('center_axis',(0.,-1.,0.));
#13375=DIRECTION('ref_axis',(1.,0.,0.));
#13376=DIRECTION('',(0.,0.,1.));
#13377=DIRECTION('',(0.,0.,1.));
#13378=DIRECTION('',(1.,0.,0.));
#13379=DIRECTION('center_axis',(0.,1.,0.));
#13380=DIRECTION('ref_axis',(-1.,0.,0.));
#13381=DIRECTION('',(0.,0.,1.));
#13382=DIRECTION('',(-1.,0.,0.));
#13383=DIRECTION('',(0.,0.,1.));
#13384=DIRECTION('center_axis',(1.,0.,0.));
#13385=DIRECTION('ref_axis',(0.,1.,0.));
#13386=DIRECTION('',(0.,1.,0.));
#13387=DIRECTION('center_axis',(0.,-1.,0.));
#13388=DIRECTION('ref_axis',(1.,0.,0.));
#13389=DIRECTION('',(0.,0.,-1.));
#13390=DIRECTION('',(1.,0.,0.));
#13391=DIRECTION('',(0.,0.,1.));
#13392=DIRECTION('center_axis',(-1.,0.,0.));
#13393=DIRECTION('ref_axis',(0.,-1.,0.));
#13394=DIRECTION('',(0.,-1.,0.));
#13395=DIRECTION('center_axis',(0.,0.,1.));
#13396=DIRECTION('ref_axis',(-1.83697019872103E-16,-1.,0.));
#13397=DIRECTION('center_axis',(0.,0.,1.));
#13398=DIRECTION('ref_axis',(1.,0.,0.));
#13399=DIRECTION('center_axis',(0.,0.,1.));
#13400=DIRECTION('ref_axis',(1.,0.,0.));
#13401=DIRECTION('center_axis',(0.,0.,1.));
#13402=DIRECTION('ref_axis',(1.,0.,0.));
#13403=DIRECTION('',(0.,0.,-1.));
#13404=DIRECTION('center_axis',(0.,0.,1.));
#13405=DIRECTION('ref_axis',(1.,0.,0.));
#13406=DIRECTION('center_axis',(0.,0.,1.));
#13407=DIRECTION('ref_axis',(1.,0.,0.));
#13408=DIRECTION('axis',(0.,0.,1.));
#13409=DIRECTION('refdir',(1.,0.,0.));
#13410=DIRECTION('center_axis',(0.,0.,1.));
#13411=DIRECTION('ref_axis',(1.,0.,0.));
#13412=DIRECTION('center_axis',(0.,0.,-1.));
#13413=DIRECTION('ref_axis',(1.,0.,0.));
#13414=DIRECTION('center_axis',(1.22464679914735E-16,-1.,0.));
#13415=DIRECTION('ref_axis',(-1.,-1.22464679914735E-16,0.));
#13416=DIRECTION('center_axis',(0.,0.,1.));
#13417=DIRECTION('ref_axis',(1.,0.,0.));
#13418=DIRECTION('center_axis',(0.,0.,1.));
#13419=DIRECTION('ref_axis',(1.,0.,0.));
#13420=DIRECTION('',(0.,0.,-1.));
#13421=DIRECTION('center_axis',(0.,0.,-1.));
#13422=DIRECTION('ref_axis',(1.,0.,0.));
#13423=DIRECTION('center_axis',(0.,0.,1.));
#13424=DIRECTION('ref_axis',(1.,0.,0.));
#13425=DIRECTION('center_axis',(0.,0.,-1.));
#13426=DIRECTION('ref_axis',(1.,0.,0.));
#13427=DIRECTION('center_axis',(0.,0.,1.));
#13428=DIRECTION('ref_axis',(1.,0.,0.));
#13429=DIRECTION('center_axis',(1.22464679914735E-16,-1.,0.));
#13430=DIRECTION('ref_axis',(-1.,-1.22464679914735E-16,0.));
#13431=DIRECTION('center_axis',(0.,0.,1.));
#13432=DIRECTION('ref_axis',(1.,0.,0.));
#13433=DIRECTION('center_axis',(0.,0.,1.));
#13434=DIRECTION('ref_axis',(1.,0.,0.));
#13435=DIRECTION('center_axis',(0.,0.,1.));
#13436=DIRECTION('ref_axis',(1.,0.,0.));
#13437=DIRECTION('center_axis',(0.,0.,-1.));
#13438=DIRECTION('ref_axis',(1.,0.,0.));
#13439=DIRECTION('center_axis',(0.,0.,-1.));
#13440=DIRECTION('ref_axis',(1.,0.,0.));
#13441=DIRECTION('center_axis',(0.,0.,1.));
#13442=DIRECTION('ref_axis',(1.,0.,0.));
#13443=DIRECTION('center_axis',(0.,0.,-1.));
#13444=DIRECTION('ref_axis',(1.,0.,0.));
#13445=DIRECTION('',(0.,0.,-1.));
#13446=DIRECTION('center_axis',(0.,0.,1.));
#13447=DIRECTION('ref_axis',(1.,0.,0.));
#13448=DIRECTION('center_axis',(0.,0.,-1.));
#13449=DIRECTION('ref_axis',(1.,0.,0.));
#13450=DIRECTION('center_axis',(0.,0.,-1.));
#13451=DIRECTION('ref_axis',(1.,0.,0.));
#13452=DIRECTION('center_axis',(0.,0.,1.));
#13453=DIRECTION('ref_axis',(1.,0.,0.));
#13454=DIRECTION('',(0.,0.,-1.));
#13455=DIRECTION('center_axis',(0.,0.,1.));
#13456=DIRECTION('ref_axis',(1.,0.,0.));
#13457=DIRECTION('',(0.,0.,-1.));
#13458=DIRECTION('center_axis',(0.,0.,-1.));
#13459=DIRECTION('ref_axis',(1.,0.,0.));
#13460=DIRECTION('center_axis',(0.,0.,1.));
#13461=DIRECTION('ref_axis',(1.,0.,0.));
#13462=DIRECTION('',(0.,0.,-1.));
#13463=DIRECTION('center_axis',(0.,0.,1.));
#13464=DIRECTION('ref_axis',(1.,0.,0.));
#13465=DIRECTION('center_axis',(0.,0.,1.));
#13466=DIRECTION('ref_axis',(1.,0.,0.));
#13467=DIRECTION('axis',(0.,0.,1.));
#13468=DIRECTION('refdir',(1.,0.,0.));
#13469=DIRECTION('center_axis',(0.,0.,-1.));
#13470=DIRECTION('ref_axis',(1.,0.,0.));
#13471=DIRECTION('center_axis',(0.,0.,-1.));
#13472=DIRECTION('ref_axis',(1.,0.,0.));
#13473=DIRECTION('',(0.,0.,-1.));
#13474=DIRECTION('center_axis',(0.,0.,1.));
#13475=DIRECTION('ref_axis',(1.,0.,0.));
#13476=DIRECTION('center_axis',(0.,0.,-1.));
#13477=DIRECTION('ref_axis',(1.,0.,0.));
#13478=DIRECTION('center_axis',(0.,0.,-1.));
#13479=DIRECTION('ref_axis',(1.,0.,0.));
#13480=DIRECTION('',(0.,0.,-1.));
#13481=DIRECTION('center_axis',(0.,0.,1.));
#13482=DIRECTION('ref_axis',(1.,0.,0.));
#13483=DIRECTION('center_axis',(0.,1.,0.));
#13484=DIRECTION('ref_axis',(-1.,0.,0.));
#13485=DIRECTION('',(-1.,0.,0.));
#13486=DIRECTION('',(0.,0.,1.));
#13487=DIRECTION('',(-1.,0.,0.));
#13488=DIRECTION('',(0.,0.,1.));
#13489=DIRECTION('center_axis',(1.,0.,0.));
#13490=DIRECTION('ref_axis',(0.,1.,0.));
#13491=DIRECTION('',(0.,1.,0.));
#13492=DIRECTION('',(0.,1.,0.));
#13493=DIRECTION('',(0.,0.,1.));
#13494=DIRECTION('center_axis',(0.,-1.,0.));
#13495=DIRECTION('ref_axis',(1.,0.,0.));
#13496=DIRECTION('',(1.,0.,0.));
#13497=DIRECTION('',(1.,0.,0.));
#13498=DIRECTION('',(0.,0.,1.));
#13499=DIRECTION('center_axis',(-1.,0.,0.));
#13500=DIRECTION('ref_axis',(0.,-1.,0.));
#13501=DIRECTION('',(0.,-1.,0.));
#13502=DIRECTION('',(0.,-1.,0.));
#13503=DIRECTION('center_axis',(0.,0.,1.));
#13504=DIRECTION('ref_axis',(1.,0.,0.));
#13505=DIRECTION('center_axis',(0.,0.,1.));
#13506=DIRECTION('ref_axis',(1.,0.,0.));
#13507=DIRECTION('axis',(0.,0.,1.));
#13508=DIRECTION('refdir',(1.,0.,0.));
#13509=DIRECTION('center_axis',(0.,0.,-1.));
#13510=DIRECTION('ref_axis',(-1.,0.,0.));
#13511=DIRECTION('center_axis',(7.34788079488412E-16,0.,-1.));
#13512=DIRECTION('ref_axis',(-1.,0.,-7.34788079488412E-16));
#13513=DIRECTION('center_axis',(-7.34788079488412E-16,0.,1.));
#13514=DIRECTION('ref_axis',(1.,0.,7.34788079488412E-16));
#13515=DIRECTION('center_axis',(0.,0.,1.));
#13516=DIRECTION('ref_axis',(1.,0.,0.));
#13517=DIRECTION('axis',(0.,0.,1.));
#13518=DIRECTION('refdir',(1.,0.,0.));
#13519=DIRECTION('center_axis',(0.,0.,1.));
#13520=DIRECTION('ref_axis',(-1.,0.,0.));
#13521=DIRECTION('',(0.,0.,1.));
#13522=DIRECTION('center_axis',(0.,0.,-1.));
#13523=DIRECTION('ref_axis',(-1.,0.,0.));
#13524=DIRECTION('',(0.,0.,1.));
#13525=DIRECTION('center_axis',(0.,0.,-1.));
#13526=DIRECTION('ref_axis',(-1.,0.,0.));
#13527=DIRECTION('center_axis',(0.,0.,1.));
#13528=DIRECTION('ref_axis',(-1.,0.,0.));
#13529=DIRECTION('',(0.,0.,1.));
#13530=DIRECTION('center_axis',(0.,0.,1.));
#13531=DIRECTION('ref_axis',(-1.,0.,0.));
#13532=DIRECTION('',(0.,0.,1.));
#13533=DIRECTION('center_axis',(0.,0.,1.));
#13534=DIRECTION('ref_axis',(-1.,0.,0.));
#13535=DIRECTION('',(0.,0.,1.));
#13536=DIRECTION('center_axis',(0.,0.,1.));
#13537=DIRECTION('ref_axis',(-1.,0.,0.));
#13538=DIRECTION('',(0.,0.,1.));
#13539=DIRECTION('center_axis',(0.,0.,1.));
#13540=DIRECTION('ref_axis',(-1.,0.,0.));
#13541=DIRECTION('',(0.,0.,1.));
#13542=DIRECTION('center_axis',(0.,0.,1.));
#13543=DIRECTION('ref_axis',(-1.,0.,0.));
#13544=DIRECTION('',(0.,0.,1.));
#13545=DIRECTION('center_axis',(0.,0.,1.));
#13546=DIRECTION('ref_axis',(-1.,0.,0.));
#13547=DIRECTION('',(0.,0.,1.));
#13548=DIRECTION('center_axis',(0.,0.,1.));
#13549=DIRECTION('ref_axis',(-1.,0.,0.));
#13550=DIRECTION('',(0.,0.,1.));
#13551=DIRECTION('center_axis',(0.,0.,1.));
#13552=DIRECTION('ref_axis',(-1.,0.,0.));
#13553=DIRECTION('',(0.,0.,1.));
#13554=DIRECTION('center_axis',(0.,0.,1.));
#13555=DIRECTION('ref_axis',(-1.,0.,0.));
#13556=DIRECTION('',(0.,0.,1.));
#13557=DIRECTION('center_axis',(0.,0.,1.));
#13558=DIRECTION('ref_axis',(-0.938434237953747,-0.345457929473576,0.));
#13559=DIRECTION('',(0.,0.,1.));
#13560=DIRECTION('center_axis',(0.,0.,-1.));
#13561=DIRECTION('ref_axis',(-1.,0.,0.));
#13562=DIRECTION('center_axis',(0.,0.,1.));
#13563=DIRECTION('ref_axis',(-0.450135889590755,0.892960066801612,0.));
#13564=DIRECTION('',(-1.22464679914735E-16,-7.02543712147503E-30,1.));
#13565=DIRECTION('center_axis',(0.,0.,-1.));
#13566=DIRECTION('ref_axis',(-1.,-5.72445829159016E-14,0.));
#13567=DIRECTION('center_axis',(0.,0.,1.));
#13568=DIRECTION('ref_axis',(-1.,-5.72445829159016E-14,0.));
#13569=DIRECTION('',(-1.22464679914735E-16,-7.02543712147503E-30,1.));
#13570=DIRECTION('center_axis',(0.,0.,1.));
#13571=DIRECTION('ref_axis',(-1.,-5.72445829159016E-14,0.));
#13572=DIRECTION('',(-1.22464679914735E-16,-7.02543712147503E-30,1.));
#13573=DIRECTION('center_axis',(0.,0.,1.));
#13574=DIRECTION('ref_axis',(-1.,-5.72445829159016E-14,0.));
#13575=DIRECTION('',(-1.22464679914735E-16,-7.02543712147503E-30,1.));
#13576=DIRECTION('center_axis',(0.,0.,1.));
#13577=DIRECTION('ref_axis',(-1.,-5.72445829159016E-14,0.));
#13578=DIRECTION('',(-1.22464679914735E-16,-7.02543712147503E-30,1.));
#13579=DIRECTION('center_axis',(0.,0.,1.));
#13580=DIRECTION('ref_axis',(-1.,-5.72445829159016E-14,0.));
#13581=DIRECTION('',(-1.22464679914735E-16,-7.02543712147503E-30,1.));
#13582=DIRECTION('center_axis',(0.,0.,1.));
#13583=DIRECTION('ref_axis',(-1.,-5.72445829159016E-14,0.));
#13584=DIRECTION('',(-1.22464679914735E-16,-7.02543712147503E-30,1.));
#13585=DIRECTION('center_axis',(0.,0.,1.));
#13586=DIRECTION('ref_axis',(-1.,-5.72445829159016E-14,0.));
#13587=DIRECTION('',(-1.22464679914735E-16,-7.02543712147503E-30,1.));
#13588=DIRECTION('center_axis',(0.,0.,1.));
#13589=DIRECTION('ref_axis',(-1.,-5.72445829159016E-14,0.));
#13590=DIRECTION('',(-1.22464679914735E-16,-7.02543712147503E-30,1.));
#13591=DIRECTION('center_axis',(0.,0.,1.));
#13592=DIRECTION('ref_axis',(-1.,-5.72445829159016E-14,0.));
#13593=DIRECTION('',(-1.22464679914735E-16,-7.02543712147503E-30,1.));
#13594=DIRECTION('center_axis',(0.,0.,1.));
#13595=DIRECTION('ref_axis',(-1.,-5.72445829159016E-14,0.));
#13596=DIRECTION('',(-1.22464679914735E-16,-7.02543712147503E-30,1.));
#13597=DIRECTION('center_axis',(0.,0.,1.));
#13598=DIRECTION('ref_axis',(-1.,-5.72445829159016E-14,0.));
#13599=DIRECTION('',(-1.22464679914735E-16,-7.02543712147503E-30,1.));
#13600=DIRECTION('center_axis',(0.,0.,1.));
#13601=DIRECTION('ref_axis',(0.609351642559645,-0.79290010449606,0.));
#13602=DIRECTION('',(-1.22464679914735E-16,-7.02543712147503E-30,1.));
#13603=DIRECTION('center_axis',(0.,0.,1.));
#13604=DIRECTION('ref_axis',(-1.,-5.72445829159016E-14,0.));
#13605=DIRECTION('center_axis',(0.,0.,-1.));
#13606=DIRECTION('ref_axis',(1.,0.,0.));
#13607=DIRECTION('',(0.,0.,-1.));
#13608=DIRECTION('center_axis',(0.,0.,1.));
#13609=DIRECTION('ref_axis',(1.,0.,0.));
#13610=DIRECTION('',(0.,0.,-1.));
#13611=DIRECTION('center_axis',(0.,0.,1.));
#13612=DIRECTION('ref_axis',(1.,0.,0.));
#13613=DIRECTION('center_axis',(0.,0.,1.));
#13614=DIRECTION('ref_axis',(1.,0.,0.));
#13615=DIRECTION('center_axis',(0.,0.,-1.));
#13616=DIRECTION('ref_axis',(1.,0.,0.));
#13617=DIRECTION('',(0.,0.,-1.));
#13618=DIRECTION('center_axis',(0.,0.,-1.));
#13619=DIRECTION('ref_axis',(1.,0.,0.));
#13620=DIRECTION('',(0.,0.,-1.));
#13621=DIRECTION('center_axis',(0.,0.,-1.));
#13622=DIRECTION('ref_axis',(1.,0.,0.));
#13623=DIRECTION('',(0.,0.,-1.));
#13624=DIRECTION('center_axis',(0.,0.,-1.));
#13625=DIRECTION('ref_axis',(1.,0.,0.));
#13626=DIRECTION('',(0.,0.,-1.));
#13627=DIRECTION('center_axis',(0.,0.,-1.));
#13628=DIRECTION('ref_axis',(1.,0.,0.));
#13629=DIRECTION('',(0.,0.,-1.));
#13630=DIRECTION('center_axis',(0.,0.,-1.));
#13631=DIRECTION('ref_axis',(1.,0.,0.));
#13632=DIRECTION('',(0.,0.,-1.));
#13633=DIRECTION('center_axis',(0.,0.,-1.));
#13634=DIRECTION('ref_axis',(1.,0.,0.));
#13635=DIRECTION('',(0.,0.,-1.));
#13636=DIRECTION('center_axis',(0.,0.,-1.));
#13637=DIRECTION('ref_axis',(1.,0.,0.));
#13638=DIRECTION('',(0.,0.,-1.));
#13639=DIRECTION('center_axis',(0.,0.,-1.));
#13640=DIRECTION('ref_axis',(1.,0.,0.));
#13641=DIRECTION('',(0.,0.,-1.));
#13642=DIRECTION('center_axis',(0.,0.,-1.));
#13643=DIRECTION('ref_axis',(1.,0.,0.));
#13644=DIRECTION('',(0.,0.,-1.));
#13645=DIRECTION('center_axis',(0.,0.,-1.));
#13646=DIRECTION('ref_axis',(1.,0.,0.));
#13647=DIRECTION('',(0.,0.,-1.));
#13648=DIRECTION('center_axis',(0.,0.,-1.));
#13649=DIRECTION('ref_axis',(1.,0.,0.));
#13650=DIRECTION('',(0.,0.,-1.));
#13651=DIRECTION('center_axis',(0.,0.,-1.));
#13652=DIRECTION('ref_axis',(1.,0.,0.));
#13653=DIRECTION('',(0.,0.,-1.));
#13654=DIRECTION('center_axis',(0.,0.,-1.));
#13655=DIRECTION('ref_axis',(1.,0.,0.));
#13656=DIRECTION('',(0.,0.,-1.));
#13657=DIRECTION('center_axis',(0.,0.,-1.));
#13658=DIRECTION('ref_axis',(1.,0.,0.));
#13659=DIRECTION('',(0.,0.,-1.));
#13660=DIRECTION('center_axis',(0.,0.,-1.));
#13661=DIRECTION('ref_axis',(1.,0.,0.));
#13662=DIRECTION('',(0.,0.,-1.));
#13663=DIRECTION('center_axis',(0.,0.,-1.));
#13664=DIRECTION('ref_axis',(0.937376106323228,-0.348318870138132,0.));
#13665=DIRECTION('',(0.,0.,-1.));
#13666=DIRECTION('center_axis',(0.,0.,-1.));
#13667=DIRECTION('ref_axis',(1.,0.,0.));
#13668=DIRECTION('center_axis',(0.,0.,-1.));
#13669=DIRECTION('ref_axis',(1.,-9.27379496885572E-14,0.));
#13670=DIRECTION('',(1.22464679914735E-16,-1.13721209223846E-29,-1.));
#13671=DIRECTION('center_axis',(0.,0.,1.));
#13672=DIRECTION('ref_axis',(1.,-9.27379496885572E-14,0.));
#13673=DIRECTION('center_axis',(0.,0.,-1.));
#13674=DIRECTION('ref_axis',(1.,-9.27379496885572E-14,0.));
#13675=DIRECTION('',(1.22464679914735E-16,-1.13721209223846E-29,-1.));
#13676=DIRECTION('center_axis',(0.,0.,-1.));
#13677=DIRECTION('ref_axis',(1.,-9.27379496885572E-14,0.));
#13678=DIRECTION('',(1.22464679914735E-16,-1.13721209223846E-29,-1.));
#13679=DIRECTION('center_axis',(0.,0.,-1.));
#13680=DIRECTION('ref_axis',(1.,-9.27379496885572E-14,0.));
#13681=DIRECTION('',(1.22464679914735E-16,-1.13721209223846E-29,-1.));
#13682=DIRECTION('center_axis',(0.,0.,-1.));
#13683=DIRECTION('ref_axis',(1.,-9.27379496885572E-14,0.));
#13684=DIRECTION('',(1.22464679914735E-16,-1.13721209223846E-29,-1.));
#13685=DIRECTION('center_axis',(0.,0.,-1.));
#13686=DIRECTION('ref_axis',(1.,-9.27379496885572E-14,0.));
#13687=DIRECTION('',(1.22464679914735E-16,-1.13721209223846E-29,-1.));
#13688=DIRECTION('center_axis',(0.,0.,-1.));
#13689=DIRECTION('ref_axis',(1.,-9.27379496885572E-14,0.));
#13690=DIRECTION('',(1.22464679914735E-16,-1.13721209223846E-29,-1.));
#13691=DIRECTION('center_axis',(0.,0.,-1.));
#13692=DIRECTION('ref_axis',(1.,-9.27379496885572E-14,0.));
#13693=DIRECTION('',(1.22464679914735E-16,-1.13721209223846E-29,-1.));
#13694=DIRECTION('center_axis',(0.,0.,-1.));
#13695=DIRECTION('ref_axis',(1.,-9.27379496885572E-14,0.));
#13696=DIRECTION('',(1.22464679914735E-16,-1.13721209223846E-29,-1.));
#13697=DIRECTION('center_axis',(0.,0.,-1.));
#13698=DIRECTION('ref_axis',(1.,-9.27379496885572E-14,0.));
#13699=DIRECTION('',(1.22464679914735E-16,-1.13721209223846E-29,-1.));
#13700=DIRECTION('center_axis',(0.,0.,-1.));
#13701=DIRECTION('ref_axis',(1.,-9.27379496885572E-14,0.));
#13702=DIRECTION('',(1.22464679914735E-16,-1.13721209223846E-29,-1.));
#13703=DIRECTION('center_axis',(0.,0.,-1.));
#13704=DIRECTION('ref_axis',(1.,-9.27379496885572E-14,0.));
#13705=DIRECTION('',(1.22464679914735E-16,-1.13721209223846E-29,-1.));
#13706=DIRECTION('center_axis',(0.,0.,-1.));
#13707=DIRECTION('ref_axis',(1.,-9.27379496885572E-14,0.));
#13708=DIRECTION('',(1.22464679914735E-16,-1.13721209223846E-29,-1.));
#13709=DIRECTION('center_axis',(0.,0.,-1.));
#13710=DIRECTION('ref_axis',(1.,-9.27379496885572E-14,0.));
#13711=DIRECTION('',(1.22464679914735E-16,-1.13721209223846E-29,-1.));
#13712=DIRECTION('center_axis',(0.,0.,-1.));
#13713=DIRECTION('ref_axis',(1.,-9.27379496885572E-14,0.));
#13714=DIRECTION('',(1.22464679914735E-16,-1.13721209223846E-29,-1.));
#13715=DIRECTION('center_axis',(0.,0.,-1.));
#13716=DIRECTION('ref_axis',(1.,-9.27379496885572E-14,0.));
#13717=DIRECTION('',(1.22464679914735E-16,-1.13721209223846E-29,-1.));
#13718=DIRECTION('center_axis',(0.,0.,-1.));
#13719=DIRECTION('ref_axis',(1.,-9.27379496885572E-14,0.));
#13720=DIRECTION('',(1.22464679914735E-16,-1.13721209223846E-29,-1.));
#13721=DIRECTION('center_axis',(0.,0.,-1.));
#13722=DIRECTION('ref_axis',(-0.609161390867883,-0.793046278520936,0.));
#13723=DIRECTION('',(1.22464679914735E-16,-1.13721209223846E-29,-1.));
#13724=DIRECTION('center_axis',(0.,0.,-1.));
#13725=DIRECTION('ref_axis',(1.,-9.27379496885572E-14,0.));
#13726=DIRECTION('center_axis',(0.,0.,1.));
#13727=DIRECTION('ref_axis',(1.,0.,0.));
#13728=DIRECTION('center_axis',(0.,0.,-1.));
#13729=DIRECTION('ref_axis',(1.,-9.27379496885572E-14,0.));
#13730=DIRECTION('center_axis',(0.,0.,-1.));
#13731=DIRECTION('ref_axis',(1.,0.,0.));
#13732=DIRECTION('center_axis',(0.,0.,-1.));
#13733=DIRECTION('ref_axis',(1.,0.,0.));
#13734=DIRECTION('center_axis',(0.,0.,1.));
#13735=DIRECTION('ref_axis',(1.,0.,0.));
#13736=DIRECTION('center_axis',(0.,0.,1.));
#13737=DIRECTION('ref_axis',(-1.,-5.72445829159016E-14,0.));
#13738=DIRECTION('center_axis',(0.,0.,1.));
#13739=DIRECTION('ref_axis',(-1.,0.,0.));
#13740=DIRECTION('center_axis',(0.,0.,1.));
#13741=DIRECTION('ref_axis',(-1.,0.,0.));
#13742=DIRECTION('center_axis',(0.,1.,0.));
#13743=DIRECTION('ref_axis',(-1.,0.,0.));
#13744=DIRECTION('',(-1.,0.,0.));
#13745=DIRECTION('',(0.,0.,1.));
#13746=DIRECTION('',(-1.,0.,0.));
#13747=DIRECTION('',(0.,0.,1.));
#13748=DIRECTION('center_axis',(1.,0.,0.));
#13749=DIRECTION('ref_axis',(0.,1.,0.));
#13750=DIRECTION('',(0.,1.,0.));
#13751=DIRECTION('',(0.,1.,0.));
#13752=DIRECTION('',(0.,0.,1.));
#13753=DIRECTION('center_axis',(0.,-1.,0.));
#13754=DIRECTION('ref_axis',(1.,0.,0.));
#13755=DIRECTION('',(1.,0.,0.));
#13756=DIRECTION('',(1.,0.,0.));
#13757=DIRECTION('',(0.,0.,1.));
#13758=DIRECTION('center_axis',(-1.,0.,0.));
#13759=DIRECTION('ref_axis',(0.,-1.,0.));
#13760=DIRECTION('',(0.,-1.,0.));
#13761=DIRECTION('',(0.,-1.,0.));
#13762=DIRECTION('center_axis',(0.,0.,1.));
#13763=DIRECTION('ref_axis',(1.,0.,0.));
#13764=DIRECTION('center_axis',(0.,0.,1.));
#13765=DIRECTION('ref_axis',(1.,0.,0.));
#13766=DIRECTION('axis',(0.,0.,1.));
#13767=DIRECTION('refdir',(1.,0.,0.));
#13768=DIRECTION('center_axis',(0.,0.,-1.));
#13769=DIRECTION('ref_axis',(1.,0.,0.));
#13770=DIRECTION('',(0.,0.,-1.));
#13771=DIRECTION('center_axis',(0.,0.,1.));
#13772=DIRECTION('ref_axis',(1.,0.,0.));
#13773=DIRECTION('',(0.,0.,-1.));
#13774=DIRECTION('center_axis',(0.,0.,1.));
#13775=DIRECTION('ref_axis',(1.,0.,0.));
#13776=DIRECTION('center_axis',(0.,0.,1.));
#13777=DIRECTION('ref_axis',(1.,0.,0.));
#13778=DIRECTION('center_axis',(0.,0.,-1.));
#13779=DIRECTION('ref_axis',(1.,0.,0.));
#13780=DIRECTION('',(0.,0.,-1.));
#13781=DIRECTION('center_axis',(0.,0.,-1.));
#13782=DIRECTION('ref_axis',(1.,0.,0.));
#13783=DIRECTION('',(0.,0.,-1.));
#13784=DIRECTION('center_axis',(0.,0.,-1.));
#13785=DIRECTION('ref_axis',(1.,0.,0.));
#13786=DIRECTION('',(0.,0.,-1.));
#13787=DIRECTION('center_axis',(0.,0.,-1.));
#13788=DIRECTION('ref_axis',(1.,0.,0.));
#13789=DIRECTION('',(0.,0.,-1.));
#13790=DIRECTION('center_axis',(0.,0.,-1.));
#13791=DIRECTION('ref_axis',(1.,0.,0.));
#13792=DIRECTION('',(0.,0.,-1.));
#13793=DIRECTION('center_axis',(0.,0.,-1.));
#13794=DIRECTION('ref_axis',(1.,0.,0.));
#13795=DIRECTION('',(0.,0.,-1.));
#13796=DIRECTION('center_axis',(0.,0.,-1.));
#13797=DIRECTION('ref_axis',(1.,0.,0.));
#13798=DIRECTION('',(0.,0.,-1.));
#13799=DIRECTION('center_axis',(0.,0.,-1.));
#13800=DIRECTION('ref_axis',(1.,0.,0.));
#13801=DIRECTION('',(0.,0.,-1.));
#13802=DIRECTION('center_axis',(0.,0.,-1.));
#13803=DIRECTION('ref_axis',(0.937367309351136,-0.348342543137946,0.));
#13804=DIRECTION('',(0.,0.,-1.));
#13805=DIRECTION('center_axis',(0.,0.,-1.));
#13806=DIRECTION('ref_axis',(1.,0.,0.));
#13807=DIRECTION('center_axis',(0.,0.,-1.));
#13808=DIRECTION('ref_axis',(1.,-4.8329028703551E-14,0.));
#13809=DIRECTION('',(1.22464679914735E-16,-5.93359662859705E-30,-1.));
#13810=DIRECTION('center_axis',(0.,0.,1.));
#13811=DIRECTION('ref_axis',(1.,-4.8329028703551E-14,0.));
#13812=DIRECTION('center_axis',(0.,0.,-1.));
#13813=DIRECTION('ref_axis',(1.,-4.8329028703551E-14,0.));
#13814=DIRECTION('',(1.22464679914735E-16,-5.93359662859705E-30,-1.));
#13815=DIRECTION('center_axis',(0.,0.,-1.));
#13816=DIRECTION('ref_axis',(1.,-4.8329028703551E-14,0.));
#13817=DIRECTION('',(1.22464679914735E-16,-5.93359662859705E-30,-1.));
#13818=DIRECTION('center_axis',(0.,0.,-1.));
#13819=DIRECTION('ref_axis',(1.,-4.8329028703551E-14,0.));
#13820=DIRECTION('',(1.22464679914735E-16,-5.93359662859705E-30,-1.));
#13821=DIRECTION('center_axis',(0.,0.,-1.));
#13822=DIRECTION('ref_axis',(1.,-4.8329028703551E-14,0.));
#13823=DIRECTION('',(1.22464679914735E-16,-5.93359662859705E-30,-1.));
#13824=DIRECTION('center_axis',(0.,0.,-1.));
#13825=DIRECTION('ref_axis',(1.,-4.8329028703551E-14,0.));
#13826=DIRECTION('',(1.22464679914735E-16,-5.93359662859705E-30,-1.));
#13827=DIRECTION('center_axis',(0.,0.,-1.));
#13828=DIRECTION('ref_axis',(1.,-4.8329028703551E-14,0.));
#13829=DIRECTION('',(1.22464679914735E-16,-5.93359662859705E-30,-1.));
#13830=DIRECTION('center_axis',(0.,0.,-1.));
#13831=DIRECTION('ref_axis',(1.,-4.8329028703551E-14,0.));
#13832=DIRECTION('',(1.22464679914735E-16,-5.93359662859705E-30,-1.));
#13833=DIRECTION('center_axis',(0.,0.,-1.));
#13834=DIRECTION('ref_axis',(1.,-4.8329028703551E-14,0.));
#13835=DIRECTION('',(1.22464679914735E-16,-5.93359662859705E-30,-1.));
#13836=DIRECTION('center_axis',(0.,0.,-1.));
#13837=DIRECTION('ref_axis',(-0.609222020738255,-0.792999703308644,0.));
#13838=DIRECTION('',(1.22464679914735E-16,-5.93359662859705E-30,-1.));
#13839=DIRECTION('center_axis',(0.,0.,-1.));
#13840=DIRECTION('ref_axis',(1.,-4.8329028703551E-14,0.));
#13841=DIRECTION('center_axis',(0.,0.,1.));
#13842=DIRECTION('ref_axis',(1.,0.,0.));
#13843=DIRECTION('center_axis',(0.,0.,-1.));
#13844=DIRECTION('ref_axis',(1.,-4.8329028703551E-14,0.));
#13845=DIRECTION('center_axis',(0.,0.,-1.));
#13846=DIRECTION('ref_axis',(1.,0.,0.));
#13847=DIRECTION('center_axis',(0.,0.,-1.));
#13848=DIRECTION('ref_axis',(1.,0.,0.));
#13849=DIRECTION('center_axis',(0.,0.,-1.));
#13850=DIRECTION('ref_axis',(1.,0.,0.));
#13851=DIRECTION('center_axis',(0.,0.,-1.));
#13852=DIRECTION('ref_axis',(1.,0.,0.));
#13853=DIRECTION('',(0.,0.,-1.));
#13854=DIRECTION('center_axis',(0.,0.,1.));
#13855=DIRECTION('ref_axis',(1.,0.,0.));
#13856=DIRECTION('center_axis',(1.,0.,0.));
#13857=DIRECTION('ref_axis',(0.,1.,0.));
#13858=DIRECTION('',(0.,1.,0.));
#13859=DIRECTION('',(0.,0.,1.));
#13860=DIRECTION('',(0.,1.,0.));
#13861=DIRECTION('',(0.,0.,1.));
#13862=DIRECTION('center_axis',(0.,0.,1.));
#13863=DIRECTION('ref_axis',(1.,0.,0.));
#13864=DIRECTION('',(0.,-1.,0.));
#13865=DIRECTION('',(-1.,0.,0.));
#13866=DIRECTION('',(1.,0.,0.));
#13867=DIRECTION('center_axis',(0.,1.,0.));
#13868=DIRECTION('ref_axis',(-1.,0.,0.));
#13869=DIRECTION('',(-1.,0.,0.));
#13870=DIRECTION('',(0.,0.,1.));
#13871=DIRECTION('',(-1.,0.,0.));
#13872=DIRECTION('',(0.,0.,1.));
#13873=DIRECTION('center_axis',(1.,0.,0.));
#13874=DIRECTION('ref_axis',(0.,1.,0.));
#13875=DIRECTION('',(0.,0.,1.));
#13876=DIRECTION('',(0.,1.,0.));
#13877=DIRECTION('center_axis',(0.,-1.,0.));
#13878=DIRECTION('ref_axis',(1.,0.,0.));
#13879=DIRECTION('',(1.,0.,0.));
#13880=DIRECTION('',(0.,0.,1.));
#13881=DIRECTION('',(1.,0.,0.));
#13882=DIRECTION('center_axis',(-1.,0.,0.));
#13883=DIRECTION('ref_axis',(0.,-1.,0.));
#13884=DIRECTION('',(0.,-1.,0.));
#13885=DIRECTION('',(0.,-1.,0.));
#13886=DIRECTION('center_axis',(0.,0.,1.));
#13887=DIRECTION('ref_axis',(1.,0.,0.));
#13888=DIRECTION('center_axis',(0.,0.,1.));
#13889=DIRECTION('ref_axis',(1.,0.,0.));
#13890=DIRECTION('axis',(0.,0.,1.));
#13891=DIRECTION('refdir',(1.,0.,0.));
#13892=DIRECTION('center_axis',(0.,0.,-1.));
#13893=DIRECTION('ref_axis',(1.,0.,0.));
#13894=DIRECTION('center_axis',(0.,0.,-1.));
#13895=DIRECTION('ref_axis',(1.,0.,0.));
#13896=DIRECTION('',(0.,0.,-1.));
#13897=DIRECTION('center_axis',(0.,0.,1.));
#13898=DIRECTION('ref_axis',(1.,0.,0.));
#13899=DIRECTION('center_axis',(0.,1.,0.));
#13900=DIRECTION('ref_axis',(-1.,0.,0.));
#13901=DIRECTION('',(-1.,0.,0.));
#13902=DIRECTION('',(0.,0.,1.));
#13903=DIRECTION('',(-1.,0.,0.));
#13904=DIRECTION('',(0.,0.,1.));
#13905=DIRECTION('center_axis',(1.,0.,0.));
#13906=DIRECTION('ref_axis',(0.,1.,0.));
#13907=DIRECTION('',(0.,1.,0.));
#13908=DIRECTION('',(0.,1.,0.));
#13909=DIRECTION('',(0.,0.,1.));
#13910=DIRECTION('center_axis',(0.,-1.,0.));
#13911=DIRECTION('ref_axis',(1.,0.,0.));
#13912=DIRECTION('',(1.,0.,0.));
#13913=DIRECTION('',(1.,0.,0.));
#13914=DIRECTION('',(0.,0.,1.));
#13915=DIRECTION('center_axis',(-1.,0.,0.));
#13916=DIRECTION('ref_axis',(0.,-1.,0.));
#13917=DIRECTION('',(0.,-1.,0.));
#13918=DIRECTION('',(0.,-1.,0.));
#13919=DIRECTION('center_axis',(0.,0.,1.));
#13920=DIRECTION('ref_axis',(1.,0.,0.));
#13921=DIRECTION('center_axis',(0.,0.,1.));
#13922=DIRECTION('ref_axis',(1.,0.,0.));
#13923=DIRECTION('axis',(0.,0.,1.));
#13924=DIRECTION('refdir',(1.,0.,0.));
#13925=DIRECTION('center_axis',(6.12323399573677E-17,0.,1.));
#13926=DIRECTION('ref_axis',(1.,0.,0.));
#13927=DIRECTION('center_axis',(1.22464679914735E-16,-1.,0.));
#13928=DIRECTION('ref_axis',(-1.,-1.22464679914735E-16,0.));
#13929=DIRECTION('axis',(0.,0.,1.));
#13930=DIRECTION('refdir',(1.,0.,0.));
#13931=DIRECTION('center_axis',(0.,0.,1.));
#13932=DIRECTION('ref_axis',(1.,0.,0.));
#13933=DIRECTION('center_axis',(0.,0.,1.));
#13934=DIRECTION('ref_axis',(1.,0.,0.));
#13935=DIRECTION('center_axis',(0.,0.,1.));
#13936=DIRECTION('ref_axis',(1.,0.,0.));
#13937=DIRECTION('center_axis',(0.,0.,1.));
#13938=DIRECTION('ref_axis',(1.,0.,0.));
#13939=DIRECTION('center_axis',(0.,0.,1.));
#13940=DIRECTION('ref_axis',(1.,0.,0.));
#13941=DIRECTION('',(0.,0.,-1.));
#13942=DIRECTION('center_axis',(0.,0.,1.));
#13943=DIRECTION('ref_axis',(1.,0.,0.));
#13944=DIRECTION('center_axis',(0.,0.,1.));
#13945=DIRECTION('ref_axis',(1.,0.,0.));
#13946=DIRECTION('',(0.,0.,-1.));
#13947=DIRECTION('center_axis',(0.,0.,1.));
#13948=DIRECTION('ref_axis',(1.,0.,0.));
#13949=DIRECTION('center_axis',(0.,0.,1.));
#13950=DIRECTION('ref_axis',(1.,0.,0.));
#13951=DIRECTION('axis',(0.,0.,1.));
#13952=DIRECTION('refdir',(1.,0.,0.));
#13953=DIRECTION('center_axis',(0.,0.,-1.));
#13954=DIRECTION('ref_axis',(-1.,0.,0.));
#13955=DIRECTION('center_axis',(7.34788079488412E-16,0.,-1.));
#13956=DIRECTION('ref_axis',(-1.,0.,-7.34788079488412E-16));
#13957=DIRECTION('center_axis',(-7.34788079488412E-16,0.,1.));
#13958=DIRECTION('ref_axis',(1.,0.,7.34788079488412E-16));
#13959=DIRECTION('center_axis',(0.,0.,1.));
#13960=DIRECTION('ref_axis',(1.,0.,0.));
#13961=DIRECTION('axis',(0.,0.,1.));
#13962=DIRECTION('refdir',(1.,0.,0.));
#13963=DIRECTION('center_axis',(0.,0.,1.));
#13964=DIRECTION('ref_axis',(1.,0.,0.));
#13965=DIRECTION('',(0.,0.,-1.));
#13966=DIRECTION('center_axis',(0.,0.,-1.));
#13967=DIRECTION('ref_axis',(1.,0.,0.));
#13968=DIRECTION('center_axis',(0.,0.,1.));
#13969=DIRECTION('ref_axis',(1.,0.,0.));
#13970=DIRECTION('',(0.,0.,-1.));
#13971=DIRECTION('center_axis',(0.,0.,1.));
#13972=DIRECTION('ref_axis',(1.,0.,0.));
#13973=DIRECTION('',(0.,0.,-1.));
#13974=DIRECTION('center_axis',(0.,0.,1.));
#13975=DIRECTION('ref_axis',(1.,0.,0.));
#13976=DIRECTION('',(0.,0.,-1.));
#13977=DIRECTION('center_axis',(0.,0.,1.));
#13978=DIRECTION('ref_axis',(1.,0.,0.));
#13979=DIRECTION('',(0.,0.,-1.));
#13980=DIRECTION('center_axis',(0.,0.,1.));
#13981=DIRECTION('ref_axis',(1.,0.,0.));
#13982=DIRECTION('',(0.,0.,-1.));
#13983=DIRECTION('center_axis',(0.,0.,1.));
#13984=DIRECTION('ref_axis',(1.,0.,0.));
#13985=DIRECTION('',(0.,0.,-1.));
#13986=DIRECTION('center_axis',(0.,0.,1.));
#13987=DIRECTION('ref_axis',(1.,0.,0.));
#13988=DIRECTION('',(0.,0.,-1.));
#13989=DIRECTION('center_axis',(0.,0.,1.));
#13990=DIRECTION('ref_axis',(1.,0.,0.));
#13991=DIRECTION('',(0.,0.,-1.));
#13992=DIRECTION('center_axis',(0.,0.,1.));
#13993=DIRECTION('ref_axis',(1.,0.,0.));
#13994=DIRECTION('',(0.,0.,-1.));
#13995=DIRECTION('center_axis',(0.,0.,1.));
#13996=DIRECTION('ref_axis',(1.,0.,0.));
#13997=DIRECTION('',(0.,0.,-1.));
#13998=DIRECTION('center_axis',(0.,0.,1.));
#13999=DIRECTION('ref_axis',(1.,0.,0.));
#14000=DIRECTION('',(0.,0.,-1.));
#14001=DIRECTION('center_axis',(0.,0.,1.));
#14002=DIRECTION('ref_axis',(1.,0.,0.));
#14003=DIRECTION('',(0.,0.,-1.));
#14004=DIRECTION('center_axis',(0.,0.,1.));
#14005=DIRECTION('ref_axis',(1.,0.,0.));
#14006=DIRECTION('',(0.,0.,-1.));
#14007=DIRECTION('center_axis',(0.,0.,1.));
#14008=DIRECTION('ref_axis',(1.,0.,0.));
#14009=DIRECTION('',(0.,0.,-1.));
#14010=DIRECTION('center_axis',(0.,0.,1.));
#14011=DIRECTION('ref_axis',(1.,0.,0.));
#14012=DIRECTION('',(0.,0.,-1.));
#14013=DIRECTION('center_axis',(0.,0.,1.));
#14014=DIRECTION('ref_axis',(1.,1.29731060939901E-13,0.));
#14015=DIRECTION('',(0.,0.,1.));
#14016=DIRECTION('center_axis',(0.,0.,-1.));
#14017=DIRECTION('ref_axis',(1.,1.29731060939901E-13,0.));
#14018=DIRECTION('center_axis',(0.,0.,1.));
#14019=DIRECTION('ref_axis',(1.,1.29731060939901E-13,0.));
#14020=DIRECTION('',(0.,0.,1.));
#14021=DIRECTION('center_axis',(0.,0.,1.));
#14022=DIRECTION('ref_axis',(1.,1.29731060939901E-13,0.));
#14023=DIRECTION('',(0.,0.,1.));
#14024=DIRECTION('center_axis',(0.,0.,1.));
#14025=DIRECTION('ref_axis',(1.,1.29731060939901E-13,0.));
#14026=DIRECTION('',(0.,0.,1.));
#14027=DIRECTION('center_axis',(0.,0.,1.));
#14028=DIRECTION('ref_axis',(1.,1.29731060939901E-13,0.));
#14029=DIRECTION('',(0.,0.,1.));
#14030=DIRECTION('center_axis',(0.,0.,1.));
#14031=DIRECTION('ref_axis',(1.,1.29731060939901E-13,0.));
#14032=DIRECTION('',(0.,0.,1.));
#14033=DIRECTION('center_axis',(0.,0.,1.));
#14034=DIRECTION('ref_axis',(1.,1.29731060939901E-13,0.));
#14035=DIRECTION('',(0.,0.,1.));
#14036=DIRECTION('center_axis',(0.,0.,1.));
#14037=DIRECTION('ref_axis',(1.,1.29731060939901E-13,0.));
#14038=DIRECTION('',(0.,0.,1.));
#14039=DIRECTION('center_axis',(0.,0.,1.));
#14040=DIRECTION('ref_axis',(1.,1.29731060939901E-13,0.));
#14041=DIRECTION('',(0.,0.,1.));
#14042=DIRECTION('center_axis',(0.,0.,1.));
#14043=DIRECTION('ref_axis',(1.,1.29731060939901E-13,0.));
#14044=DIRECTION('',(0.,0.,1.));
#14045=DIRECTION('center_axis',(0.,0.,1.));
#14046=DIRECTION('ref_axis',(1.,1.29731060939901E-13,0.));
#14047=DIRECTION('',(0.,0.,1.));
#14048=DIRECTION('center_axis',(0.,0.,1.));
#14049=DIRECTION('ref_axis',(1.,1.29731060939901E-13,0.));
#14050=DIRECTION('',(0.,0.,1.));
#14051=DIRECTION('center_axis',(0.,0.,1.));
#14052=DIRECTION('ref_axis',(1.,1.29731060939901E-13,0.));
#14053=DIRECTION('',(0.,0.,1.));
#14054=DIRECTION('center_axis',(0.,0.,1.));
#14055=DIRECTION('ref_axis',(1.,1.29731060939901E-13,0.));
#14056=DIRECTION('',(0.,0.,1.));
#14057=DIRECTION('center_axis',(0.,0.,1.));
#14058=DIRECTION('ref_axis',(1.,1.29731060939901E-13,0.));
#14059=DIRECTION('',(0.,0.,1.));
#14060=DIRECTION('center_axis',(0.,0.,1.));
#14061=DIRECTION('ref_axis',(1.,1.29731060939901E-13,0.));
#14062=DIRECTION('',(0.,0.,1.));
#14063=DIRECTION('center_axis',(0.,0.,-1.));
#14064=DIRECTION('ref_axis',(1.,0.,0.));
#14065=DIRECTION('center_axis',(0.,0.,-1.));
#14066=DIRECTION('ref_axis',(1.,0.,0.));
#14067=DIRECTION('',(0.707106781186548,8.65956056235494E-17,0.707106781186547));
#14068=DIRECTION('center_axis',(0.,0.,1.));
#14069=DIRECTION('ref_axis',(1.,0.,0.));
#14070=DIRECTION('center_axis',(0.,0.,1.));
#14071=DIRECTION('ref_axis',(1.,1.29731060939901E-13,0.));
#14072=DIRECTION('center_axis',(0.,0.,-1.));
#14073=DIRECTION('ref_axis',(1.,1.29731060939901E-13,0.));
#14074=DIRECTION('center_axis',(0.,0.,1.));
#14075=DIRECTION('ref_axis',(1.,0.,0.));
#14076=DIRECTION('center_axis',(-1.60246890531964E-16,-1.,0.));
#14077=DIRECTION('ref_axis',(1.,-1.60246890531964E-16,0.));
#14078=DIRECTION('',(1.,-1.60246890531964E-16,0.));
#14079=DIRECTION('',(0.,0.,1.));
#14080=DIRECTION('',(1.,-1.60246890531964E-16,0.));
#14081=DIRECTION('',(0.,0.,1.));
#14082=DIRECTION('center_axis',(-0.866025403784439,-0.5,0.));
#14083=DIRECTION('ref_axis',(0.5,-0.866025403784439,0.));
#14084=DIRECTION('',(0.5,-0.866025403784439,0.));
#14085=DIRECTION('',(0.,0.,1.));
#14086=DIRECTION('',(0.5,-0.866025403784439,0.));
#14087=DIRECTION('center_axis',(-0.866025403784439,0.5,0.));
#14088=DIRECTION('ref_axis',(-0.5,-0.866025403784439,0.));
#14089=DIRECTION('',(-0.5,-0.866025403784439,0.));
#14090=DIRECTION('',(0.,0.,1.));
#14091=DIRECTION('',(-0.5,-0.866025403784439,0.));
#14092=DIRECTION('center_axis',(1.60246890531964E-16,1.,0.));
#14093=DIRECTION('ref_axis',(-1.,1.60246890531964E-16,0.));
#14094=DIRECTION('',(-1.,1.60246890531964E-16,0.));
#14095=DIRECTION('',(0.,0.,1.));
#14096=DIRECTION('',(-1.,1.60246890531964E-16,0.));
#14097=DIRECTION('center_axis',(0.866025403784439,0.5,0.));
#14098=DIRECTION('ref_axis',(-0.5,0.866025403784439,0.));
#14099=DIRECTION('',(-0.5,0.866025403784439,0.));
#14100=DIRECTION('',(0.,0.,1.));
#14101=DIRECTION('',(-0.5,0.866025403784439,0.));
#14102=DIRECTION('center_axis',(0.866025403784439,-0.5,0.));
#14103=DIRECTION('ref_axis',(0.5,0.866025403784439,0.));
#14104=DIRECTION('',(0.5,0.866025403784439,0.));
#14105=DIRECTION('',(0.5,0.866025403784439,0.));
#14106=DIRECTION('center_axis',(0.,0.,1.));
#14107=DIRECTION('ref_axis',(1.,0.,0.));
#14108=DIRECTION('center_axis',(0.,0.,1.));
#14109=DIRECTION('ref_axis',(1.,0.,0.));
#14110=DIRECTION('center_axis',(0.,0.,1.));
#14111=DIRECTION('ref_axis',(1.,0.,0.));
#14112=DIRECTION('center_axis',(0.,0.,1.));
#14113=DIRECTION('ref_axis',(1.,0.,0.));
#14114=DIRECTION('',(0.,0.,-1.));
#14115=DIRECTION('center_axis',(0.,0.,1.));
#14116=DIRECTION('ref_axis',(1.,0.,0.));
#14117=DIRECTION('center_axis',(0.,0.,1.));
#14118=DIRECTION('ref_axis',(1.,0.,0.));
#14119=DIRECTION('center_axis',(0.,0.,1.));
#14120=DIRECTION('ref_axis',(1.,0.,0.));
#14121=DIRECTION('axis',(0.,0.,1.));
#14122=DIRECTION('refdir',(1.,0.,0.));
#14123=DIRECTION('center_axis',(0.,0.,1.));
#14124=DIRECTION('ref_axis',(1.,0.,0.));
#14125=DIRECTION('',(0.,0.,-1.));
#14126=DIRECTION('center_axis',(0.,0.,-1.));
#14127=DIRECTION('ref_axis',(1.,0.,0.));
#14128=DIRECTION('center_axis',(0.,0.,1.));
#14129=DIRECTION('ref_axis',(1.,0.,0.));
#14130=DIRECTION('',(0.,0.,-1.));
#14131=DIRECTION('center_axis',(0.,0.,1.));
#14132=DIRECTION('ref_axis',(1.,0.,0.));
#14133=DIRECTION('',(0.,0.,-1.));
#14134=DIRECTION('center_axis',(0.,0.,1.));
#14135=DIRECTION('ref_axis',(1.,0.,0.));
#14136=DIRECTION('',(0.,0.,-1.));
#14137=DIRECTION('center_axis',(0.,0.,1.));
#14138=DIRECTION('ref_axis',(1.,0.,0.));
#14139=DIRECTION('',(0.,0.,-1.));
#14140=DIRECTION('center_axis',(0.,0.,1.));
#14141=DIRECTION('ref_axis',(1.,0.,0.));
#14142=DIRECTION('',(0.,0.,-1.));
#14143=DIRECTION('center_axis',(0.,0.,1.));
#14144=DIRECTION('ref_axis',(1.,0.,0.));
#14145=DIRECTION('',(0.,0.,-1.));
#14146=DIRECTION('center_axis',(0.,0.,1.));
#14147=DIRECTION('ref_axis',(1.,0.,0.));
#14148=DIRECTION('',(0.,0.,-1.));
#14149=DIRECTION('center_axis',(0.,0.,1.));
#14150=DIRECTION('ref_axis',(1.,0.,0.));
#14151=DIRECTION('',(0.,0.,-1.));
#14152=DIRECTION('center_axis',(0.,0.,1.));
#14153=DIRECTION('ref_axis',(1.,0.,0.));
#14154=DIRECTION('',(0.,0.,-1.));
#14155=DIRECTION('center_axis',(0.,0.,1.));
#14156=DIRECTION('ref_axis',(1.,7.53540174823413E-14,0.));
#14157=DIRECTION('',(0.,0.,1.));
#14158=DIRECTION('center_axis',(0.,0.,-1.));
#14159=DIRECTION('ref_axis',(1.,7.53540174823413E-14,0.));
#14160=DIRECTION('center_axis',(0.,0.,1.));
#14161=DIRECTION('ref_axis',(1.,7.53540174823413E-14,0.));
#14162=DIRECTION('',(0.,0.,1.));
#14163=DIRECTION('center_axis',(0.,0.,1.));
#14164=DIRECTION('ref_axis',(1.,7.53540174823413E-14,0.));
#14165=DIRECTION('',(0.,0.,1.));
#14166=DIRECTION('center_axis',(0.,0.,1.));
#14167=DIRECTION('ref_axis',(1.,7.53540174823413E-14,0.));
#14168=DIRECTION('',(0.,0.,1.));
#14169=DIRECTION('center_axis',(0.,0.,1.));
#14170=DIRECTION('ref_axis',(1.,7.53540174823413E-14,0.));
#14171=DIRECTION('',(0.,0.,1.));
#14172=DIRECTION('center_axis',(0.,0.,1.));
#14173=DIRECTION('ref_axis',(1.,7.53540174823413E-14,0.));
#14174=DIRECTION('',(0.,0.,1.));
#14175=DIRECTION('center_axis',(0.,0.,1.));
#14176=DIRECTION('ref_axis',(1.,7.53540174823413E-14,0.));
#14177=DIRECTION('',(0.,0.,1.));
#14178=DIRECTION('center_axis',(0.,0.,1.));
#14179=DIRECTION('ref_axis',(1.,7.53540174823413E-14,0.));
#14180=DIRECTION('',(0.,0.,1.));
#14181=DIRECTION('center_axis',(0.,0.,1.));
#14182=DIRECTION('ref_axis',(1.,7.53540174823413E-14,0.));
#14183=DIRECTION('',(0.,0.,1.));
#14184=DIRECTION('center_axis',(0.,0.,1.));
#14185=DIRECTION('ref_axis',(1.,7.53540174823413E-14,0.));
#14186=DIRECTION('',(0.,0.,1.));
#14187=DIRECTION('center_axis',(0.,0.,-1.));
#14188=DIRECTION('ref_axis',(1.,0.,0.));
#14189=DIRECTION('center_axis',(0.,0.,-1.));
#14190=DIRECTION('ref_axis',(1.,0.,0.));
#14191=DIRECTION('',(0.707106781186548,8.65956056235493E-17,0.707106781186547));
#14192=DIRECTION('center_axis',(0.,0.,1.));
#14193=DIRECTION('ref_axis',(1.,0.,0.));
#14194=DIRECTION('center_axis',(0.,0.,1.));
#14195=DIRECTION('ref_axis',(1.,7.53540174823413E-14,0.));
#14196=DIRECTION('center_axis',(0.,0.,-1.));
#14197=DIRECTION('ref_axis',(1.,7.53540174823413E-14,0.));
#14198=DIRECTION('center_axis',(0.,0.,1.));
#14199=DIRECTION('ref_axis',(1.,0.,0.));
#14200=DIRECTION('center_axis',(-2.40370335797945E-16,-1.,0.));
#14201=DIRECTION('ref_axis',(1.,-2.40370335797945E-16,0.));
#14202=DIRECTION('',(1.,-2.40370335797945E-16,0.));
#14203=DIRECTION('',(0.,0.,1.));
#14204=DIRECTION('',(1.,-2.40370335797945E-16,0.));
#14205=DIRECTION('',(0.,0.,1.));
#14206=DIRECTION('center_axis',(-0.866025403784439,-0.5,0.));
#14207=DIRECTION('ref_axis',(0.5,-0.866025403784439,0.));
#14208=DIRECTION('',(0.5,-0.866025403784439,0.));
#14209=DIRECTION('',(0.,0.,1.));
#14210=DIRECTION('',(0.5,-0.866025403784439,0.));
#14211=DIRECTION('center_axis',(-0.866025403784439,0.5,0.));
#14212=DIRECTION('ref_axis',(-0.5,-0.866025403784439,0.));
#14213=DIRECTION('',(-0.5,-0.866025403784439,0.));
#14214=DIRECTION('',(0.,0.,1.));
#14215=DIRECTION('',(-0.5,-0.866025403784439,0.));
#14216=DIRECTION('center_axis',(1.20185167898973E-16,1.,0.));
#14217=DIRECTION('ref_axis',(-1.,1.20185167898973E-16,0.));
#14218=DIRECTION('',(-1.,1.20185167898973E-16,0.));
#14219=DIRECTION('',(0.,0.,1.));
#14220=DIRECTION('',(-1.,1.20185167898973E-16,0.));
#14221=DIRECTION('center_axis',(0.866025403784439,0.5,0.));
#14222=DIRECTION('ref_axis',(-0.5,0.866025403784439,0.));
#14223=DIRECTION('',(-0.5,0.866025403784439,0.));
#14224=DIRECTION('',(0.,0.,1.));
#14225=DIRECTION('',(-0.5,0.866025403784439,0.));
#14226=DIRECTION('center_axis',(0.866025403784439,-0.5,0.));
#14227=DIRECTION('ref_axis',(0.5,0.866025403784439,0.));
#14228=DIRECTION('',(0.5,0.866025403784439,0.));
#14229=DIRECTION('',(0.5,0.866025403784439,0.));
#14230=DIRECTION('center_axis',(0.,0.,1.));
#14231=DIRECTION('ref_axis',(1.,0.,0.));
#14232=DIRECTION('center_axis',(0.,0.,1.));
#14233=DIRECTION('ref_axis',(1.,0.,0.));
#14234=DIRECTION('center_axis',(0.,0.,1.));
#14235=DIRECTION('ref_axis',(1.,0.,0.));
#14236=DIRECTION('center_axis',(0.,0.,1.));
#14237=DIRECTION('ref_axis',(1.,0.,0.));
#14238=DIRECTION('',(0.,0.,-1.));
#14239=DIRECTION('center_axis',(0.,0.,1.));
#14240=DIRECTION('ref_axis',(1.,0.,0.));
#14241=DIRECTION('center_axis',(0.,0.,1.));
#14242=DIRECTION('ref_axis',(1.,0.,0.));
#14243=DIRECTION('center_axis',(0.,0.,1.));
#14244=DIRECTION('ref_axis',(1.,0.,0.));
#14245=DIRECTION('axis',(0.,0.,1.));
#14246=DIRECTION('refdir',(1.,0.,0.));
#14247=DIRECTION('center_axis',(0.,0.,1.));
#14248=DIRECTION('ref_axis',(1.,0.,0.));
#14249=DIRECTION('',(0.,0.,-1.));
#14250=DIRECTION('center_axis',(0.,0.,-1.));
#14251=DIRECTION('ref_axis',(1.,0.,0.));
#14252=DIRECTION('center_axis',(0.,0.,1.));
#14253=DIRECTION('ref_axis',(1.,0.,0.));
#14254=DIRECTION('',(0.,0.,-1.));
#14255=DIRECTION('center_axis',(0.,0.,1.));
#14256=DIRECTION('ref_axis',(1.,0.,0.));
#14257=DIRECTION('',(0.,0.,-1.));
#14258=DIRECTION('center_axis',(0.,0.,1.));
#14259=DIRECTION('ref_axis',(1.,0.,0.));
#14260=DIRECTION('',(0.,0.,-1.));
#14261=DIRECTION('center_axis',(0.,0.,1.));
#14262=DIRECTION('ref_axis',(1.,0.,0.));
#14263=DIRECTION('',(0.,0.,-1.));
#14264=DIRECTION('center_axis',(0.,0.,1.));
#14265=DIRECTION('ref_axis',(1.,0.,0.));
#14266=DIRECTION('',(0.,0.,-1.));
#14267=DIRECTION('center_axis',(0.,0.,1.));
#14268=DIRECTION('ref_axis',(1.,0.,0.));
#14269=DIRECTION('',(0.,0.,-1.));
#14270=DIRECTION('center_axis',(0.,0.,1.));
#14271=DIRECTION('ref_axis',(1.,0.,0.));
#14272=DIRECTION('',(0.,0.,-1.));
#14273=DIRECTION('center_axis',(0.,0.,1.));
#14274=DIRECTION('ref_axis',(1.,0.,0.));
#14275=DIRECTION('',(0.,0.,-1.));
#14276=DIRECTION('center_axis',(0.,0.,1.));
#14277=DIRECTION('ref_axis',(1.,0.,0.));
#14278=DIRECTION('',(0.,0.,-1.));
#14279=DIRECTION('center_axis',(0.,0.,1.));
#14280=DIRECTION('ref_axis',(1.,0.,0.));
#14281=DIRECTION('',(0.,0.,-1.));
#14282=DIRECTION('center_axis',(0.,0.,1.));
#14283=DIRECTION('ref_axis',(1.,0.,0.));
#14284=DIRECTION('',(0.,0.,-1.));
#14285=DIRECTION('center_axis',(0.,0.,1.));
#14286=DIRECTION('ref_axis',(1.,0.,0.));
#14287=DIRECTION('',(0.,0.,-1.));
#14288=DIRECTION('center_axis',(0.,0.,1.));
#14289=DIRECTION('ref_axis',(1.,0.,0.));
#14290=DIRECTION('',(0.,0.,-1.));
#14291=DIRECTION('center_axis',(0.,0.,1.));
#14292=DIRECTION('ref_axis',(1.,0.,0.));
#14293=DIRECTION('',(0.,0.,-1.));
#14294=DIRECTION('center_axis',(0.,0.,1.));
#14295=DIRECTION('ref_axis',(1.,0.,0.));
#14296=DIRECTION('',(0.,0.,-1.));
#14297=DIRECTION('center_axis',(0.,0.,1.));
#14298=DIRECTION('ref_axis',(1.,0.,0.));
#14299=DIRECTION('',(0.,0.,-1.));
#14300=DIRECTION('center_axis',(0.,0.,1.));
#14301=DIRECTION('ref_axis',(1.,0.,0.));
#14302=DIRECTION('',(0.,0.,-1.));
#14303=DIRECTION('center_axis',(0.,0.,1.));
#14304=DIRECTION('ref_axis',(1.,1.10671505702589E-13,0.));
#14305=DIRECTION('',(0.,0.,1.));
#14306=DIRECTION('center_axis',(0.,0.,-1.));
#14307=DIRECTION('ref_axis',(1.,1.10671505702589E-13,0.));
#14308=DIRECTION('center_axis',(0.,0.,1.));
#14309=DIRECTION('ref_axis',(1.,1.10671505702589E-13,0.));
#14310=DIRECTION('',(0.,0.,1.));
#14311=DIRECTION('center_axis',(0.,0.,1.));
#14312=DIRECTION('ref_axis',(1.,1.10671505702589E-13,0.));
#14313=DIRECTION('',(0.,0.,1.));
#14314=DIRECTION('center_axis',(0.,0.,1.));
#14315=DIRECTION('ref_axis',(1.,1.10671505702589E-13,0.));
#14316=DIRECTION('',(0.,0.,1.));
#14317=DIRECTION('center_axis',(0.,0.,1.));
#14318=DIRECTION('ref_axis',(1.,1.10671505702589E-13,0.));
#14319=DIRECTION('',(0.,0.,1.));
#14320=DIRECTION('center_axis',(0.,0.,1.));
#14321=DIRECTION('ref_axis',(1.,1.10671505702589E-13,0.));
#14322=DIRECTION('',(0.,0.,1.));
#14323=DIRECTION('center_axis',(0.,0.,1.));
#14324=DIRECTION('ref_axis',(1.,1.10671505702589E-13,0.));
#14325=DIRECTION('',(0.,0.,1.));
#14326=DIRECTION('center_axis',(0.,0.,1.));
#14327=DIRECTION('ref_axis',(1.,1.10671505702589E-13,0.));
#14328=DIRECTION('',(0.,0.,1.));
#14329=DIRECTION('center_axis',(0.,0.,1.));
#14330=DIRECTION('ref_axis',(1.,1.10671505702589E-13,0.));
#14331=DIRECTION('',(0.,0.,1.));
#14332=DIRECTION('center_axis',(0.,0.,1.));
#14333=DIRECTION('ref_axis',(1.,1.10671505702589E-13,0.));
#14334=DIRECTION('',(0.,0.,1.));
#14335=DIRECTION('center_axis',(0.,0.,1.));
#14336=DIRECTION('ref_axis',(1.,1.10671505702589E-13,0.));
#14337=DIRECTION('',(0.,0.,1.));
#14338=DIRECTION('center_axis',(0.,0.,1.));
#14339=DIRECTION('ref_axis',(1.,1.10671505702589E-13,0.));
#14340=DIRECTION('',(0.,0.,1.));
#14341=DIRECTION('center_axis',(0.,0.,1.));
#14342=DIRECTION('ref_axis',(1.,1.10671505702589E-13,0.));
#14343=DIRECTION('',(0.,0.,1.));
#14344=DIRECTION('center_axis',(0.,0.,1.));
#14345=DIRECTION('ref_axis',(1.,1.10671505702589E-13,0.));
#14346=DIRECTION('',(0.,0.,1.));
#14347=DIRECTION('center_axis',(0.,0.,1.));
#14348=DIRECTION('ref_axis',(1.,1.10671505702589E-13,0.));
#14349=DIRECTION('',(0.,0.,1.));
#14350=DIRECTION('center_axis',(0.,0.,1.));
#14351=DIRECTION('ref_axis',(1.,1.10671505702589E-13,0.));
#14352=DIRECTION('',(0.,0.,1.));
#14353=DIRECTION('center_axis',(0.,0.,1.));
#14354=DIRECTION('ref_axis',(1.,1.10671505702589E-13,0.));
#14355=DIRECTION('',(0.,0.,1.));
#14356=DIRECTION('center_axis',(0.,0.,1.));
#14357=DIRECTION('ref_axis',(1.,1.10671505702589E-13,0.));
#14358=DIRECTION('',(0.,0.,1.));
#14359=DIRECTION('center_axis',(0.,0.,-1.));
#14360=DIRECTION('ref_axis',(1.,0.,0.));
#14361=DIRECTION('center_axis',(0.,0.,-1.));
#14362=DIRECTION('ref_axis',(1.,0.,0.));
#14363=DIRECTION('',(0.707106781186548,8.65956056235493E-17,0.707106781186547));
#14364=DIRECTION('center_axis',(0.,0.,1.));
#14365=DIRECTION('ref_axis',(1.,0.,0.));
#14366=DIRECTION('center_axis',(0.,0.,1.));
#14367=DIRECTION('ref_axis',(1.,1.10671505702589E-13,0.));
#14368=DIRECTION('center_axis',(0.,0.,-1.));
#14369=DIRECTION('ref_axis',(1.,1.10671505702589E-13,0.));
#14370=DIRECTION('center_axis',(0.,0.,1.));
#14371=DIRECTION('ref_axis',(1.,0.,0.));
#14372=DIRECTION('center_axis',(-2.40370335797945E-16,-1.,0.));
#14373=DIRECTION('ref_axis',(1.,-2.40370335797945E-16,0.));
#14374=DIRECTION('',(1.,-2.40370335797945E-16,0.));
#14375=DIRECTION('',(0.,0.,1.));
#14376=DIRECTION('',(1.,-2.40370335797945E-16,0.));
#14377=DIRECTION('',(0.,0.,1.));
#14378=DIRECTION('center_axis',(-0.866025403784439,-0.5,0.));
#14379=DIRECTION('ref_axis',(0.5,-0.866025403784439,0.));
#14380=DIRECTION('',(0.5,-0.866025403784439,0.));
#14381=DIRECTION('',(0.,0.,1.));
#14382=DIRECTION('',(0.5,-0.866025403784439,0.));
#14383=DIRECTION('center_axis',(-0.866025403784439,0.5,0.));
#14384=DIRECTION('ref_axis',(-0.5,-0.866025403784439,0.));
#14385=DIRECTION('',(-0.5,-0.866025403784439,0.));
#14386=DIRECTION('',(0.,0.,1.));
#14387=DIRECTION('',(-0.5,-0.866025403784439,0.));
#14388=DIRECTION('center_axis',(1.20185167898973E-16,1.,0.));
#14389=DIRECTION('ref_axis',(-1.,1.20185167898973E-16,0.));
#14390=DIRECTION('',(-1.,1.20185167898973E-16,0.));
#14391=DIRECTION('',(0.,0.,1.));
#14392=DIRECTION('',(-1.,1.20185167898973E-16,0.));
#14393=DIRECTION('center_axis',(0.866025403784439,0.5,0.));
#14394=DIRECTION('ref_axis',(-0.5,0.866025403784439,0.));
#14395=DIRECTION('',(-0.5,0.866025403784439,0.));
#14396=DIRECTION('',(0.,0.,1.));
#14397=DIRECTION('',(-0.5,0.866025403784439,0.));
#14398=DIRECTION('center_axis',(0.866025403784439,-0.5,0.));
#14399=DIRECTION('ref_axis',(0.5,0.866025403784439,0.));
#14400=DIRECTION('',(0.5,0.866025403784439,0.));
#14401=DIRECTION('',(0.5,0.866025403784439,0.));
#14402=DIRECTION('center_axis',(0.,0.,1.));
#14403=DIRECTION('ref_axis',(1.,0.,0.));
#14404=DIRECTION('center_axis',(0.,0.,1.));
#14405=DIRECTION('ref_axis',(1.,0.,0.));
#14406=DIRECTION('center_axis',(0.,0.,1.));
#14407=DIRECTION('ref_axis',(1.,0.,0.));
#14408=DIRECTION('center_axis',(0.,0.,1.));
#14409=DIRECTION('ref_axis',(1.,0.,0.));
#14410=DIRECTION('',(0.,0.,-1.));
#14411=DIRECTION('center_axis',(0.,0.,1.));
#14412=DIRECTION('ref_axis',(1.,0.,0.));
#14413=DIRECTION('center_axis',(0.,0.,1.));
#14414=DIRECTION('ref_axis',(1.,0.,0.));
#14415=DIRECTION('center_axis',(0.,0.,1.));
#14416=DIRECTION('ref_axis',(1.,0.,0.));
#14417=DIRECTION('axis',(0.,0.,1.));
#14418=DIRECTION('refdir',(1.,0.,0.));
#14419=DIRECTION('center_axis',(0.,0.,1.));
#14420=DIRECTION('ref_axis',(1.,0.,0.));
#14421=DIRECTION('',(0.,0.,-1.));
#14422=DIRECTION('center_axis',(0.,0.,-1.));
#14423=DIRECTION('ref_axis',(1.,0.,0.));
#14424=DIRECTION('center_axis',(0.,0.,1.));
#14425=DIRECTION('ref_axis',(1.,0.,0.));
#14426=DIRECTION('',(0.,0.,-1.));
#14427=DIRECTION('center_axis',(0.,0.,1.));
#14428=DIRECTION('ref_axis',(0.995010084519338,-0.0997744040564514,0.));
#14429=DIRECTION('',(0.,0.,1.));
#14430=DIRECTION('center_axis',(0.,0.,-1.));
#14431=DIRECTION('ref_axis',(1.,2.96346172991068E-16,0.));
#14432=DIRECTION('center_axis',(0.,0.,1.));
#14433=DIRECTION('ref_axis',(1.,2.96346172991068E-16,0.));
#14434=DIRECTION('',(0.,0.,1.));
#14435=DIRECTION('center_axis',(0.,0.,-1.));
#14436=DIRECTION('ref_axis',(1.,0.,0.));
#14437=DIRECTION('center_axis',(0.,0.,-1.));
#14438=DIRECTION('ref_axis',(1.,0.,0.));
#14439=DIRECTION('',(0.707106781186547,8.65956056235493E-17,0.707106781186548));
#14440=DIRECTION('center_axis',(0.,0.,1.));
#14441=DIRECTION('ref_axis',(1.,0.,0.));
#14442=DIRECTION('center_axis',(0.,0.,1.));
#14443=DIRECTION('ref_axis',(0.889042129798311,0.457825394057258,0.));
#14444=DIRECTION('center_axis',(0.,0.,-1.));
#14445=DIRECTION('ref_axis',(1.,2.96346172991068E-16,0.));
#14446=DIRECTION('center_axis',(0.,0.,1.));
#14447=DIRECTION('ref_axis',(1.,0.,0.));
#14448=DIRECTION('center_axis',(-1.92296268638356E-16,-1.,0.));
#14449=DIRECTION('ref_axis',(1.,-1.92296268638356E-16,0.));
#14450=DIRECTION('',(1.,-1.92296268638356E-16,0.));
#14451=DIRECTION('',(0.,0.,1.));
#14452=DIRECTION('',(1.,-1.92296268638356E-16,0.));
#14453=DIRECTION('',(0.,0.,1.));
#14454=DIRECTION('center_axis',(-0.866025403784439,-0.5,0.));
#14455=DIRECTION('ref_axis',(0.5,-0.866025403784439,0.));
#14456=DIRECTION('',(0.5,-0.866025403784439,0.));
#14457=DIRECTION('',(0.,0.,1.));
#14458=DIRECTION('',(0.5,-0.866025403784439,0.));
#14459=DIRECTION('center_axis',(-0.866025403784439,0.5,0.));
#14460=DIRECTION('ref_axis',(-0.5,-0.866025403784439,0.));
#14461=DIRECTION('',(-0.5,-0.866025403784439,0.));
#14462=DIRECTION('',(0.,0.,1.));
#14463=DIRECTION('',(-0.5,-0.866025403784438,0.));
#14464=DIRECTION('center_axis',(1.92296268638356E-16,1.,0.));
#14465=DIRECTION('ref_axis',(-1.,1.92296268638356E-16,0.));
#14466=DIRECTION('',(-1.,1.92296268638356E-16,0.));
#14467=DIRECTION('',(0.,0.,1.));
#14468=DIRECTION('',(-1.,1.92296268638356E-16,0.));
#14469=DIRECTION('center_axis',(0.866025403784439,0.5,0.));
#14470=DIRECTION('ref_axis',(-0.5,0.866025403784439,0.));
#14471=DIRECTION('',(-0.5,0.866025403784439,0.));
#14472=DIRECTION('',(0.,0.,1.));
#14473=DIRECTION('',(-0.5,0.866025403784439,0.));
#14474=DIRECTION('center_axis',(0.866025403784439,-0.5,0.));
#14475=DIRECTION('ref_axis',(0.5,0.866025403784439,0.));
#14476=DIRECTION('',(0.5,0.866025403784439,0.));
#14477=DIRECTION('',(0.5,0.866025403784439,0.));
#14478=DIRECTION('center_axis',(0.,0.,1.));
#14479=DIRECTION('ref_axis',(1.,0.,0.));
#14480=DIRECTION('center_axis',(0.,0.,1.));
#14481=DIRECTION('ref_axis',(1.,0.,0.));
#14482=DIRECTION('center_axis',(0.,0.,1.));
#14483=DIRECTION('ref_axis',(1.,0.,0.));
#14484=DIRECTION('center_axis',(0.,0.,1.));
#14485=DIRECTION('ref_axis',(1.,0.,0.));
#14486=DIRECTION('',(0.,0.,-1.));
#14487=DIRECTION('center_axis',(0.,0.,1.));
#14488=DIRECTION('ref_axis',(1.,0.,0.));
#14489=DIRECTION('center_axis',(0.,0.,1.));
#14490=DIRECTION('ref_axis',(1.,0.,0.));
#14491=DIRECTION('center_axis',(0.,0.,1.));
#14492=DIRECTION('ref_axis',(1.,0.,0.));
#14493=DIRECTION('',(0.,0.,1.));
#14494=DIRECTION('',(1.,0.,0.));
#14495=DIRECTION('',(0.,0.,1.));
#14496=DIRECTION('',(1.,0.,0.));
#14497=DIRECTION('',(0.,1.,0.));
#14498=DIRECTION('',(1.,0.,0.));
#14499=DIRECTION('',(6.12323399573677E-17,-6.12323399573677E-17,1.));
#14500=DIRECTION('',(1.,6.12323399573677E-17,-6.12323399573676E-17));
#14501=DIRECTION('',(6.12323399573677E-17,-6.12323399573677E-17,1.));
#14502=DIRECTION('',(1.,6.12323399573677E-17,-6.12323399573676E-17));
#14503=DIRECTION('',(6.12323399573677E-17,-6.12323399573677E-17,1.));
#14504=DIRECTION('',(1.,6.12323399573677E-17,-6.12323399573676E-17));
#14505=DIRECTION('',(0.,0.,1.));
#14506=DIRECTION('',(1.,0.,0.));
#14507=DIRECTION('',(0.,0.,1.));
#14508=DIRECTION('',(1.,0.,0.));
#14509=DIRECTION('',(0.,0.,1.));
#14510=DIRECTION('',(1.,0.,0.));
#14511=DIRECTION('',(0.,0.,1.));
#14512=DIRECTION('',(1.,0.,0.));
#14513=DIRECTION('',(1.,0.,0.));
#14514=DIRECTION('',(0.,1.,0.));
#14515=DIRECTION('',(0.,-1.,0.));
#14516=DIRECTION('',(1.,0.,0.));
#14517=DIRECTION('',(0.,0.,1.));
#14518=DIRECTION('',(1.,0.,0.));
#14519=DIRECTION('',(0.,0.,1.));
#14520=DIRECTION('',(-1.,1.22464679914735E-16,0.));
#14521=DIRECTION('',(0.,0.,1.));
#14522=DIRECTION('',(1.,0.,0.));
#14523=DIRECTION('',(0.,0.,1.));
#14524=DIRECTION('',(1.,0.,0.));
#14525=DIRECTION('',(-1.,0.,0.));
#14526=DIRECTION('',(0.,-1.,0.));
#14527=DIRECTION('',(0.,0.,1.));
#14528=DIRECTION('',(0.,1.,0.));
#14529=DIRECTION('',(0.,-1.22464679914735E-16,-1.));
#14530=DIRECTION('',(-0.766044443118978,-0.64278760968654,7.87187788734199E-17));
#14531=DIRECTION('',(-6.12323399573676E-17,-6.12323399573677E-17,-1.));
#14532=DIRECTION('',(1.,6.12323399573677E-17,-6.12323399573676E-17));
#14533=DIRECTION('',(0.,-1.22464679914735E-16,-1.));
#14534=DIRECTION('',(1.,0.,0.));
#14535=DIRECTION('',(-1.,0.,0.));
#14536=DIRECTION('',(0.,1.,0.));
#14537=DIRECTION('',(0.,0.,1.));
#14538=DIRECTION('',(0.,-1.,0.));
#14539=DIRECTION('',(0.,-1.22464679914735E-16,-1.));
#14540=DIRECTION('',(-0.766044443118978,-0.64278760968654,7.87187788734199E-17));
#14541=DIRECTION('',(0.,-1.22464679914735E-16,-1.));
#14542=DIRECTION('',(-0.766044443118978,-0.64278760968654,7.87187788734199E-17));
#14543=DIRECTION('',(0.,-1.22464679914735E-16,-1.));
#14544=DIRECTION('',(-0.766044443118978,-0.64278760968654,7.87187788734199E-17));
#14545=DIRECTION('',(0.,-2.46519032881566E-32,1.));
#14546=DIRECTION('',(-2.77555756156289E-16,-1.,0.));
#14547=DIRECTION('',(0.,-2.46519032881566E-32,1.));
#14548=DIRECTION('',(-2.77555756156289E-16,-1.,0.));
#14549=DIRECTION('',(-6.12323399573676E-17,-6.12323399573677E-17,-1.));
#14550=DIRECTION('',(2.27765793651141E-16,-1.,6.12323399573676E-17));
#14551=DIRECTION('',(-6.12323399573676E-17,-6.12323399573677E-17,-1.));
#14552=DIRECTION('',(1.,6.12323399573677E-17,-6.12323399573676E-17));
#14553=DIRECTION('',(1.49975978266186E-32,1.22464679914735E-16,-1.));
#14554=DIRECTION('',(-1.,1.22464679914735E-16,0.));
#14555=DIRECTION('',(0.,-1.22464679914735E-16,-1.));
#14556=DIRECTION('',(1.,0.,0.));
#14557=DIRECTION('',(0.,-1.22464679914735E-16,-1.));
#14558=DIRECTION('',(1.,0.,0.));
#14559=DIRECTION('',(1.,0.,0.));
#14560=DIRECTION('',(0.,-1.,0.));
#14561=CARTESIAN_POINT('',(0.,0.,0.));
#14562=CARTESIAN_POINT('',(0.,0.,0.));
#14563=CARTESIAN_POINT('Origin',(-3.6,-2.4,4.7));
#14564=CARTESIAN_POINT('',(-3.76675587540948,-2.40012144305632,4.38714803633902));
#14565=CARTESIAN_POINT('',(-3.76680083731002,-2.3999030629831,4.36785196366098));
#14566=CARTESIAN_POINT('',(-3.7666,-2.4,4.7));
#14567=CARTESIAN_POINT('',(-3.76351293272515,-2.4319230454628,4.3));
#14568=CARTESIAN_POINT('Ctrl Pts',(-3.76680083731002,-2.3999030629831,4.36785196366098));
#14569=CARTESIAN_POINT('Ctrl Pts',(-3.76684159509423,-2.39409443145766,
4.36746222055426));
#14570=CARTESIAN_POINT('Ctrl Pts',(-3.76656457427738,-2.38828969174785,
4.36707247744754));
#14571=CARTESIAN_POINT('Ctrl Pts',(-3.76595694000634,-2.38251974073322,
4.36668273434082));
#14572=CARTESIAN_POINT('Ctrl Pts',(-3.76018123887082,-2.32767505172373,
4.36297813798855));
#14573=CARTESIAN_POINT('Ctrl Pts',(-3.72453483587179,-2.27597349778246,
4.35927354163629));
#14574=CARTESIAN_POINT('Ctrl Pts',(-3.675321975809,-2.25108560394313,4.35556894528402));
#14575=CARTESIAN_POINT('Ctrl Pts',(-3.6261091157462,-2.22619771010379,4.35186434893175));
#14576=CARTESIAN_POINT('Ctrl Pts',(-3.56332979861965,-2.22812347636638,
4.34815975257948));
#14577=CARTESIAN_POINT('Ctrl Pts',(-3.51573443717815,-2.25596350777206,
4.34445515622722));
#14578=CARTESIAN_POINT('Ctrl Pts',(-3.46813907573665,-2.28380353917775,
4.34075055987495));
#14579=CARTESIAN_POINT('Ctrl Pts',(-3.43572766998022,-2.33755783572652,
4.33704596352268));
#14580=CARTESIAN_POINT('Ctrl Pts',(-3.43329506857802,-2.39266164758784,
4.33334136717041));
#14581=CARTESIAN_POINT('Ctrl Pts',(-3.43086246717583,-2.44776545944916,
4.32963677081814));
#14582=CARTESIAN_POINT('Ctrl Pts',(-3.45840867012789,-2.50421878662303,
4.32593217446588));
#14583=CARTESIAN_POINT('Ctrl Pts',(-3.5034058713341,-2.53611223252088,4.32222757811361));
#14584=CARTESIAN_POINT('Ctrl Pts',(-3.5484030725403,-2.56800567841873,4.31852298176134));
#14585=CARTESIAN_POINT('Ctrl Pts',(-3.61085127200066,-2.57533924304056,
4.31481838540907));
#14586=CARTESIAN_POINT('Ctrl Pts',(-3.66197494402253,-2.55491156986817,
4.3111137890568));
#14587=CARTESIAN_POINT('Ctrl Pts',(-3.7130986160444,-2.53448389669578,4.30740919270454));
#14588=CARTESIAN_POINT('Ctrl Pts',(-3.75289776062778,-2.48629498572916,
4.30370459635227));
#14589=CARTESIAN_POINT('Ctrl Pts',(-3.76351293272515,-2.4319230454628,4.3));
#14590=CARTESIAN_POINT('',(-3.60525667617797,-2.23318013248672,4.3));
#14591=CARTESIAN_POINT('Origin',(-3.6,-2.4,4.3));
#14592=CARTESIAN_POINT('',(-3.766345497777,-2.40006497186855,4.31714803633902));
#14593=CARTESIAN_POINT('Ctrl Pts',(-3.60525667255608,-2.23317994016621,
4.3));
#14594=CARTESIAN_POINT('Ctrl Pts',(-3.65930633468078,-2.23495318766097,
4.30363229181855));
#14595=CARTESIAN_POINT('Ctrl Pts',(-3.71251718041942,-2.26542183293127,
4.30726458363711));
#14596=CARTESIAN_POINT('Ctrl Pts',(-3.74128612006692,-2.31121589839408,
4.31089687545566));
#14597=CARTESIAN_POINT('Ctrl Pts',(-3.75778986656855,-2.33748637123519,
4.31298059575011));
#14598=CARTESIAN_POINT('Ctrl Pts',(-3.76624997632687,-2.36880031787527,
4.31506431604457));
#14599=CARTESIAN_POINT('Ctrl Pts',(-3.766345497777,-2.40006497186855,4.31714803633902));
#14600=CARTESIAN_POINT('',(-3.7666,-2.4,4.2));
#14601=CARTESIAN_POINT('',(-3.7666,-2.4,4.7));
#14602=CARTESIAN_POINT('Origin',(-3.6,-2.4,4.2));
#14603=CARTESIAN_POINT('Ctrl Pts',(-3.766345497777,-2.40006497186855,4.31714803633902));
#14604=CARTESIAN_POINT('Ctrl Pts',(-3.76641980162283,-2.42438499660917,
4.31876891239684));
#14605=CARTESIAN_POINT('Ctrl Pts',(-3.76143276745508,-2.44867519480749,
4.32038978845465));
#14606=CARTESIAN_POINT('Ctrl Pts',(-3.75123332790854,-2.47053847327949,
4.32201066451247));
#14607=CARTESIAN_POINT('Ctrl Pts',(-3.72792197948242,-2.52050813091336,
4.32571526086474));
#14608=CARTESIAN_POINT('Ctrl Pts',(-3.67738234157418,-2.55780017273342,
4.329419857217));
#14609=CARTESIAN_POINT('Ctrl Pts',(-3.6227496090289,-2.56532196535192,4.33312445356927));
#14610=CARTESIAN_POINT('Ctrl Pts',(-3.56811687648362,-2.57284375797042,
4.33682904992154));
#14611=CARTESIAN_POINT('Ctrl Pts',(-3.5093910493013,-2.55059530138736,4.34053364627381));
#14612=CARTESIAN_POINT('Ctrl Pts',(-3.47344562081921,-2.50877156715293,
4.34423824262608));
#14613=CARTESIAN_POINT('Ctrl Pts',(-3.43750019233712,-2.4669478329185,4.34794283897835));
#14614=CARTESIAN_POINT('Ctrl Pts',(-3.42433516255526,-2.40554882103269,
4.35164743533061));
#14615=CARTESIAN_POINT('Ctrl Pts',(-3.4399769373371,-2.35266772584057,4.35535203168288));
#14616=CARTESIAN_POINT('Ctrl Pts',(-3.45561871211893,-2.29978663064845,
4.35905662803515));
#14617=CARTESIAN_POINT('Ctrl Pts',(-3.50006729146445,-2.25542345215002,
4.36276122438742));
#14618=CARTESIAN_POINT('Ctrl Pts',(-3.55297985415763,-2.23988445249497,
4.36646582073969));
#14619=CARTESIAN_POINT('Ctrl Pts',(-3.60589241685081,-2.22434545283993,
4.37017041709195));
#14620=CARTESIAN_POINT('Ctrl Pts',(-3.66726896289165,-2.23763063202826,
4.37387501344422));
#14621=CARTESIAN_POINT('Ctrl Pts',(-3.70902050597011,-2.2736583534049,4.37757960979649));
#14622=CARTESIAN_POINT('Ctrl Pts',(-3.74496653400264,-2.3046764520682,4.38076908531067));
#14623=CARTESIAN_POINT('Ctrl Pts',(-3.76636579491573,-2.35255215149476,
4.38395856082485));
#14624=CARTESIAN_POINT('Ctrl Pts',(-3.76675587540948,-2.40012144305632,
4.38714803633902));
#14625=CARTESIAN_POINT('Origin',(-3.6,-2.4,4.7));
#14626=CARTESIAN_POINT('',(-3.76672469163696,-2.39986752250016,4.45714803633902));
#14627=CARTESIAN_POINT('',(-3.76637108132843,-2.3999167674636,4.43785196366098));
#14628=CARTESIAN_POINT('',(-3.7666,-2.4,4.7));
#14629=CARTESIAN_POINT('Ctrl Pts',(-3.76637108132843,-2.3999167674636,4.43785196366098));
#14630=CARTESIAN_POINT('Ctrl Pts',(-3.76647256500337,-2.37748041616576,
4.43635646533454));
#14631=CARTESIAN_POINT('Ctrl Pts',(-3.7622516281058,-2.3550806593951,4.43486096700809));
#14632=CARTESIAN_POINT('Ctrl Pts',(-3.7535269013147,-2.3345994559913,4.43336546868165));
#14633=CARTESIAN_POINT('Ctrl Pts',(-3.73191431207048,-2.28386413246858,
4.42966087232938));
#14634=CARTESIAN_POINT('Ctrl Pts',(-3.68266490417161,-2.24490171859149,
4.42595627597712));
#14635=CARTESIAN_POINT('Ctrl Pts',(-3.62831780053848,-2.23554372384707,
4.42225167962485));
#14636=CARTESIAN_POINT('Ctrl Pts',(-3.57397069690535,-2.22618572910265,
4.41854708327258));
#14637=CARTESIAN_POINT('Ctrl Pts',(-3.51452589753796,-2.2464321534909,4.41484248692031));
#14638=CARTESIAN_POINT('Ctrl Pts',(-3.47718894803579,-2.28701682605767,
4.41113789056804));
#14639=CARTESIAN_POINT('Ctrl Pts',(-3.43985199853362,-2.32760149862444,
4.40743329421577));
#14640=CARTESIAN_POINT('Ctrl Pts',(-3.42462289889666,-2.38852441936972,
4.40372869786351));
#14641=CARTESIAN_POINT('Ctrl Pts',(-3.4384707400222,-2.441904428893,4.40002410151124));
#14642=CARTESIAN_POINT('Ctrl Pts',(-3.45231858114774,-2.49528443841629,
4.39631950515897));
#14643=CARTESIAN_POINT('Ctrl Pts',(-3.49524336303579,-2.54112153671759,
4.3926149088067));
#14644=CARTESIAN_POINT('Ctrl Pts',(-3.54760150310682,-2.55843699301478,
4.38891031245443));
#14645=CARTESIAN_POINT('Ctrl Pts',(-3.59995964317784,-2.57575244931197,
4.38520571610217));
#14646=CARTESIAN_POINT('Ctrl Pts',(-3.66175114143183,-2.56454626360505,
4.3815011197499));
#14647=CARTESIAN_POINT('Ctrl Pts',(-3.70469439092283,-2.52994925871274,
4.37779652339763));
#14648=CARTESIAN_POINT('Ctrl Pts',(-3.74311978370889,-2.49899204150246,
4.37448167015208));
#14649=CARTESIAN_POINT('Ctrl Pts',(-3.76645418313973,-2.44930678746824,
4.37116681690653));
#14650=CARTESIAN_POINT('Ctrl Pts',(-3.76680083731002,-2.3999030629831,4.36785196366098));
#14651=CARTESIAN_POINT('Ctrl Pts',(-3.76675587540948,-2.40012144305632,
4.38714803633902));
#14652=CARTESIAN_POINT('Ctrl Pts',(-3.76681887592163,-2.40780419002449,
4.38766315717712));
#14653=CARTESIAN_POINT('Ctrl Pts',(-3.76633386603033,-2.41547894454867,
4.38817827801521));
#14654=CARTESIAN_POINT('Ctrl Pts',(-3.76527362096253,-2.42307339831024,
4.3886933988533));
#14655=CARTESIAN_POINT('Ctrl Pts',(-3.75764865276043,-2.47769045827401,
4.39239799520556));
#14656=CARTESIAN_POINT('Ctrl Pts',(-3.72027217624014,-2.52815431463659,
4.39610259155783));
#14657=CARTESIAN_POINT('Ctrl Pts',(-3.67024983212249,-2.55136949856929,
4.3998071879101));
#14658=CARTESIAN_POINT('Ctrl Pts',(-3.62022748800484,-2.57458468250198,
4.40351178426236));
#14659=CARTESIAN_POINT('Ctrl Pts',(-3.55755927628983,-2.57055119400479,
4.40721638061464));
#14660=CARTESIAN_POINT('Ctrl Pts',(-3.51092561732084,-2.54111518112976,
4.4109209769669));
#14661=CARTESIAN_POINT('Ctrl Pts',(-3.46429195835185,-2.51167916825472,
4.41462557331917));
#14662=CARTESIAN_POINT('Ctrl Pts',(-3.43369285212889,-2.45684063100183,
4.41833016967144));
#14663=CARTESIAN_POINT('Ctrl Pts',(-3.433132174149,-2.40169663743424,4.4220347660237));
#14664=CARTESIAN_POINT('Ctrl Pts',(-3.4325714961691,-2.34655264386664,4.42573936237597));
#14665=CARTESIAN_POINT('Ctrl Pts',(-3.46204924643229,-2.29110319398435,
4.42944395872824));
#14666=CARTESIAN_POINT('Ctrl Pts',(-3.50807475488023,-2.26072509261964,
4.43314855508051));
#14667=CARTESIAN_POINT('Ctrl Pts',(-3.55410026332817,-2.23034699125494,
4.43685315143278));
#14668=CARTESIAN_POINT('Ctrl Pts',(-3.61667352996086,-2.22504023840783,
4.44055774778505));
#14669=CARTESIAN_POINT('Ctrl Pts',(-3.66715754973313,-2.24723347480277,
4.44426234413731));
#14670=CARTESIAN_POINT('Ctrl Pts',(-3.71764156950539,-2.26942671119771,
4.44796694048958));
#14671=CARTESIAN_POINT('Ctrl Pts',(-3.75603634241723,-2.3191199368347,4.45167153684185));
#14672=CARTESIAN_POINT('Ctrl Pts',(-3.76477028031358,-2.37357077761011,
4.45537613319412));
#14673=CARTESIAN_POINT('Ctrl Pts',(-3.76616275698799,-2.38225203073804,
4.45596676757575));
#14674=CARTESIAN_POINT('Ctrl Pts',(-3.76680128976178,-2.39105421690488,
4.45655740195739));
#14675=CARTESIAN_POINT('Ctrl Pts',(-3.76672469163696,-2.39986752250016,
4.45714803633902));
#14676=CARTESIAN_POINT('Origin',(-3.6,-2.4,4.7));
#14677=CARTESIAN_POINT('',(-3.76633791767176,-2.39996197521538,4.52714803633902));
#14678=CARTESIAN_POINT('',(-3.76649857915956,-2.40014312937522,4.50785196366098));
#14679=CARTESIAN_POINT('',(-3.7666,-2.4,4.7));
#14680=CARTESIAN_POINT('Ctrl Pts',(-3.76649857915956,-2.40014312937522,
4.50785196366098));
#14681=CARTESIAN_POINT('Ctrl Pts',(-3.76617946285532,-2.36119271347016,
4.50525071011481));
#14682=CARTESIAN_POINT('Ctrl Pts',(-3.75254367029535,-2.32204100961925,
4.50264945656865));
#14683=CARTESIAN_POINT('Ctrl Pts',(-3.7275842614224,-2.29243603978678,4.50004820302248));
#14684=CARTESIAN_POINT('Ctrl Pts',(-3.69203811667935,-2.25027388169498,
4.49634360667021));
#14685=CARTESIAN_POINT('Ctrl Pts',(-3.63352511503972,-2.22747466102272,
4.49263901031794));
#14686=CARTESIAN_POINT('Ctrl Pts',(-3.57882406120147,-2.23447257256027,
4.48893441396567));
#14687=CARTESIAN_POINT('Ctrl Pts',(-3.52412300736323,-2.24147048409781,
4.4852298176134));
#14688=CARTESIAN_POINT('Ctrl Pts',(-3.47323390132638,-2.27826552784516,
4.48152522126114));
#14689=CARTESIAN_POINT('Ctrl Pts',(-3.44944643562249,-2.32801823904553,
4.47782062490887));
#14690=CARTESIAN_POINT('Ctrl Pts',(-3.42565896991859,-2.37777095024589,
4.4741160285566));
#14691=CARTESIAN_POINT('Ctrl Pts',(-3.42897314454765,-2.44048132889927,
4.47041143220433));
#14692=CARTESIAN_POINT('Ctrl Pts',(-3.45787219950101,-2.4874496233209,4.46670683585206));
#14693=CARTESIAN_POINT('Ctrl Pts',(-3.48677125445436,-2.53441791774253,
4.46300223949979));
#14694=CARTESIAN_POINT('Ctrl Pts',(-3.54125518973201,-2.56564412793241,
4.45929764314753));
#14695=CARTESIAN_POINT('Ctrl Pts',(-3.59638914182557,-2.56683738431542,
4.45559304679526));
#14696=CARTESIAN_POINT('Ctrl Pts',(-3.65152309391912,-2.56803064069842,
4.45188845044299));
#14697=CARTESIAN_POINT('Ctrl Pts',(-3.7073070628286,-2.53919094327454,4.44818385409072));
#14698=CARTESIAN_POINT('Ctrl Pts',(-3.73821116198855,-2.49351697797843,
4.44447925773846));
#14699=CARTESIAN_POINT('Ctrl Pts',(-3.75663967023947,-2.4662810102851,4.44227015971263));
#14700=CARTESIAN_POINT('Ctrl Pts',(-3.76622117317942,-2.43305896393576,
4.4400610616868));
#14701=CARTESIAN_POINT('Ctrl Pts',(-3.76637108132843,-2.3999167674636,4.43785196366098));
#14702=CARTESIAN_POINT('Ctrl Pts',(-3.76672469163696,-2.39986752250016,
4.45714803633902));
#14703=CARTESIAN_POINT('Ctrl Pts',(-3.76632084848944,-2.44633332149978,
4.46026199830965));
#14704=CARTESIAN_POINT('Ctrl Pts',(-3.74603891301781,-2.49310820101244,
4.46337596028029));
#14705=CARTESIAN_POINT('Ctrl Pts',(-3.71156690339415,-2.52409905358083,
4.46648992225092));
#14706=CARTESIAN_POINT('Ctrl Pts',(-3.67055648569751,-2.56096803286229,
4.47019451860319));
#14707=CARTESIAN_POINT('Ctrl Pts',(-3.60946254742337,-2.57549753551134,
4.47389911495546));
#14708=CARTESIAN_POINT('Ctrl Pts',(-3.55624507519594,-2.56103805534263,
4.47760371130773));
#14709=CARTESIAN_POINT('Ctrl Pts',(-3.5030276029685,-2.54657857517392,4.48130830765999));
#14710=CARTESIAN_POINT('Ctrl Pts',(-3.45768659678778,-2.50313011218745,
4.48501290401226));
#14711=CARTESIAN_POINT('Ctrl Pts',(-3.44097262555956,-2.45057710029542,
4.48871750036453));
#14712=CARTESIAN_POINT('Ctrl Pts',(-3.42425865433133,-2.39802408840339,
4.4924220967168));
#14713=CARTESIAN_POINT('Ctrl Pts',(-3.43617171805559,-2.33636652760581,
4.49612669306907));
#14714=CARTESIAN_POINT('Ctrl Pts',(-3.47125973540437,-2.29382235099447,
4.49983128942134));
#14715=CARTESIAN_POINT('Ctrl Pts',(-3.50634775275315,-2.25127817438312,
4.5035358857736));
#14716=CARTESIAN_POINT('Ctrl Pts',(-3.56461072372645,-2.22784738195801,
4.50724048212587));
#14717=CARTESIAN_POINT('Ctrl Pts',(-3.61938426936618,-2.23425320834927,
4.51094507847814));
#14718=CARTESIAN_POINT('Ctrl Pts',(-3.67415781500591,-2.24065903474052,
4.51464967483041));
#14719=CARTESIAN_POINT('Ctrl Pts',(-3.72544193531206,-2.27690147994813,
4.51835427118268));
#14720=CARTESIAN_POINT('Ctrl Pts',(-3.74976616178516,-2.3263939836064,4.52205886753495));
#14721=CARTESIAN_POINT('Ctrl Pts',(-3.76090458576616,-2.34905733490504,
4.52375525713631));
#14722=CARTESIAN_POINT('Ctrl Pts',(-3.76638989772718,-2.37449903782319,
4.52545164673766));
#14723=CARTESIAN_POINT('Ctrl Pts',(-3.76633791767176,-2.39996197521538,
4.52714803633902));
#14724=CARTESIAN_POINT('Origin',(-3.6,-2.4,4.7));
#14725=CARTESIAN_POINT('',(-3.7665852438883,-2.4001523433009,4.59714803633902));
#14726=CARTESIAN_POINT('',(-3.76687644757351,-2.39999932887962,4.57785196366098));
#14727=CARTESIAN_POINT('',(-3.7666,-2.4,4.7));
#14728=CARTESIAN_POINT('Ctrl Pts',(-3.76687644620932,-2.39999932888293,
4.57785196366098));
#14729=CARTESIAN_POINT('Ctrl Pts',(-3.76687974213825,-2.34481655618538,
4.57414495489509));
#14730=CARTESIAN_POINT('Ctrl Pts',(-3.73679498392134,-2.28963687265016,
4.57043794612919));
#14731=CARTESIAN_POINT('Ctrl Pts',(-3.69041339984634,-2.25973893422683,
4.5667309373633));
#14732=CARTESIAN_POINT('Ctrl Pts',(-3.64406199955899,-2.22986045251336,
4.56302634101103));
#14733=CARTESIAN_POINT('Ctrl Pts',(-3.58143498915818,-2.22523082136041,
4.55932174465877));
#14734=CARTESIAN_POINT('Ctrl Pts',(-3.53119397503756,-2.24796881775056,
4.5556171483065));
#14735=CARTESIAN_POINT('Ctrl Pts',(-3.48095296091694,-2.27070681414072,
4.55191255195423));
#14736=CARTESIAN_POINT('Ctrl Pts',(-3.44309794307651,-2.32081243807398,
4.54820795560196));
#14737=CARTESIAN_POINT('Ctrl Pts',(-3.43495348515474,-2.3753545665717,4.54450335924969));
#14738=CARTESIAN_POINT('Ctrl Pts',(-3.42680902723298,-2.42989669506942,
4.54079876289742));
#14739=CARTESIAN_POINT('Ctrl Pts',(-3.44837512922987,-2.4888753281316,4.53709416654516));
#14740=CARTESIAN_POINT('Ctrl Pts',(-3.48978194213576,-2.52529856004066,
4.53338957019289));
#14741=CARTESIAN_POINT('Ctrl Pts',(-3.53118875504166,-2.56172179194972,
4.52968497384062));
#14742=CARTESIAN_POINT('Ctrl Pts',(-3.59243627885656,-2.57558962270566,
4.52598037748835));
#14743=CARTESIAN_POINT('Ctrl Pts',(-3.64549423729516,-2.5605553606569,4.52227578113609));
#14744=CARTESIAN_POINT('Ctrl Pts',(-3.69855219573377,-2.54552109860814,
4.51857118478382));
#14745=CARTESIAN_POINT('Ctrl Pts',(-3.74342058879608,-2.50158474375469,
4.51486658843155));
#14746=CARTESIAN_POINT('Ctrl Pts',(-3.759565141404,-2.4488540185723,4.51116199207928));
#14747=CARTESIAN_POINT('Ctrl Pts',(-3.76437348603424,-2.43314918577593,
4.51005864927318));
#14748=CARTESIAN_POINT('Ctrl Pts',(-3.76663393493028,-2.41666426444364,
4.50895530646708));
#14749=CARTESIAN_POINT('Ctrl Pts',(-3.76649857915956,-2.40014312937522,
4.50785196366098));
#14750=CARTESIAN_POINT('Ctrl Pts',(-3.76633791767176,-2.39996197521538,
4.52714803633902));
#14751=CARTESIAN_POINT('Ctrl Pts',(-3.76627638304661,-2.43010531182154,
4.52915624308993));
#14752=CARTESIAN_POINT('Ctrl Pts',(-3.75845482433377,-2.46027840666142,
4.53116444984084));
#14753=CARTESIAN_POINT('Ctrl Pts',(-3.74306538783811,-2.48590718051351,
4.53317265659175));
#14754=CARTESIAN_POINT('Ctrl Pts',(-3.71467605477792,-2.53318531165342,
4.53687725294402));
#14755=CARTESIAN_POINT('Ctrl Pts',(-3.66053305601751,-2.56499901182434,
4.54058184929628));
#14756=CARTESIAN_POINT('Ctrl Pts',(-3.60541524194112,-2.56678856079501,
4.54428644564855));
#14757=CARTESIAN_POINT('Ctrl Pts',(-3.55029742786473,-2.56857810976569,
4.54799104200082));
#14758=CARTESIAN_POINT('Ctrl Pts',(-3.49420479847236,-2.54034350753613,
4.55169563835309));
#14759=CARTESIAN_POINT('Ctrl Pts',(-3.46280846367734,-2.49500647989383,
4.55540023470536));
#14760=CARTESIAN_POINT('Ctrl Pts',(-3.43141212888233,-2.44966945225154,
4.55910483105763));
#14761=CARTESIAN_POINT('Ctrl Pts',(-3.42471208868465,-2.38722999919651,
4.56280942740989));
#14762=CARTESIAN_POINT('Ctrl Pts',(-3.44577465447007,-2.33626389048712,
4.56651402376216));
#14763=CARTESIAN_POINT('Ctrl Pts',(-3.46683722025548,-2.28529778177773,
4.57021862011443));
#14764=CARTESIAN_POINT('Ctrl Pts',(-3.515662392024,-2.24580501741397,4.5739232164667));
#14765=CARTESIAN_POINT('Ctrl Pts',(-3.56990505305945,-2.23585968494016,
4.57762781281897));
#14766=CARTESIAN_POINT('Ctrl Pts',(-3.62414771409491,-2.22591435246634,
4.58133240917123));
#14767=CARTESIAN_POINT('Ctrl Pts',(-3.68380786439731,-2.24551645188247,
4.5850370055235));
#14768=CARTESIAN_POINT('Ctrl Pts',(-3.72158169788407,-2.28569497124226,
4.58874160187577));
#14769=CARTESIAN_POINT('Ctrl Pts',(-3.75015370460556,-2.31608587465984,
4.59154374669686));
#14770=CARTESIAN_POINT('Ctrl Pts',(-3.76620375900909,-2.35824929108539,
4.59434589151794));
#14771=CARTESIAN_POINT('Ctrl Pts',(-3.7665852438883,-2.4001523433009,4.59714803633902));
#14772=CARTESIAN_POINT('Origin',(-3.6,-2.4,4.7));
#14773=CARTESIAN_POINT('',(-3.76685427080137,-2.39994496470643,4.66714803633902));
#14774=CARTESIAN_POINT('',(-3.76649662121988,-2.39985729252779,4.64785196366098));
#14775=CARTESIAN_POINT('',(-3.7666,-2.4,4.7));
#14776=CARTESIAN_POINT('Ctrl Pts',(-3.76649662121988,-2.39985729252779,
4.64785196366098));
#14777=CARTESIAN_POINT('Ctrl Pts',(-3.76663205173418,-2.38326341802857,
4.64674379602763));
#14778=CARTESIAN_POINT('Ctrl Pts',(-3.76435139460867,-2.36670593234144,
4.64563562839428));
#14779=CARTESIAN_POINT('Ctrl Pts',(-3.7595015341574,-2.35093871131677,4.64452746076093));
#14780=CARTESIAN_POINT('Ctrl Pts',(-3.74328848588199,-2.29822900591163,
4.64082286440866));
#14781=CARTESIAN_POINT('Ctrl Pts',(-3.69836304774957,-2.25435098262799,
4.63711826805639));
#14782=CARTESIAN_POINT('Ctrl Pts',(-3.64528560126629,-2.23938566762668,
4.63341367170413));
#14783=CARTESIAN_POINT('Ctrl Pts',(-3.59220815478301,-2.22442035262536,
4.62970907535186));
#14784=CARTESIAN_POINT('Ctrl Pts',(-3.53097869994887,-2.23836774590636,
4.62600447899959));
#14785=CARTESIAN_POINT('Ctrl Pts',(-3.48961924396277,-2.27484474384805,
4.62229988264732));
#14786=CARTESIAN_POINT('Ctrl Pts',(-3.44825978797668,-2.31132174178974,
4.61859528629506));
#14787=CARTESIAN_POINT('Ctrl Pts',(-3.42677033083864,-2.37032834439211,
4.61489068994278));
#14788=CARTESIAN_POINT('Ctrl Pts',(-3.43498564446249,-2.42485984538296,
4.61118609359052));
#14789=CARTESIAN_POINT('Ctrl Pts',(-3.44320095808634,-2.47939134637381,
4.60748149723825));
#14790=CARTESIAN_POINT('Ctrl Pts',(-3.48112104247208,-2.52944774575313,
4.60377690088598));
#14791=CARTESIAN_POINT('Ctrl Pts',(-3.53139155597687,-2.55212044850799,
4.60007230453371));
#14792=CARTESIAN_POINT('Ctrl Pts',(-3.58166206948165,-2.57479315126284,
4.59636770818145));
#14793=CARTESIAN_POINT('Ctrl Pts',(-3.64428301210547,-2.57008215739322,
4.59266311182917));
#14794=CARTESIAN_POINT('Ctrl Pts',(-3.69059555437608,-2.54014347995252,
4.58895851547691));
#14795=CARTESIAN_POINT('Ctrl Pts',(-3.73687793816318,-2.51022429842083,
4.58525633153826));
#14796=CARTESIAN_POINT('Ctrl Pts',(-3.76687315457017,-2.45511027888938,
4.58155414759962));
#14797=CARTESIAN_POINT('Ctrl Pts',(-3.76687644620932,-2.39999932888293,
4.57785196366098));
#14798=CARTESIAN_POINT('Ctrl Pts',(-3.7665852438883,-2.4001523433009,4.59714803633902));
#14799=CARTESIAN_POINT('Ctrl Pts',(-3.76670810392422,-2.41364753218216,
4.59805048787021));
#14800=CARTESIAN_POINT('Ctrl Pts',(-3.76520580454733,-2.42711571583196,
4.59895293940139));
#14801=CARTESIAN_POINT('Ctrl Pts',(-3.76197323580484,-2.44015494667501,
4.59985539093257));
#14802=CARTESIAN_POINT('Ctrl Pts',(-3.74870342356775,-2.49368146344449,
4.60355998728484));
#14803=CARTESIAN_POINT('Ctrl Pts',(-3.70627628242244,-2.53997955767999,
4.60726458363711));
#14804=CARTESIAN_POINT('Ctrl Pts',(-3.65410883409218,-2.55786064402731,
4.61096917998938));
#14805=CARTESIAN_POINT('Ctrl Pts',(-3.60194138576191,-2.57574173037463,
4.61467377634165));
#14806=CARTESIAN_POINT('Ctrl Pts',(-3.54003363024668,-2.56520580883379,
4.61837837269391));
#14807=CARTESIAN_POINT('Ctrl Pts',(-3.49671800289895,-2.53107470364031,
4.62208296904618));
#14808=CARTESIAN_POINT('Ctrl Pts',(-3.45340237555123,-2.49694359844684,
4.62578756539845));
#14809=CARTESIAN_POINT('Ctrl Pts',(-3.42867887637101,-2.43921730960073,
4.62949216175072));
#14810=CARTESIAN_POINT('Ctrl Pts',(-3.43386235494986,-2.38431460052291,
4.63319675810299));
#14811=CARTESIAN_POINT('Ctrl Pts',(-3.43904583352872,-2.3294118914451,4.63690135445526));
#14812=CARTESIAN_POINT('Ctrl Pts',(-3.47413628986665,-2.27733276213558,
4.64060595080752));
#14813=CARTESIAN_POINT('Ctrl Pts',(-3.52307437764419,-2.25191152143151,
4.64431054715979));
#14814=CARTESIAN_POINT('Ctrl Pts',(-3.57201246542174,-2.22649028072744,
4.64801514351206));
#14815=CARTESIAN_POINT('Ctrl Pts',(-3.6347981846389,-2.22772692862883,4.65171973986433));
#14816=CARTESIAN_POINT('Ctrl Pts',(-3.68269729487669,-2.25505550621137,
4.65542433621659));
#14817=CARTESIAN_POINT('Ctrl Pts',(-3.73059640511449,-2.28238408379392,
4.65912893256886));
#14818=CARTESIAN_POINT('Ctrl Pts',(-3.76360890637291,-2.33580459105762,
4.66283352892113));
#14819=CARTESIAN_POINT('Ctrl Pts',(-3.76662644025744,-2.39086882993835,
4.6665381252734));
#14820=CARTESIAN_POINT('Ctrl Pts',(-3.76679203880333,-2.3938906876002,4.66674142896194));
#14821=CARTESIAN_POINT('Ctrl Pts',(-3.76686730212629,-2.39691749565456,
4.66694473265048));
#14822=CARTESIAN_POINT('Ctrl Pts',(-3.76685427080137,-2.39994496470643,
4.66714803633902));
#14823=CARTESIAN_POINT('Origin',(-3.6,-2.4,4.7));
#14824=CARTESIAN_POINT('',(-3.7664227625968,-2.39988235338239,4.73714803633902));
#14825=CARTESIAN_POINT('',(-3.76637219995946,-2.40008425137793,4.71785196366098));
#14826=CARTESIAN_POINT('',(-3.7666,-2.4,4.7));
#14827=CARTESIAN_POINT('Ctrl Pts',(-3.76637219995946,-2.40008425137793,
4.71785196366098));
#14828=CARTESIAN_POINT('Ctrl Pts',(-3.76622009461901,-2.36687021016323,
4.7156380408079));
#14829=CARTESIAN_POINT('Ctrl Pts',(-3.7565937463241,-2.33357496437374,4.71342411795483));
#14830=CARTESIAN_POINT('Ctrl Pts',(-3.73808953535598,-2.30630352370031,
4.71121019510175));
#14831=CARTESIAN_POINT('Ctrl Pts',(-3.70712611115225,-2.26066973862981,
4.70750559874949));
#14832=CARTESIAN_POINT('Ctrl Pts',(-3.65130474062691,-2.23190256095558,
4.70380100239722));
#14833=CARTESIAN_POINT('Ctrl Pts',(-3.5961723905296,-2.23316745266121,4.70009640604495));
#14834=CARTESIAN_POINT('Ctrl Pts',(-3.54104004043228,-2.23443234436684,
4.69639180969269));
#14835=CARTESIAN_POINT('Ctrl Pts',(-3.48659671076299,-2.26572930545233,
4.69268721334042));
#14836=CARTESIAN_POINT('Ctrl Pts',(-3.45775870005953,-2.31273510421107,
4.68898261698815));
#14837=CARTESIAN_POINT('Ctrl Pts',(-3.42892068935607,-2.35974090296982,
4.68527802063588));
#14838=CARTESIAN_POINT('Ctrl Pts',(-3.42568799761845,-2.42245553940182,
4.68157342428361));
#14839=CARTESIAN_POINT('Ctrl Pts',(-3.44954008455102,-2.47217730452778,
4.67786882793134));
#14840=CARTESIAN_POINT('Ctrl Pts',(-3.47339217148359,-2.52189906965374,
4.67416423157907));
#14841=CARTESIAN_POINT('Ctrl Pts',(-3.52432903708635,-2.55862796347366,
4.6704596352268));
#14842=CARTESIAN_POINT('Ctrl Pts',(-3.57903913598448,-2.56555479946389,
4.66675503887454));
#14843=CARTESIAN_POINT('Ctrl Pts',(-3.63374923488261,-2.57248163545412,
4.66305044252227));
#14844=CARTESIAN_POINT('Ctrl Pts',(-3.69223256707613,-2.54960641361466,
4.65934584617));
#14845=CARTESIAN_POINT('Ctrl Pts',(-3.72772390396368,-2.50739810893161,
4.65564124981774));
#14846=CARTESIAN_POINT('Ctrl Pts',(-3.75259860490409,-2.47781570803419,
4.65304482109882));
#14847=CARTESIAN_POINT('Ctrl Pts',(-3.76617930850818,-2.43873661999706,
4.6504483923799));
#14848=CARTESIAN_POINT('Ctrl Pts',(-3.76649662121988,-2.39985729252779,
4.64785196366098));
#14849=CARTESIAN_POINT('Ctrl Pts',(-3.76685427080137,-2.39994496470643,
4.66714803633902));
#14850=CARTESIAN_POINT('Ctrl Pts',(-3.76662984554536,-2.45208398518876,
4.67064932900275));
#14851=CARTESIAN_POINT('Ctrl Pts',(-3.74021751929721,-2.50441905534817,
4.67415062166648));
#14852=CARTESIAN_POINT('Ctrl Pts',(-3.6980405151982,-2.53504001717725,4.6776519143302));
#14853=CARTESIAN_POINT('Ctrl Pts',(-3.65341448974379,-2.56743899503768,
4.68135651068247));
#14854=CARTESIAN_POINT('Ctrl Pts',(-3.59113987232435,-2.57552898026078,
4.68506110703474));
#14855=CARTESIAN_POINT('Ctrl Pts',(-3.53971699472298,-2.55560754523587,
4.68876570338701));
#14856=CARTESIAN_POINT('Ctrl Pts',(-3.48829411712161,-2.53568611021095,
4.69247029973928));
#14857=CARTESIAN_POINT('Ctrl Pts',(-3.4477229793383,-2.48775325493802,4.69617489609154));
#14858=CARTESIAN_POINT('Ctrl Pts',(-3.4365711926336,-2.4337457224305,4.69987949244381));
#14859=CARTESIAN_POINT('Ctrl Pts',(-3.42541940592889,-2.37973818992299,
4.70358408879608));
#14860=CARTESIAN_POINT('Ctrl Pts',(-3.44368697030278,-2.31965598018089,
4.70728868514835));
#14861=CARTESIAN_POINT('Ctrl Pts',(-3.48301363133541,-2.28099605718198,
4.71099328150062));
#14862=CARTESIAN_POINT('Ctrl Pts',(-3.52234029236805,-2.24233613418307,
4.71469787785288));
#14863=CARTESIAN_POINT('Ctrl Pts',(-3.58272605005944,-2.22509849792735,
4.71840247420515));
#14864=CARTESIAN_POINT('Ctrl Pts',(-3.63653501999159,-2.23717205039129,
4.72210707055742));
#14865=CARTESIAN_POINT('Ctrl Pts',(-3.69034398992373,-2.24924560285524,
4.72581166690969));
#14866=CARTESIAN_POINT('Ctrl Pts',(-3.73757617209662,-2.29063034403885,
4.72951626326196));
#14867=CARTESIAN_POINT('Ctrl Pts',(-3.75661549051415,-2.342386312472,4.73322085961422));
#14868=CARTESIAN_POINT('Ctrl Pts',(-3.76334323815838,-2.36067483977454,
4.73452991852249));
#14869=CARTESIAN_POINT('Ctrl Pts',(-3.76655071734768,-2.38025835805218,
4.73583897743076));
#14870=CARTESIAN_POINT('Ctrl Pts',(-3.7664227625968,-2.39988235338239,4.73714803633902));
#14871=CARTESIAN_POINT('Origin',(-3.6,-2.4,4.7));
#14872=CARTESIAN_POINT('',(-3.76642911325459,-2.40012064491874,4.80714803633902));
#14873=CARTESIAN_POINT('',(-3.76680409091049,-2.40009747380892,4.78785196366098));
#14874=CARTESIAN_POINT('',(-3.7666,-2.4,4.7));
#14875=CARTESIAN_POINT('Ctrl Pts',(-3.76680409091049,-2.40009747380892,
4.78785196366098));
#14876=CARTESIAN_POINT('Ctrl Pts',(-3.76646019447366,-2.35062358790434,
4.78453228558818));
#14877=CARTESIAN_POINT('Ctrl Pts',(-3.74304697023447,-2.30086701998663,
4.78121260751538));
#14878=CARTESIAN_POINT('Ctrl Pts',(-3.70452480595454,-2.26991420375009,
4.77789292944258));
#14879=CARTESIAN_POINT('Ctrl Pts',(-3.66153597807928,-2.23537239348787,
4.77418833309031));
#14880=CARTESIAN_POINT('Ctrl Pts',(-3.59973129997326,-2.22424775044289,
4.77048373673805));
#14881=CARTESIAN_POINT('Ctrl Pts',(-3.54739603302806,-2.24163153058572,
4.76677914038578));
#14882=CARTESIAN_POINT('Ctrl Pts',(-3.49506076608285,-2.25901531072854,
4.76307454403351));
#14883=CARTESIAN_POINT('Ctrl Pts',(-3.45219491029846,-2.30490751405916,
4.75936994768124));
#14884=CARTESIAN_POINT('Ctrl Pts',(-3.43841626764055,-2.35830531349683,
4.75566535132897));
#14885=CARTESIAN_POINT('Ctrl Pts',(-3.42463762498264,-2.4117031129345,4.7519607549767));
#14886=CARTESIAN_POINT('Ctrl Pts',(-3.4399461954512,-2.47260650847922,4.74825615862444));
#14887=CARTESIAN_POINT('Ctrl Pts',(-3.47733592496581,-2.51314271581421,
4.74455156227217));
#14888=CARTESIAN_POINT('Ctrl Pts',(-3.51472565448041,-2.55367892314919,
4.7408469659199));
#14889=CARTESIAN_POINT('Ctrl Pts',(-3.57419654304106,-2.57384794227444,
4.73714236956763));
#14890=CARTESIAN_POINT('Ctrl Pts',(-3.62853140127509,-2.56441930722117,
4.73343777321536));
#14891=CARTESIAN_POINT('Ctrl Pts',(-3.68286625950912,-2.55499067216789,
4.7297331768631));
#14892=CARTESIAN_POINT('Ctrl Pts',(-3.73206508741654,-2.5159643829361,4.72602858051083));
#14893=CARTESIAN_POINT('Ctrl Pts',(-3.75361176242918,-2.46520104208683,
4.72232398415856));
#14894=CARTESIAN_POINT('Ctrl Pts',(-3.7622818183227,-2.4447746420856,4.72083331065936));
#14895=CARTESIAN_POINT('Ctrl Pts',(-3.76647461518129,-2.42244785405319,
4.71934263716017));
#14896=CARTESIAN_POINT('Ctrl Pts',(-3.76637219995946,-2.40008425137793,
4.71785196366098));
#14897=CARTESIAN_POINT('Ctrl Pts',(-3.7664227625968,-2.39988235338239,4.73714803633902));
#14898=CARTESIAN_POINT('Ctrl Pts',(-3.76618860934753,-2.43579365983134,
4.73954357378302));
#14899=CARTESIAN_POINT('Ctrl Pts',(-3.75478479773435,-2.47184051531438,
4.74193911122703));
#14900=CARTESIAN_POINT('Ctrl Pts',(-3.73334402642865,-2.50033503613074,
4.74433464867103));
#14901=CARTESIAN_POINT('Ctrl Pts',(-3.70018678926345,-2.54440059567364,
4.7480392450233));
#14902=CARTESIAN_POINT('Ctrl Pts',(-3.64302586027087,-2.57040451907673,
4.75174384137556));
#14903=CARTESIAN_POINT('Ctrl Pts',(-3.58802126272889,-2.56644596334232,
4.75544843772783));
#14904=CARTESIAN_POINT('Ctrl Pts',(-3.53301666518691,-2.56248740760791,
4.7591530340801));
#14905=CARTESIAN_POINT('Ctrl Pts',(-3.48016839909552,-2.52856637273599,
4.76285763043237));
#14906=CARTESIAN_POINT('Ctrl Pts',(-3.4536627731015,-2.48020701268106,4.76656222678464));
#14907=CARTESIAN_POINT('Ctrl Pts',(-3.42715714710748,-2.43184765262612,
4.77026682313691));
#14908=CARTESIAN_POINT('Ctrl Pts',(-3.42699416121083,-2.36904996738817,
4.77397141948918));
#14909=CARTESIAN_POINT('Ctrl Pts',(-3.45324840683133,-2.32055367370344,
4.77767601584144));
#14910=CARTESIAN_POINT('Ctrl Pts',(-3.47950265245184,-2.2720573800187,4.78138061219371));
#14911=CARTESIAN_POINT('Ctrl Pts',(-3.53217412958951,-2.23786247788719,
4.78508520854597));
#14912=CARTESIAN_POINT('Ctrl Pts',(-3.58715743806471,-2.23361845816768,
4.78878980489824));
#14913=CARTESIAN_POINT('Ctrl Pts',(-3.6421407465399,-2.22937443844816,4.79249440125051));
#14914=CARTESIAN_POINT('Ctrl Pts',(-3.69943588635261,-2.25508130114064,
4.79619899760278));
#14915=CARTESIAN_POINT('Ctrl Pts',(-3.73282141188201,-2.29897415476607,
4.79990359395505));
#14916=CARTESIAN_POINT('Ctrl Pts',(-3.75458352333835,-2.32758539144982,
4.80231840808304));
#14917=CARTESIAN_POINT('Ctrl Pts',(-3.76618646552292,-2.36392383602884,
4.80473322221103));
#14918=CARTESIAN_POINT('Ctrl Pts',(-3.76642911325459,-2.40012064491874,
4.80714803633902));
#14919=CARTESIAN_POINT('Origin',(-3.6,-2.4,4.7));
#14920=CARTESIAN_POINT('',(-3.76685810224694,-2.40005005741615,4.87714803633902));
#14921=CARTESIAN_POINT('',(-3.76666750911963,-2.3998541249347,4.85785196366098));
#14922=CARTESIAN_POINT('',(-3.7666,-2.4,4.7));
#14923=CARTESIAN_POINT('Ctrl Pts',(-3.76666750911963,-2.3998541249347,4.85785196366098));
#14924=CARTESIAN_POINT('Ctrl Pts',(-3.76676617376365,-2.38908842257499,
4.85713112672072));
#14925=CARTESIAN_POINT('Ctrl Pts',(-3.76581236816026,-2.37834012863908,
4.85641028978047));
#14926=CARTESIAN_POINT('Ctrl Pts',(-3.76374257749965,-2.36781121686714,
4.85568945284021));
#14927=CARTESIAN_POINT('Ctrl Pts',(-3.75310530504175,-2.31369999425172,
4.85198485648794));
#14928=CARTESIAN_POINT('Ctrl Pts',(-3.71299219872321,-2.26538317916478,
4.84828026013567));
#14929=CARTESIAN_POINT('Ctrl Pts',(-3.66176124910748,-2.24497323600586,
4.8445756637834));
#14930=CARTESIAN_POINT('Ctrl Pts',(-3.61053029949175,-2.22456329284695,
4.84087106743114));
#14931=CARTESIAN_POINT('Ctrl Pts',(-3.54818150657882,-2.23206022161606,
4.83716647107887));
#14932=CARTESIAN_POINT('Ctrl Pts',(-3.50324914898701,-2.26403301035152,
4.8334618747266));
#14933=CARTESIAN_POINT('Ctrl Pts',(-3.45831679139521,-2.29600579908698,
4.82975727837433));
#14934=CARTESIAN_POINT('Ctrl Pts',(-3.43080086912452,-2.35245444778878,
4.82605268202206));
#14935=CARTESIAN_POINT('Ctrl Pts',(-3.43329420002801,-2.40754491229296,
4.82234808566979));
#14936=CARTESIAN_POINT('Ctrl Pts',(-3.43578753093151,-2.46263537679713,
4.81864348931753));
#14937=CARTESIAN_POINT('Ctrl Pts',(-3.4682901150092,-2.51636765710367,4.81493889296526));
#14938=CARTESIAN_POINT('Ctrl Pts',(-3.51592696035573,-2.54415087044753,
4.81123429661299));
#14939=CARTESIAN_POINT('Ctrl Pts',(-3.56356380570226,-2.5719340837914,4.80752970026073));
#14940=CARTESIAN_POINT('Ctrl Pts',(-3.62633491231765,-2.57376823017258,
4.80382510390846));
#14941=CARTESIAN_POINT('Ctrl Pts',(-3.67551272732296,-2.54881390209942,
4.80012050755619));
#14942=CARTESIAN_POINT('Ctrl Pts',(-3.72469054232828,-2.52385957402626,
4.79641591120392));
#14943=CARTESIAN_POINT('Ctrl Pts',(-3.76027506572354,-2.47211677149876,
4.79271131485165));
#14944=CARTESIAN_POINT('Ctrl Pts',(-3.76598083859892,-2.41726588149528,
4.78900671849938));
#14945=CARTESIAN_POINT('Ctrl Pts',(-3.76657368490912,-2.41156671532445,
4.78862180021991));
#14946=CARTESIAN_POINT('Ctrl Pts',(-3.7668439658688,-2.40583399482793,4.78823688194045));
#14947=CARTESIAN_POINT('Ctrl Pts',(-3.76680409091049,-2.40009747380892,
4.78785196366098));
#14948=CARTESIAN_POINT('Ctrl Pts',(-3.76642911325459,-2.40012064491874,
4.80714803633902));
#14949=CARTESIAN_POINT('Ctrl Pts',(-3.76655871442242,-2.41945381020902,
4.8084378185633));
#14950=CARTESIAN_POINT('Ctrl Pts',(-3.76344749532011,-2.43874657022512,
4.80972760078758));
#14951=CARTESIAN_POINT('Ctrl Pts',(-3.75691244110645,-2.45679995321808,
4.81101738301185));
#14952=CARTESIAN_POINT('Ctrl Pts',(-3.73814203355539,-2.50865405348629,
4.81472197936412));
#14953=CARTESIAN_POINT('Ctrl Pts',(-3.69112530720718,-2.55028340946432,
4.81842657571639));
#14954=CARTESIAN_POINT('Ctrl Pts',(-3.63737973347804,-2.56263611033431,
4.82213117206866));
#14955=CARTESIAN_POINT('Ctrl Pts',(-3.58363415974891,-2.5749888112043,4.82583576842093));
#14956=CARTESIAN_POINT('Ctrl Pts',(-3.52315973863885,-2.55806485696625,
4.82954036477319));
#14957=CARTESIAN_POINT('Ctrl Pts',(-3.48363293188217,-2.51960959124259,
4.83324496112546));
#14958=CARTESIAN_POINT('Ctrl Pts',(-3.44410612512549,-2.48115432551893,
4.83694955747773));
#14959=CARTESIAN_POINT('Ctrl Pts',(-3.42552693272221,-2.42116774830966,
4.84065415383));
#14960=CARTESIAN_POINT('Ctrl Pts',(-3.43639822742686,-2.36710305682155,
4.84435875018227));
#14961=CARTESIAN_POINT('Ctrl Pts',(-3.44726952213151,-2.31303836533343,
4.84806334653454));
#14962=CARTESIAN_POINT('Ctrl Pts',(-3.48759130394411,-2.26489555956646,
4.8517679428868));
#14963=CARTESIAN_POINT('Ctrl Pts',(-3.53891008077804,-2.24470746756836,
4.85547253923907));
#14964=CARTESIAN_POINT('Ctrl Pts',(-3.59022885761198,-2.22451937557026,
4.85917713559134));
#14965=CARTESIAN_POINT('Ctrl Pts',(-3.65254462946725,-2.23228599734102,
4.86288173194361));
#14966=CARTESIAN_POINT('Ctrl Pts',(-3.69733822999987,-2.26445289438714,
4.86658632829587));
#14967=CARTESIAN_POINT('Ctrl Pts',(-3.73990669414912,-2.29502189057005,
4.87010689764359));
#14968=CARTESIAN_POINT('Ctrl Pts',(-3.76665058750282,-2.34762719015485,
4.87362746699131));
#14969=CARTESIAN_POINT('Ctrl Pts',(-3.76685810224694,-2.40005005741615,
4.87714803633902));
#14970=CARTESIAN_POINT('Origin',(-3.6,-2.4,4.7));
#14971=CARTESIAN_POINT('',(-3.76657660157387,-2.39984780956506,4.94714803633902));
#14972=CARTESIAN_POINT('',(-3.76633014204238,-2.3999936674641,4.92785196366098));
#14973=CARTESIAN_POINT('',(-3.7666,-2.4,4.7));
#14974=CARTESIAN_POINT('Ctrl Pts',(-3.76633014204238,-2.3999936674641,4.92785196366098));
#14975=CARTESIAN_POINT('Ctrl Pts',(-3.76633943871615,-2.37257318075516,
4.926025371501));
#14976=CARTESIAN_POINT('Ctrl Pts',(-3.75993532676097,-2.34515678209823,
4.92419877934102));
#14977=CARTESIAN_POINT('Ctrl Pts',(-3.74709395990921,-2.32118936363805,
4.92237218718104));
#14978=CARTESIAN_POINT('Ctrl Pts',(-3.72104978768541,-2.27257992966252,
4.91866759082877));
#14979=CARTESIAN_POINT('Ctrl Pts',(-3.66852675339565,-2.23815745462599,
4.9149629944765));
#14980=CARTESIAN_POINT('Ctrl Pts',(-3.61356232150655,-2.23367557941999,
4.91125839812423));
#14981=CARTESIAN_POINT('Ctrl Pts',(-3.55859788961746,-2.22919370421399,
4.90755380177196));
#14982=CARTESIAN_POINT('Ctrl Pts',(-3.50119206012902,-2.25465242883852,
4.90384920541969));
#14983=CARTESIAN_POINT('Ctrl Pts',(-3.4676169364208,-2.2984004236072,4.90014460906743));
#14984=CARTESIAN_POINT('Ctrl Pts',(-3.43404181271257,-2.34214841837589,
4.89644001271516));
#14985=CARTESIAN_POINT('Ctrl Pts',(-3.42429739478456,-2.40418568328873,
4.89273541636289));
#14986=CARTESIAN_POINT('Ctrl Pts',(-3.44284327075563,-2.45612051228373,
4.88903082001062));
#14987=CARTESIAN_POINT('Ctrl Pts',(-3.46138914672669,-2.50805534127872,
4.88532622365836));
#14988=CARTESIAN_POINT('Ctrl Pts',(-3.50822531659685,-2.54988773435588,
4.88162162730609));
#14989=CARTESIAN_POINT('Ctrl Pts',(-3.56191694164611,-2.56247285961735,
4.87791703095382));
#14990=CARTESIAN_POINT('Ctrl Pts',(-3.61560856669538,-2.57505798487881,
4.87421243460155));
#14991=CARTESIAN_POINT('Ctrl Pts',(-3.67615564692375,-2.55839584232458,
4.87050783824928));
#14992=CARTESIAN_POINT('Ctrl Pts',(-3.7158484677393,-2.52011195597552,4.86680324189701));
#14993=CARTESIAN_POINT('Ctrl Pts',(-3.74781789610229,-2.48927731291044,
4.863819482485));
#14994=CARTESIAN_POINT('Ctrl Pts',(-3.76625910668661,-2.44441658275108,
4.86083572307299));
#14995=CARTESIAN_POINT('Ctrl Pts',(-3.76666750911963,-2.3998541249347,4.85785196366098));
#14996=CARTESIAN_POINT('Ctrl Pts',(-3.76685810224694,-2.40005005741615,
4.87714803633902));
#14997=CARTESIAN_POINT('Ctrl Pts',(-3.76686894944607,-2.40279030260928,
4.87733206334357));
#14998=CARTESIAN_POINT('Ctrl Pts',(-3.76680728980785,-2.40553004933232,
4.87751609034813));
#14999=CARTESIAN_POINT('Ctrl Pts',(-3.76667159341225,-2.40826612418172,
4.87770011735268));
#15000=CARTESIAN_POINT('Ctrl Pts',(-3.76393992708203,-2.46334528460871,
4.88140471370495));
#15001=CARTESIAN_POINT('Ctrl Pts',(-3.73120516521163,-2.5169364331412,4.88510931005721));
#15002=CARTESIAN_POINT('Ctrl Pts',(-3.6834485571899,-2.54451327676931,4.88881390640948));
#15003=CARTESIAN_POINT('Ctrl Pts',(-3.63569194916816,-2.57209012039741,
4.89251850276175));
#15004=CARTESIAN_POINT('Ctrl Pts',(-3.57291349499508,-2.57365265912114,
4.89622309911402));
#15005=CARTESIAN_POINT('Ctrl Pts',(-3.52384411020076,-2.5484857882364,4.89992769546629));
#15006=CARTESIAN_POINT('Ctrl Pts',(-3.47477472540644,-2.52331891735167,
4.90363229181856));
#15007=CARTESIAN_POINT('Ctrl Pts',(-3.43941440999087,-2.47142263685848,
4.90733688817082));
#15008=CARTESIAN_POINT('Ctrl Pts',(-3.43394601281114,-2.41654757379038,
4.91104148452309));
#15009=CARTESIAN_POINT('Ctrl Pts',(-3.42847761563141,-2.36167251072229,
4.91474608087536));
#15010=CARTESIAN_POINT('Ctrl Pts',(-3.45290113668751,-2.30381866507929,
4.91845067722763));
#15011=CARTESIAN_POINT('Ctrl Pts',(-3.4960390130763,-2.2694631773857,4.9221552735799));
#15012=CARTESIAN_POINT('Ctrl Pts',(-3.53917688946509,-2.23510768969211,
4.92585986993217));
#15013=CARTESIAN_POINT('Ctrl Pts',(-3.60102912118658,-2.22425055994793,
4.92956446628443));
#15014=CARTESIAN_POINT('Ctrl Pts',(-3.65328868366947,-2.24186061512031,
4.9332690626367));
#15015=CARTESIAN_POINT('Ctrl Pts',(-3.70554824615237,-2.25947067029269,
4.93697365898897));
#15016=CARTESIAN_POINT('Ctrl Pts',(-3.74821513939667,-2.30554791038164,
4.94067825534123));
#15017=CARTESIAN_POINT('Ctrl Pts',(-3.76176261776726,-2.35900482523354,
4.9443828516935));
#15018=CARTESIAN_POINT('Ctrl Pts',(-3.76513332050279,-2.37230526124053,
4.94530457990868));
#15019=CARTESIAN_POINT('Ctrl Pts',(-3.76670139313906,-2.38606253416914,
4.94622630812385));
#15020=CARTESIAN_POINT('Ctrl Pts',(-3.76657660157387,-2.39984780956506,
4.94714803633902));
#15021=CARTESIAN_POINT('Origin',(-3.6,-2.4,4.7));
#15022=CARTESIAN_POINT('',(-3.76634000649331,-2.40004261214866,5.01714803633902));
#15023=CARTESIAN_POINT('',(-3.76664426409402,-2.40014916296054,4.99785196366098));
#15024=CARTESIAN_POINT('',(-3.7666,-2.4,4.7));
#15025=CARTESIAN_POINT('Ctrl Pts',(-3.76664426409402,-2.40014916296054,
4.99785196366098));
#15026=CARTESIAN_POINT('Ctrl Pts',(-3.76623994861442,-2.35633882629306,
4.99491961628127));
#15027=CARTESIAN_POINT('Ctrl Pts',(-3.74849621908403,-2.31223872253049,
4.99198726890157));
#15028=CARTESIAN_POINT('Ctrl Pts',(-3.71750016680111,-2.28150333241251,
4.98905492152186));
#15029=CARTESIAN_POINT('Ctrl Pts',(-3.678341142527,-2.24267361704367,4.98535032516959));
#15030=CARTESIAN_POINT('Ctrl Pts',(-3.61803053121903,-2.22517487203488,
4.98164572881732));
#15031=CARTESIAN_POINT('Ctrl Pts',(-3.56416982600182,-2.23701549741557,
4.97794113246506));
#15032=CARTESIAN_POINT('Ctrl Pts',(-3.51030912078461,-2.24885612279626,
4.97423653611279));
#15033=CARTESIAN_POINT('Ctrl Pts',(-3.46289832165815,-2.29003611856643,
4.97053193976052));
#15034=CARTESIAN_POINT('Ctrl Pts',(-3.44363524974256,-2.34170922607974,
4.96682734340825));
#15035=CARTESIAN_POINT('Ctrl Pts',(-3.42437217782697,-2.39338233359304,
4.96312274705598));
#15036=CARTESIAN_POINT('Ctrl Pts',(-3.43325683312225,-2.45554855284948,
4.95941815070371));
#15037=CARTESIAN_POINT('Ctrl Pts',(-3.46622310272193,-2.4997571611377,4.95571355435145));
#15038=CARTESIAN_POINT('Ctrl Pts',(-3.49918937232162,-2.54396576942592,
4.95200895799918));
#15039=CARTESIAN_POINT('Ctrl Pts',(-3.55623725622572,-2.57021676674591,
4.94830436164691));
#15040=CARTESIAN_POINT('Ctrl Pts',(-3.61125846689758,-2.56649623530203,
4.94459976529464));
#15041=CARTESIAN_POINT('Ctrl Pts',(-3.66627967756944,-2.56277570385816,
4.94089516894238));
#15042=CARTESIAN_POINT('Ctrl Pts',(-3.71927421500904,-2.52908364365041,
4.93719057259011));
#15043=CARTESIAN_POINT('Ctrl Pts',(-3.74598882864993,-2.48083941708926,
4.93348597623784));
#15044=CARTESIAN_POINT('Ctrl Pts',(-3.7595315068913,-2.45638253943781,4.93160797204555));
#15045=CARTESIAN_POINT('Ctrl Pts',(-3.76632058370052,-2.4281859427416,4.92972996785327));
#15046=CARTESIAN_POINT('Ctrl Pts',(-3.76633014204238,-2.3999936674641,4.92785196366098));
#15047=CARTESIAN_POINT('Ctrl Pts',(-3.76657660157387,-2.39984780956506,
4.94714803633902));
#15048=CARTESIAN_POINT('Ctrl Pts',(-3.76619983273375,-2.44146810829183,
4.94993090447612));
#15049=CARTESIAN_POINT('Ctrl Pts',(-3.75039179589374,-2.48334366291991,
4.95271377261321));
#15050=CARTESIAN_POINT('Ctrl Pts',(-3.7221733933057,-2.5136723837762,4.95549664075031));
#15051=CARTESIAN_POINT('Ctrl Pts',(-3.68460862697666,-2.55404643785209,
4.95920123710258));
#15052=CARTESIAN_POINT('Ctrl Pts',(-3.62505103082171,-2.57395795638902,
4.96290583345484));
#15053=CARTESIAN_POINT('Ctrl Pts',(-3.57075747641916,-2.56429432021831,
4.96661042980711));
#15054=CARTESIAN_POINT('Ctrl Pts',(-3.51646392201662,-2.5546306840476,4.97031502615938));
#15055=CARTESIAN_POINT('Ctrl Pts',(-3.46743440936648,-2.51539189316926,
4.97401962251165));
#15056=CARTESIAN_POINT('Ctrl Pts',(-3.44610757298242,-2.46453580233588,
4.97772421886392));
#15057=CARTESIAN_POINT('Ctrl Pts',(-3.42478073659837,-2.41367971150249,
4.98142881521618));
#15058=CARTESIAN_POINT('Ctrl Pts',(-3.43115657648041,-2.35120632071406,
4.98513341156845));
#15059=CARTESIAN_POINT('Ctrl Pts',(-3.46231715328677,-2.30570693229799,
4.98883800792072));
#15060=CARTESIAN_POINT('Ctrl Pts',(-3.49347773009313,-2.26020754388192,
4.99254260427299));
#15061=CARTESIAN_POINT('Ctrl Pts',(-3.54942304382382,-2.2316821578382,4.99624720062526));
#15062=CARTESIAN_POINT('Ctrl Pts',(-3.60454940455119,-2.2331855772681,4.99995179697753));
#15063=CARTESIAN_POINT('Ctrl Pts',(-3.65967576527857,-2.23468899669801,
5.00365639332979));
#15064=CARTESIAN_POINT('Ctrl Pts',(-3.71398317300263,-2.26622122160152,
5.00736098968206));
#15065=CARTESIAN_POINT('Ctrl Pts',(-3.74261753436876,-2.31335135359861,
5.01106558603433));
#15066=CARTESIAN_POINT('Ctrl Pts',(-3.75828879455967,-2.33914513862194,
5.01309306946923));
#15067=CARTESIAN_POINT('Ctrl Pts',(-3.76627033973982,-2.36961088421597,
5.01512055290412));
#15068=CARTESIAN_POINT('Ctrl Pts',(-3.76634000649331,-2.40004261214866,
5.01714803633902));
#15069=CARTESIAN_POINT('Origin',(-3.6,-2.4,4.7));
#15070=CARTESIAN_POINT('',(-3.76673281282141,-2.40013003219325,5.08714803633902));
#15071=CARTESIAN_POINT('',(-3.7668206250807,-2.39991359866148,5.06785196366098));
#15072=CARTESIAN_POINT('',(-3.7666,-2.4,4.7));
#15073=CARTESIAN_POINT('Ctrl Pts',(-3.7668206250807,-2.39991359866148,5.06785196366098));
#15074=CARTESIAN_POINT('Ctrl Pts',(-3.76685198944486,-2.39494457920613,
5.06751845741382));
#15075=CARTESIAN_POINT('Ctrl Pts',(-3.7666492146414,-2.38997815520014,5.06718495116665));
#15076=CARTESIAN_POINT('Ctrl Pts',(-3.7662039619217,-2.38503356610626,5.06685144491949));
#15077=CARTESIAN_POINT('Ctrl Pts',(-3.76125808275068,-2.33010893762799,
5.06314684856722));
#15078=CARTESIAN_POINT('Ctrl Pts',(-3.72639327521678,-2.27787848097877,
5.05944225221495));
#15079=CARTESIAN_POINT('Ctrl Pts',(-3.67756563230702,-2.25224574125102,
5.05573765586268));
#15080=CARTESIAN_POINT('Ctrl Pts',(-3.62873798939725,-2.22661300152326,
5.05203305951042));
#15081=CARTESIAN_POINT('Ctrl Pts',(-3.56594751111163,-2.22757797871697,
5.04832846315815));
#15082=CARTESIAN_POINT('Ctrl Pts',(-3.51793060783244,-2.25469905531577,
5.04462386680588));
#15083=CARTESIAN_POINT('Ctrl Pts',(-3.46991370455325,-2.28182013191457,
5.04091927045361));
#15084=CARTESIAN_POINT('Ctrl Pts',(-3.43667037628051,-2.33509730791846,
5.03721467410135));
#15085=CARTESIAN_POINT('Ctrl Pts',(-3.43341462472151,-2.39014797674899,
5.03351007774908));
#15086=CARTESIAN_POINT('Ctrl Pts',(-3.43015887316251,-2.44519864557951,
5.02980548139681));
#15087=CARTESIAN_POINT('Ctrl Pts',(-3.45689069831725,-2.50202280723666,
5.02610088504454));
#15088=CARTESIAN_POINT('Ctrl Pts',(-3.50137612681596,-2.53461456435925,
5.02239628869227));
#15089=CARTESIAN_POINT('Ctrl Pts',(-3.54586155531466,-2.56720632148184,
5.01869169234));
#15090=CARTESIAN_POINT('Ctrl Pts',(-3.60810058715733,-2.57556567406988,
5.01498709598774));
#15091=CARTESIAN_POINT('Ctrl Pts',(-3.65960917750461,-2.5558669157941,5.01128249963547));
#15092=CARTESIAN_POINT('Ctrl Pts',(-3.71111776785188,-2.53616815751832,
5.0075779032832));
#15093=CARTESIAN_POINT('Ctrl Pts',(-3.75189591670377,-2.48841128837874,
5.00387330693093));
#15094=CARTESIAN_POINT('Ctrl Pts',(-3.7632812725096,-2.4344525109445,5.00016871057867));
#15095=CARTESIAN_POINT('Ctrl Pts',(-3.76565462941201,-2.42320442708544,
4.9993964616061));
#15096=CARTESIAN_POINT('Ctrl Pts',(-3.7667507426838,-2.41168684356181,4.99862421263354));
#15097=CARTESIAN_POINT('Ctrl Pts',(-3.76664426409402,-2.40014916296054,
4.99785196366098));
#15098=CARTESIAN_POINT('Ctrl Pts',(-3.76634000649331,-2.40004261214866,
5.01714803633902));
#15099=CARTESIAN_POINT('Ctrl Pts',(-3.76639763409716,-2.42521541658955,
5.01882514925639));
#15100=CARTESIAN_POINT('Ctrl Pts',(-3.76104161906272,-2.45036494470439,
5.02050226217376));
#15101=CARTESIAN_POINT('Ctrl Pts',(-3.75014621732021,-2.47282762178721,
5.02217937509113));
#15102=CARTESIAN_POINT('Ctrl Pts',(-3.72607922389733,-2.52244571888807,
5.0258839714434));
#15103=CARTESIAN_POINT('Ctrl Pts',(-3.67498392204337,-2.55895387399913,
5.02958856779567));
#15104=CARTESIAN_POINT('Ctrl Pts',(-3.62024436531629,-2.56564393553624,
5.03329316414794));
#15105=CARTESIAN_POINT('Ctrl Pts',(-3.5655048085892,-2.57233399707334,5.03699776050021));
#15106=CARTESIAN_POINT('Ctrl Pts',(-3.50712099698899,-2.54920596503651,
5.04070235685248));
#15107=CARTESIAN_POINT('Ctrl Pts',(-3.47181261508692,-2.50684448916664,
5.04440695320474));
#15108=CARTESIAN_POINT('Ctrl Pts',(-3.43650423318484,-2.46448301329678,
5.04811154955701));
#15109=CARTESIAN_POINT('Ctrl Pts',(-3.42427128098091,-2.4028880935939,5.05181614590928));
#15110=CARTESIAN_POINT('Ctrl Pts',(-3.44071223414431,-2.35024904491843,
5.05552074226155));
#15111=CARTESIAN_POINT('Ctrl Pts',(-3.45715318730771,-2.29760999624296,
5.05922533861381));
#15112=CARTESIAN_POINT('Ctrl Pts',(-3.50226804583846,-2.2539268185949,5.06292993496608));
#15113=CARTESIAN_POINT('Ctrl Pts',(-3.55540974746646,-2.23919126462175,
5.06663453131835));
#15114=CARTESIAN_POINT('Ctrl Pts',(-3.60855144909447,-2.2244557106486,5.07033912767062));
#15115=CARTESIAN_POINT('Ctrl Pts',(-3.66971999381974,-2.23866778035036,
5.07404372402289));
#15116=CARTESIAN_POINT('Ctrl Pts',(-3.71092123316877,-2.27532344228896,
5.07774832037516));
#15117=CARTESIAN_POINT('Ctrl Pts',(-3.74576802981578,-2.30632572323287,
5.08088155902978));
#15118=CARTESIAN_POINT('Ctrl Pts',(-3.76633165591099,-2.35338253179949,
5.0840147976844));
#15119=CARTESIAN_POINT('Ctrl Pts',(-3.76673281282141,-2.40013003219325,
5.08714803633902));
#15120=CARTESIAN_POINT('Origin',(-3.6,-2.4,4.7));
#15121=CARTESIAN_POINT('',(-3.76674783764939,-2.3998784327954,5.15714803633902));
#15122=CARTESIAN_POINT('',(-3.76638442554721,-2.39990578503699,5.13785196366098));
#15123=CARTESIAN_POINT('',(-3.7666,-2.4,4.7));
#15124=CARTESIAN_POINT('',(-3.47309291201476,-2.29206413469515,5.2));
#15125=CARTESIAN_POINT('Ctrl Pts',(-3.76674783764939,-2.3998784327954,5.15714803633902));
#15126=CARTESIAN_POINT('Ctrl Pts',(-3.7663543041176,-2.44715561431286,5.16031823516921));
#15127=CARTESIAN_POINT('Ctrl Pts',(-3.74524548348422,-2.49473161213543,
5.1634884339994));
#15128=CARTESIAN_POINT('Ctrl Pts',(-3.70967617757414,-2.52575977295725,
5.16665863282959));
#15129=CARTESIAN_POINT('Ctrl Pts',(-3.66811098624533,-2.56201832251683,
5.17036322918186));
#15130=CARTESIAN_POINT('Ctrl Pts',(-3.60679922558629,-2.57567991185357,
5.17406782553412));
#15131=CARTESIAN_POINT('Ctrl Pts',(-3.55380862744679,-2.56038491971217,
5.17777242188639));
#15132=CARTESIAN_POINT('Ctrl Pts',(-3.5008180293073,-2.54508992757078,5.18147701823866));
#15133=CARTESIAN_POINT('Ctrl Pts',(-3.45614859368735,-2.50083835395125,
5.18518161459093));
#15134=CARTESIAN_POINT('Ctrl Pts',(-3.44024450358536,-2.44813181223257,
5.1888862109432));
#15135=CARTESIAN_POINT('Ctrl Pts',(-3.42434041348337,-2.39542527051388,
5.19259080729547));
#15136=CARTESIAN_POINT('Ctrl Pts',(-3.43720166889934,-2.33426376069605,
5.19629540364773));
#15137=CARTESIAN_POINT('Ctrl Pts',(-3.47309291201476,-2.29206413469515,
5.2));
#15138=CARTESIAN_POINT('',(-3.7271475418302,-2.29187968016137,5.2));
#15139=CARTESIAN_POINT('Origin',(-3.6,-2.4,5.2));
#15140=CARTESIAN_POINT('Ctrl Pts',(-3.72714769448933,-2.29187956305504,
5.2));
#15141=CARTESIAN_POINT('Ctrl Pts',(-3.69206190113039,-2.25072743961435,
5.19636770818144));
#15142=CARTESIAN_POINT('Ctrl Pts',(-3.6350641341643,-2.22812240899828,5.19273541636289));
#15143=CARTESIAN_POINT('Ctrl Pts',(-3.58132375070445,-2.23418207790235,
5.18910312454434));
#15144=CARTESIAN_POINT('Ctrl Pts',(-3.52651360920706,-2.24036237079714,
5.18539852819207));
#15145=CARTESIAN_POINT('Ctrl Pts',(-3.47509182514536,-2.27635992272048,
5.1816939318398));
#15146=CARTESIAN_POINT('Ctrl Pts',(-3.45055836147391,-2.3257410419838,5.17798933548753));
#15147=CARTESIAN_POINT('Ctrl Pts',(-3.42602489780247,-2.37512216124712,
5.17428473913526));
#15148=CARTESIAN_POINT('Ctrl Pts',(-3.42837975452128,-2.43788684785041,
5.170580142783));
#15149=CARTESIAN_POINT('Ctrl Pts',(-3.45656193213921,-2.48529019920904,
5.16687554643073));
#15150=CARTESIAN_POINT('Ctrl Pts',(-3.48474410975714,-2.53269355056767,
5.16317095007846));
#15151=CARTESIAN_POINT('Ctrl Pts',(-3.53875360827419,-2.56473556668165,
5.15946635372619));
#15152=CARTESIAN_POINT('Ctrl Pts',(-3.59386432904901,-2.56676216280164,
5.15576175737392));
#15153=CARTESIAN_POINT('Ctrl Pts',(-3.64897504982384,-2.56878875892163,
5.15205716102165));
#15154=CARTESIAN_POINT('Ctrl Pts',(-3.70518699285644,-2.54079993504764,
5.14835256466939));
#15155=CARTESIAN_POINT('Ctrl Pts',(-3.73677861120293,-2.49559987891255,
5.14464796831712));
#15156=CARTESIAN_POINT('Ctrl Pts',(-3.75609666594378,-2.46796035917884,
5.14238263343174));
#15157=CARTESIAN_POINT('Ctrl Pts',(-3.76620859684834,-2.43388515114326,
5.14011729854636));
#15158=CARTESIAN_POINT('Ctrl Pts',(-3.76638442554721,-2.39990578503699,
5.13785196366098));
#15159=CARTESIAN_POINT('Origin',(-3.6,-2.4,5.35459252805377));
#15160=CARTESIAN_POINT('',(-3.8057227013582,-2.39988044337606,4.34540747194623));
#15161=CARTESIAN_POINT('',(-3.80516111137892,-2.40008013262119,4.33959252805377));
#15162=CARTESIAN_POINT('',(-3.805475,-2.39999999999999,5.35459252805377));
#15163=CARTESIAN_POINT('',(-3.41173724903364,-2.48232321801035,4.3));
#15164=CARTESIAN_POINT('Ctrl Pts',(-3.80516111137892,-2.40008013262119,
4.33959252805377));
#15165=CARTESIAN_POINT('Ctrl Pts',(-3.80504330063484,-2.36152007992449,
4.33750880775931));
#15166=CARTESIAN_POINT('Ctrl Pts',(-3.77605833105766,-2.25423615375421,
4.33172049111259));
#15167=CARTESIAN_POINT('Ctrl Pts',(-3.60297473301061,-2.15700944143379,
4.32222757811361));
#15168=CARTESIAN_POINT('Ctrl Pts',(-3.39749761512046,-2.26611614077921,
4.3111137890568));
#15169=CARTESIAN_POINT('Ctrl Pts',(-3.38436282049399,-2.419721374356,4.30370459635227));
#15170=CARTESIAN_POINT('Ctrl Pts',(-3.41173724903364,-2.48232321801035,
4.3));
#15171=CARTESIAN_POINT('',(-3.47764162637991,-2.56553534042572,4.3));
#15172=CARTESIAN_POINT('Origin',(-3.6,-2.4,4.3));
#15173=CARTESIAN_POINT('Ctrl Pts',(-3.8057227013582,-2.39988044337606,4.34540747194623));
#15174=CARTESIAN_POINT('Ctrl Pts',(-3.8057729696998,-2.39271640638513,4.34501772883951));
#15175=CARTESIAN_POINT('Ctrl Pts',(-3.80218373546239,-2.3175070024762,4.34092338938053));
#15176=CARTESIAN_POINT('Ctrl Pts',(-3.70962995644976,-2.18326697275372,
4.33312445356927));
#15177=CARTESIAN_POINT('Ctrl Pts',(-3.47734459894833,-2.19039236572141,
4.32201066451247));
#15178=CARTESIAN_POINT('Ctrl Pts',(-3.35820162590419,-2.3879909133699,4.31096917998938));
#15179=CARTESIAN_POINT('Ctrl Pts',(-3.42405718781536,-2.52582031335719,
4.30363229181855));
#15180=CARTESIAN_POINT('Ctrl Pts',(-3.47764149510761,-2.56553553810743,
4.3));
#15181=CARTESIAN_POINT('Origin',(-3.6,-2.4,5.35459252805377));
#15182=CARTESIAN_POINT('',(-3.80519266468163,-2.39989734570579,4.41540747194623));
#15183=CARTESIAN_POINT('',(-3.80566724789774,-2.40014978098439,4.40959252805377));
#15184=CARTESIAN_POINT('',(-3.805475,-2.39999999999999,5.35459252805377));
#15185=CARTESIAN_POINT('Ctrl Pts',(-3.80566724789774,-2.40014978098439,
4.40959252805377));
#15186=CARTESIAN_POINT('Ctrl Pts',(-3.80518614471975,-2.34148051217519,
4.40640305253959));
#15187=CARTESIAN_POINT('Ctrl Pts',(-3.74813829229662,-2.21384966330463,
4.39950898067315));
#15188=CARTESIAN_POINT('Ctrl Pts',(-3.53156901893564,-2.16697244735031,
4.38891031245443));
#15189=CARTESIAN_POINT('Ctrl Pts',(-3.36710794136624,-2.33111753922242,
4.37779652339762));
#15190=CARTESIAN_POINT('Ctrl Pts',(-3.41581894666805,-2.55829572590735,
4.36668273434083));
#15191=CARTESIAN_POINT('Ctrl Pts',(-3.63310626972243,-2.64061568298545,
4.35556894528402));
#15192=CARTESIAN_POINT('Ctrl Pts',(-3.7850442261316,-2.5285041432322,4.34653887652167));
#15193=CARTESIAN_POINT('Ctrl Pts',(-3.80525275353212,-2.43007507309885,
4.34121340411158));
#15194=CARTESIAN_POINT('Ctrl Pts',(-3.80516111137892,-2.40008013262119,
4.33959252805377));
#15195=CARTESIAN_POINT('Ctrl Pts',(-3.80519266468163,-2.39989734570579,
4.41540747194623));
#15196=CARTESIAN_POINT('Ctrl Pts',(-3.80531782889597,-2.37222562131849,
4.41391197361979));
#15197=CARTESIAN_POINT('Ctrl Pts',(-3.78721617857279,-2.2761634023784,4.40871187894108));
#15198=CARTESIAN_POINT('Ctrl Pts',(-3.64121277969171,-2.16065653443092,
4.3998071879101));
#15199=CARTESIAN_POINT('Ctrl Pts',(-3.42126523797479,-2.23556891230323,
4.38869339885329));
#15200=CARTESIAN_POINT('Ctrl Pts',(-3.36491711226222,-2.46098554747977,
4.37757960979649));
#15201=CARTESIAN_POINT('Ctrl Pts',(-3.52374009350676,-2.63058418685777,
4.36646582073969));
#15202=CARTESIAN_POINT('Ctrl Pts',(-3.74435278297668,-2.59057501347053,
4.3557417747896));
#15203=CARTESIAN_POINT('Ctrl Pts',(-3.80529515774691,-2.46081219780934,
4.34872232519178));
#15204=CARTESIAN_POINT('Ctrl Pts',(-3.8057227013582,-2.39988044337606,4.34540747194623));
#15205=CARTESIAN_POINT('Origin',(-3.6,-2.4,5.35459252805377));
#15206=CARTESIAN_POINT('',(-3.80534991328218,-2.40017652766129,4.48540747194623));
#15207=CARTESIAN_POINT('',(-3.80562878759967,-2.39983660975823,4.47959252805377));
#15208=CARTESIAN_POINT('',(-3.805475,-2.39999999999999,5.35459252805377));
#15209=CARTESIAN_POINT('Ctrl Pts',(-3.80562878759967,-2.39983660975823,
4.47959252805377));
#15210=CARTESIAN_POINT('Ctrl Pts',(-3.80572325938657,-2.3889667780224,4.47900189367213));
#15211=CARTESIAN_POINT('Ctrl Pts',(-3.79999615684062,-2.31001856287219,
4.47470666293823));
#15212=CARTESIAN_POINT('Ctrl Pts',(-3.69773850858379,-2.17766949547173,
4.46670683585206));
#15213=CARTESIAN_POINT('Ctrl Pts',(-3.46621554409366,-2.19730464027232,
4.45559304679525));
#15214=CARTESIAN_POINT('Ctrl Pts',(-3.35714698343348,-2.40246926898597,
4.44447925773846));
#15215=CARTESIAN_POINT('Ctrl Pts',(-3.47036459479899,-2.60537350263611,
4.43336546868164));
#15216=CARTESIAN_POINT('Ctrl Pts',(-3.70223885894321,-2.62029753112878,
4.42225167962485));
#15217=CARTESIAN_POINT('Ctrl Pts',(-3.80084480548257,-2.48716469502641,
4.41432736608222));
#15218=CARTESIAN_POINT('Ctrl Pts',(-3.80574494915964,-2.40962524577001,
4.41010764889186));
#15219=CARTESIAN_POINT('Ctrl Pts',(-3.80566724789774,-2.40014978098439,
4.40959252805377));
#15220=CARTESIAN_POINT('Ctrl Pts',(-3.80534991328218,-2.40017652766129,
4.48540747194623));
#15221=CARTESIAN_POINT('Ctrl Pts',(-3.8049563333145,-2.35213729171836,4.48280621840006));
#15222=CARTESIAN_POINT('Ctrl Pts',(-3.76418777806192,-2.23508077339291,
4.47650036850163));
#15223=CARTESIAN_POINT('Ctrl Pts',(-3.56918135654791,-2.15909775573836,
4.46648992225092));
#15224=CARTESIAN_POINT('Ctrl Pts',(-3.38089013692747,-2.29524052189659,
4.45537613319412));
#15225=CARTESIAN_POINT('Ctrl Pts',(-3.39315268252002,-2.52727080497827,
4.44426234413731));
#15226=CARTESIAN_POINT('Ctrl Pts',(-3.59474487821944,-2.64280871984201,
4.43314855508051));
#15227=CARTESIAN_POINT('Ctrl Pts',(-3.77337323688511,-2.5504598261374,4.42353026435015));
#15228=CARTESIAN_POINT('Ctrl Pts',(-3.80500777646484,-2.44077305290937,
4.41761656997206));
#15229=CARTESIAN_POINT('Ctrl Pts',(-3.80519266468163,-2.39989734570579,
4.41540747194623));
#15230=CARTESIAN_POINT('Origin',(-3.6,-2.4,5.35459252805377));
#15231=CARTESIAN_POINT('',(-3.80581595477291,-2.39999917227814,4.55540747194623));
#15232=CARTESIAN_POINT('',(-3.80515176250663,-2.39995310238523,4.54959252805377));
#15233=CARTESIAN_POINT('',(-3.805475,-2.39999999999999,5.35459252805377));
#15234=CARTESIAN_POINT('Ctrl Pts',(-3.80515176250663,-2.39995310238523,
4.54959252805377));
#15235=CARTESIAN_POINT('Ctrl Pts',(-3.80521587176166,-2.36854855820361,
4.54789613845241));
#15236=CARTESIAN_POINT('Ctrl Pts',(-3.78367651299531,-2.26864576859469,
4.54249515249878));
#15237=CARTESIAN_POINT('Ctrl Pts',(-3.62821111895818,-2.15877850380716,
4.53338957019289));
#15238=CARTESIAN_POINT('Ctrl Pts',(-3.4126363777684,-2.24547313898512,4.52227578113608));
#15239=CARTESIAN_POINT('Ctrl Pts',(-3.3685576844537,-2.47360796440317,4.51116199207928));
#15240=CARTESIAN_POINT('Ctrl Pts',(-3.53632076809686,-2.63436858142862,
4.50004820302248));
#15241=CARTESIAN_POINT('Ctrl Pts',(-3.75035693907624,-2.58346600089298,
4.4895250483473));
#15242=CARTESIAN_POINT('Ctrl Pts',(-3.80513071034435,-2.45714489336835,
4.4827064900244));
#15243=CARTESIAN_POINT('Ctrl Pts',(-3.80562878759967,-2.39983660975823,
4.47959252805377));
#15244=CARTESIAN_POINT('Ctrl Pts',(-3.80581595309039,-2.39999917228222,
4.55540747194623));
#15245=CARTESIAN_POINT('Ctrl Pts',(-3.80581595573579,-2.39995488126346,
4.55540505953261));
#15246=CARTESIAN_POINT('Ctrl Pts',(-3.805795885724,-2.33189557869137,4.55169805076671));
#15247=CARTESIAN_POINT('Ctrl Pts',(-3.73158417960078,-2.19586944742698,
4.54428644564855));
#15248=CARTESIAN_POINT('Ctrl Pts',(-3.49986236155564,-2.17873967321655,
4.53317265659175));
#15249=CARTESIAN_POINT('Ctrl Pts',(-3.35979765944108,-2.36413198553984,
4.52205886753494));
#15250=CARTESIAN_POINT('Ctrl Pts',(-3.43959288407154,-2.58235469793693,
4.51094507847814));
#15251=CARTESIAN_POINT('Ctrl Pts',(-3.66621056034765,-2.6336660879353,4.49983128942134));
#15252=CARTESIAN_POINT('Ctrl Pts',(-3.79336822690886,-2.50914983096546,
4.4913187539107));
#15253=CARTESIAN_POINT('Ctrl Pts',(-3.80551685342017,-2.42055275952314,
4.48651081475233));
#15254=CARTESIAN_POINT('Ctrl Pts',(-3.80534991328218,-2.40017652766129,
4.48540747194623));
#15255=CARTESIAN_POINT('Origin',(-3.6,-2.4,5.35459252805377));
#15256=CARTESIAN_POINT('',(-3.80534749847032,-2.39982399268994,4.62540747194623));
#15257=CARTESIAN_POINT('',(-3.80545680064795,-2.40018789159516,4.61959252805377));
#15258=CARTESIAN_POINT('',(-3.805475,-2.39999999999999,5.35459252805377));
#15259=CARTESIAN_POINT('Ctrl Pts',(-3.80545680064795,-2.40018789159516,
4.61959252805377));
#15260=CARTESIAN_POINT('Ctrl Pts',(-3.80498629881388,-2.34850704133116,
4.61679038323269));
#15261=CARTESIAN_POINT('Ctrl Pts',(-3.75902064354221,-2.22775548399901,
4.61028364205933));
#15262=CARTESIAN_POINT('Ctrl Pts',(-3.55620097341096,-2.16111650777606,
4.60007230453371));
#15263=CARTESIAN_POINT('Ctrl Pts',(-3.37554637252617,-2.307240921179,4.58895851547691));
#15264=CARTESIAN_POINT('Ctrl Pts',(-3.40033672233922,-2.53826877141577,
4.57784472642011));
#15265=CARTESIAN_POINT('Ctrl Pts',(-3.60788113454322,-2.64273764704216,
4.5667309373633));
#15266=CARTESIAN_POINT('Ctrl Pts',(-3.7776337191139,-2.54299330423865,4.55731353790786));
#15267=CARTESIAN_POINT('Ctrl Pts',(-3.80507586918669,-2.43713018575349,
4.55160073480468));
#15268=CARTESIAN_POINT('Ctrl Pts',(-3.80515176250663,-2.39995310238523,
4.54959252805377));
#15269=CARTESIAN_POINT('Ctrl Pts',(-3.80534749847032,-2.39982399268994,
4.62540747194623));
#15270=CARTESIAN_POINT('Ctrl Pts',(-3.8055145307928,-2.37935804813576,4.62429930431288));
#15271=CARTESIAN_POINT('Ctrl Pts',(-3.79329841632202,-2.29066951260838,
4.61948654032727));
#15272=CARTESIAN_POINT('Ctrl Pts',(-3.66590691978443,-2.16624808716256,
4.61096917998938));
#15273=CARTESIAN_POINT('Ctrl Pts',(-3.4393560992794,-2.21785386089149,4.59985539093257));
#15274=CARTESIAN_POINT('Ctrl Pts',(-3.35984446292695,-2.43618006142673,
4.58874160187577));
#15275=CARTESIAN_POINT('Ctrl Pts',(-3.50014991321196,-2.62139024142312,
4.57762781281897));
#15276=CARTESIAN_POINT('Ctrl Pts',(-3.73179898649779,-2.60396320633826,
4.56651643617578));
#15277=CARTESIAN_POINT('Ctrl Pts',(-3.80581189336919,-2.46796989528688,
4.55910965588487));
#15278=CARTESIAN_POINT('Ctrl Pts',(-3.80581595309039,-2.39999917228222,
4.55540747194623));
#15279=CARTESIAN_POINT('Origin',(-3.6,-2.4,5.35459252805377));
#15280=CARTESIAN_POINT('',(-3.80519404433776,-2.40010391087563,4.69540747194623));
#15281=CARTESIAN_POINT('',(-3.80578860319875,-2.39993212258736,4.68959252805377));
#15282=CARTESIAN_POINT('',(-3.805475,-2.39999999999999,5.35459252805377));
#15283=CARTESIAN_POINT('Ctrl Pts',(-3.80578860319875,-2.39993212258736,
4.68959252805377));
#15284=CARTESIAN_POINT('Ctrl Pts',(-3.80580467529652,-2.39619821380325,
4.68938922436523));
#15285=CARTESIAN_POINT('Ctrl Pts',(-3.8040203847709,-2.32444075317719,4.68548132432442));
#15286=CARTESIAN_POINT('Ctrl Pts',(-3.72035445765201,-2.18905336667194,
4.67786882793134));
#15287=CARTESIAN_POINT('Ctrl Pts',(-3.4880454122232,-2.18447773232253,4.66675503887454));
#15288=CARTESIAN_POINT('Ctrl Pts',(-3.35820967063793,-2.37717207376684,
4.65564124981773));
#15289=CARTESIAN_POINT('Ctrl Pts',(-3.4496873596065,-2.5907610749791,4.64452746076093));
#15290=CARTESIAN_POINT('Ctrl Pts',(-3.67874791298872,-2.62974430088435,
4.63341367170412));
#15291=CARTESIAN_POINT('Ctrl Pts',(-3.79614945789441,-2.50163131370898,
4.62510202746841));
#15292=CARTESIAN_POINT('Ctrl Pts',(-3.80560832925468,-2.41683209288794,
4.62049497958495));
#15293=CARTESIAN_POINT('Ctrl Pts',(-3.80545680064795,-2.40018789159516,
4.61959252805377));
#15294=CARTESIAN_POINT('Ctrl Pts',(-3.80519404433776,-2.40010391087563,
4.69540747194623));
#15295=CARTESIAN_POINT('Ctrl Pts',(-3.80500644622954,-2.35913959443751,
4.69319354909316));
#15296=CARTESIAN_POINT('Ctrl Pts',(-3.77326723416865,-2.24936122008858,
4.68727502988781));
#15297=CARTESIAN_POINT('Ctrl Pts',(-3.59442944460758,-2.15719833661306,
4.6776519143302));
#15298=CARTESIAN_POINT('Ctrl Pts',(-3.3929874908777,-2.27299803191391,4.6665381252734));
#15299=CARTESIAN_POINT('Ctrl Pts',(-3.38102643442896,-2.50504406890429,
4.65542433621659));
#15300=CARTESIAN_POINT('Ctrl Pts',(-3.5694943658766,-2.64094207834572,4.64431054715979));
#15301=CARTESIAN_POINT('Ctrl Pts',(-3.76430796656755,-2.56474251573525,
4.63430492573634));
#15302=CARTESIAN_POINT('Ctrl Pts',(-3.8049561429515,-2.44777555218424,4.62800390066515));
#15303=CARTESIAN_POINT('Ctrl Pts',(-3.80534749847032,-2.39982399268994,
4.62540747194623));
#15304=CARTESIAN_POINT('Origin',(-3.6,-2.4,5.35459252805377));
#15305=CARTESIAN_POINT('',(-3.80572671416466,-2.40012021867279,4.76540747194623));
#15306=CARTESIAN_POINT('',(-3.80525640542964,-2.39985490132803,4.75959252805377));
#15307=CARTESIAN_POINT('',(-3.805475,-2.39999999999999,5.35459252805377));
#15308=CARTESIAN_POINT('Ctrl Pts',(-3.80525640542964,-2.39985490132803,
4.75959252805377));
#15309=CARTESIAN_POINT('Ctrl Pts',(-3.80541421756911,-2.37565177743561,
4.7582834691455));
#15310=CARTESIAN_POINT('Ctrl Pts',(-3.7902631541036,-2.2831457592228,4.75326981388497));
#15311=CARTESIAN_POINT('Ctrl Pts',(-3.65317166084996,-2.16302647390142,
4.74455156227217));
#15312=CARTESIAN_POINT('Ctrl Pts',(-3.42974254509416,-2.22680624538361,
4.73343777321536));
#15313=CARTESIAN_POINT('Ctrl Pts',(-3.36215200866455,-2.44911222461694,
4.72232398415856));
#15314=CARTESIAN_POINT('Ctrl Pts',(-3.51226643608395,-2.62646522768789,
4.71121019510176));
#15315=CARTESIAN_POINT('Ctrl Pts',(-3.73846937161942,-2.59707960507412,
4.70029970973349));
#15316=CARTESIAN_POINT('Ctrl Pts',(-3.80551180980452,-2.46423743611441,
4.6930938207175));
#15317=CARTESIAN_POINT('Ctrl Pts',(-3.80578860319875,-2.39993212258736,
4.68959252805377));
#15318=CARTESIAN_POINT('Ctrl Pts',(-3.80572671416466,-2.40012021867279,
4.76540747194623));
#15319=CARTESIAN_POINT('Ctrl Pts',(-3.80530257178557,-2.33910193112031,
4.76208779387343));
#15320=CARTESIAN_POINT('Ctrl Pts',(-3.74420123427486,-2.20925254264417,
4.75506351944836));
#15321=CARTESIAN_POINT('Ctrl Pts',(-3.52344221265408,-2.16951662960737,
4.74433464867103));
#15322=CARTESIAN_POINT('Ctrl Pts',(-3.36483725976158,-2.33931915924769,
4.73322085961422));
#15323=CARTESIAN_POINT('Ctrl Pts',(-3.42147942993616,-2.56466355059616,
4.72210707055742));
#15324=CARTESIAN_POINT('Ctrl Pts',(-3.64152350245114,-2.63928952667227,
4.71099328150061));
#15325=CARTESIAN_POINT('Ctrl Pts',(-3.78729792557216,-2.52365598332802,
4.70209341529689));
#15326=CARTESIAN_POINT('Ctrl Pts',(-3.80532035746924,-2.42768591123397,
4.69689814544542));
#15327=CARTESIAN_POINT('Ctrl Pts',(-3.80519404433776,-2.40010391087563,
4.69540747194623));
#15328=CARTESIAN_POINT('Origin',(-3.6,-2.4,5.35459252805377));
#15329=CARTESIAN_POINT('',(-3.80555826192291,-2.39982008596012,4.83540747194623));
#15330=CARTESIAN_POINT('',(-3.80526423797111,-2.40014879660671,4.82959252805377));
#15331=CARTESIAN_POINT('',(-3.805475,-2.39999999999999,5.35459252805377));
#15332=CARTESIAN_POINT('Ctrl Pts',(-3.80526423797112,-2.40014879660671,
4.82959252805377));
#15333=CARTESIAN_POINT('Ctrl Pts',(-3.80496497000794,-2.35550570352956,
4.82717771392578));
#15334=CARTESIAN_POINT('Ctrl Pts',(-3.7687007786119,-2.24193241424781,4.82105830344552));
#15335=CARTESIAN_POINT('Ctrl Pts',(-3.58130943002562,-2.15785471265546,
4.81123429661298));
#15336=CARTESIAN_POINT('Ctrl Pts',(-3.38642338383962,-2.28437687679961,
4.8001205075562));
#15337=CARTESIAN_POINT('Ctrl Pts',(-3.38702643654876,-2.51673019686447,
4.78900671849938));
#15338=CARTESIAN_POINT('Ctrl Pts',(-3.58256660716932,-2.64223904392882,
4.77789292944258));
#15339=CARTESIAN_POINT('Ctrl Pts',(-3.76915216315368,-2.5573566497576,4.76808819929404));
#15340=CARTESIAN_POINT('Ctrl Pts',(-3.80496761407973,-2.44414587187183,
4.76198806549777));
#15341=CARTESIAN_POINT('Ctrl Pts',(-3.80525640542964,-2.39985490132803,
4.75959252805377));
#15342=CARTESIAN_POINT('Ctrl Pts',(-3.80555826192291,-2.39982008596012,
4.83540747194623));
#15343=CARTESIAN_POINT('Ctrl Pts',(-3.80567994930423,-2.38654227868304,
4.83468663500597));
#15344=CARTESIAN_POINT('Ctrl Pts',(-3.79845786380229,-2.30515766788849,
4.83026120171345));
#15345=CARTESIAN_POINT('Ctrl Pts',(-3.68988494304833,-2.17438001896094,
4.82213117206866));
#15346=CARTESIAN_POINT('Ctrl Pts',(-3.45919253805822,-2.20211888040452,
4.81101738301185));
#15347=CARTESIAN_POINT('Ctrl Pts',(-3.35738279984868,-2.41098057473832,
4.79990359395505));
#15348=CARTESIAN_POINT('Ctrl Pts',(-3.47764333640382,-2.60979162448597,
4.78878980489824));
#15349=CARTESIAN_POINT('Ctrl Pts',(-3.7098983147675,-2.61657802114276,4.77767601584144));
#15350=CARTESIAN_POINT('Ctrl Pts',(-3.80223426786157,-2.48231400602396,
4.76988190485744));
#15351=CARTESIAN_POINT('Ctrl Pts',(-3.80577589367883,-2.40719531865107,
4.7657923902257));
#15352=CARTESIAN_POINT('Ctrl Pts',(-3.80572671416466,-2.40012021867279,
4.76540747194623));
#15353=CARTESIAN_POINT('Origin',(-3.6,-2.4,5.35459252805377));
#15354=CARTESIAN_POINT('',(-3.80514217248594,-2.39999218980904,4.90540747194623));
#15355=CARTESIAN_POINT('',(-3.80579332868662,-2.40006173798069,4.89959252805377));
#15356=CARTESIAN_POINT('',(-3.805475,-2.39999999999999,5.35459252805377));
#15357=CARTESIAN_POINT('Ctrl Pts',(-3.80579332868662,-2.40006173798069,
4.89959252805377));
#15358=CARTESIAN_POINT('Ctrl Pts',(-3.80553739175956,-2.33540634391997,
4.89607195870605));
#15359=CARTESIAN_POINT('Ctrl Pts',(-3.73784442753819,-2.20225412798971,
4.88884679300607));
#15360=CARTESIAN_POINT('Ctrl Pts',(-3.511092084609,-2.17399322981363,4.87791703095382));
#15361=CARTESIAN_POINT('Ctrl Pts',(-3.36190028176488,-2.35212305601353,
4.86680324189701));
#15362=CARTESIAN_POINT('Ctrl Pts',(-3.43064385125587,-2.57407519200526,
4.85568945284021));
#15363=CARTESIAN_POINT('Ctrl Pts',(-3.6544010243217,-2.63669433060785,4.84457566378341));
#15364=CARTESIAN_POINT('Ctrl Pts',(-3.79056542018395,-2.51613221267343,
4.83587668885459));
#15365=CARTESIAN_POINT('Ctrl Pts',(-3.80542408070796,-2.42399322720708,
4.83088231027805));
#15366=CARTESIAN_POINT('Ctrl Pts',(-3.80526423797112,-2.40014879660671,
4.82959252805377));
#15367=CARTESIAN_POINT('Ctrl Pts',(-3.80514217248594,-2.39999218980904,
4.90540747194623));
#15368=CARTESIAN_POINT('Ctrl Pts',(-3.80515363847659,-2.36617331522009,
4.90358087978625));
#15369=CARTESIAN_POINT('Ctrl Pts',(-3.78123591841218,-2.26378007899297,
4.898049691274));
#15370=CARTESIAN_POINT('Ctrl Pts',(-3.61973808033182,-2.15793784472475,
4.88881390640949));
#15371=CARTESIAN_POINT('Ctrl Pts',(-3.4073347883606,-2.25213588990288,4.87770011735268));
#15372=CARTESIAN_POINT('Ctrl Pts',(-3.37128014957741,-2.48167563194308,
4.86658632829587));
#15373=CARTESIAN_POINT('Ctrl Pts',(-3.54457538374435,-2.63645674180255,
4.85547253923907));
#15374=CARTESIAN_POINT('Ctrl Pts',(-3.75407113935919,-2.57880494205606,
4.84507958712253));
#15375=CARTESIAN_POINT('Ctrl Pts',(-3.8050545615032,-2.45478089640322,4.83839123135824));
#15376=CARTESIAN_POINT('Ctrl Pts',(-3.80555826192291,-2.39982008596012,
4.83540747194623));
#15377=CARTESIAN_POINT('Origin',(-3.6,-2.4,5.35459252805377));
#15378=CARTESIAN_POINT('',(-3.80552959282545,-2.40018396914357,4.97540747194623));
#15379=CARTESIAN_POINT('',(-3.80544614170703,-2.39981229694107,4.96959252805377));
#15380=CARTESIAN_POINT('',(-3.805475,-2.39999999999999,5.35459252805377));
#15381=CARTESIAN_POINT('Ctrl Pts',(-3.80544614170703,-2.39981229694107,
4.96959252805377));
#15382=CARTESIAN_POINT('Ctrl Pts',(-3.80560005255251,-2.38281031937819,
4.9686707998386));
#15383=CARTESIAN_POINT('Ctrl Pts',(-3.79589308932397,-2.29764759199308,
4.96404447527115));
#15384=CARTESIAN_POINT('Ctrl Pts',(-3.67755429765177,-2.16985003043886,
4.95571355435145));
#15385=CARTESIAN_POINT('Ctrl Pts',(-3.44869918397279,-2.21002173633656,
4.94459976529464));
#15386=CARTESIAN_POINT('Ctrl Pts',(-3.3583314230664,-2.42408270152555,4.93348597623784));
#15387=CARTESIAN_POINT('Ctrl Pts',(-3.48916565133794,-2.61610049686178,
4.92237218718103));
#15388=CARTESIAN_POINT('Ctrl Pts',(-3.7214478158856,-2.61031905668909,4.91125839812423));
#15389=CARTESIAN_POINT('Ctrl Pts',(-3.80419976839027,-2.4748431306509,4.90366517841514));
#15390=CARTESIAN_POINT('Ctrl Pts',(-3.8058067070074,-2.4034414011323,4.89977655505832));
#15391=CARTESIAN_POINT('Ctrl Pts',(-3.80579332868662,-2.40006173798069,
4.89959252805377));
#15392=CARTESIAN_POINT('Ctrl Pts',(-3.80552959282545,-2.40018396914357,
4.97540747194623));
#15393=CARTESIAN_POINT('Ctrl Pts',(-3.80503093302249,-2.34615078230832,
4.97247512456653));
#15394=CARTESIAN_POINT('Ctrl Pts',(-3.75549941719541,-2.22304560401132,
4.96583818083455));
#15395=CARTESIAN_POINT('Ctrl Pts',(-3.54785414492032,-2.16279863265717,
4.9554966407503));
#15396=CARTESIAN_POINT('Ctrl Pts',(-3.37243276525931,-2.31516585290104,
4.94438285169351));
#15397=CARTESIAN_POINT('Ctrl Pts',(-3.40530625649813,-2.54518272988275,
4.9332690626367));
#15398=CARTESIAN_POINT('Ctrl Pts',(-3.61638513906469,-2.64231220781178,
4.9221552735799));
#15399=CARTESIAN_POINT('Ctrl Pts',(-3.78023982132068,-2.53813917250258,
4.91286807668307));
#15400=CARTESIAN_POINT('Ctrl Pts',(-3.80513038376869,-2.43476294468685,
4.90728547613852));
#15401=CARTESIAN_POINT('Ctrl Pts',(-3.80514217248594,-2.39999218980904,
4.90540747194623));
#15402=CARTESIAN_POINT('Origin',(-3.6,-2.4,5.35459252805377));
#15403=CARTESIAN_POINT('',(-3.80574710647333,-2.39989343748479,5.04540747194623));
#15404=CARTESIAN_POINT('',(-3.80515433874078,-2.40005255540964,5.03959252805377));
#15405=CARTESIAN_POINT('',(-3.805475,-2.39999999999999,5.35459252805377));
#15406=CARTESIAN_POINT('Ctrl Pts',(-3.80515433874078,-2.40005255540964,
5.03959252805377));
#15407=CARTESIAN_POINT('Ctrl Pts',(-3.80506841571452,-2.36251978652027,
5.03756504461887));
#15408=CARTESIAN_POINT('Ctrl Pts',(-3.77723760351786,-2.25628892207963,
5.0318329648317));
#15409=CARTESIAN_POINT('Ctrl Pts',(-3.60662102802227,-2.15722471599323,
5.02239628869228));
#15410=CARTESIAN_POINT('Ctrl Pts',(-3.39962168818772,-2.262769500459,5.01128249963546));
#15411=CARTESIAN_POINT('Ctrl Pts',(-3.37603088927244,-2.49392292132789,
5.00016871057867));
#15412=CARTESIAN_POINT('Ctrl Pts',(-3.55744155755193,-2.63910762521254,
4.98905492152185));
#15413=CARTESIAN_POINT('Ctrl Pts',(-3.75953036700652,-2.57154453779223,
4.97886286068023));
#15414=CARTESIAN_POINT('Ctrl Pts',(-3.80498145636834,-2.45114441507362,
4.97237539619086));
#15415=CARTESIAN_POINT('Ctrl Pts',(-3.80544614170703,-2.39981229694107,
4.96959252805377));
#15416=CARTESIAN_POINT('Ctrl Pts',(-3.80574710647333,-2.39989343748479,
5.04540747194623));
#15417=CARTESIAN_POINT('Ctrl Pts',(-3.80578578950289,-2.39376493044645,
5.04507396569907));
#15418=CARTESIAN_POINT('Ctrl Pts',(-3.80275768152815,-2.31959956136467,
5.04103586309964));
#15419=CARTESIAN_POINT('Ctrl Pts',(-3.71288602579316,-2.18496415245566,
5.03329316414794));
#15420=CARTESIAN_POINT('Ctrl Pts',(-3.4805593716682,-2.1885345970333,5.02217937509112));
#15421=CARTESIAN_POINT('Ctrl Pts',(-3.35755805936012,-2.38566174720256,
5.01106558603434));
#15422=CARTESIAN_POINT('Ctrl Pts',(-3.45646661470834,-2.59591285074103,
4.99995179697752));
#15423=CARTESIAN_POINT('Ctrl Pts',(-3.68675290044432,-2.62684270619768,
4.98883800792072));
#15424=CARTESIAN_POINT('Ctrl Pts',(-3.79782383930996,-2.49676322878239,
4.98065656624362));
#15425=CARTESIAN_POINT('Ctrl Pts',(-3.80566091748472,-2.41441389064144,
4.9761797209188));
#15426=CARTESIAN_POINT('Ctrl Pts',(-3.80552959282545,-2.40018396914357,
4.97540747194623));
#15427=CARTESIAN_POINT('Origin',(-3.6,-2.4,5.35459252805377));
#15428=CARTESIAN_POINT('',(-3.80520912268496,-2.39988380060309,5.11540747194623));
#15429=CARTESIAN_POINT('',(-3.8056388038084,-2.40016037433918,5.10959252805377));
#15430=CARTESIAN_POINT('',(-3.805475,-2.39999999999999,5.35459252805377));
#15431=CARTESIAN_POINT('Ctrl Pts',(-3.8056388038084,-2.40016037433918,5.10959252805377));
#15432=CARTESIAN_POINT('Ctrl Pts',(-3.80514403960571,-2.34250465619148,
5.10645928939915));
#15433=CARTESIAN_POINT('Ctrl Pts',(-3.74979516025411,-2.21584695448232,
5.09962145439226));
#15434=CARTESIAN_POINT('Ctrl Pts',(-3.53510505567384,-2.16596525884485,
5.0890790230331));
#15435=CARTESIAN_POINT('Ctrl Pts',(-3.36817872512274,-2.32759432716241,
5.07796523397629));
#15436=CARTESIAN_POINT('Ctrl Pts',(-3.41344101541272,-2.5554973786501,5.06685144491949));
#15437=CARTESIAN_POINT('Ctrl Pts',(-3.62946287054873,-2.64107179130501,
5.05573765586269));
#15438=CARTESIAN_POINT('Ctrl Pts',(-3.78402795903722,-2.53063333570257,
5.04665135024078));
#15439=CARTESIAN_POINT('Ctrl Pts',(-3.80522541336203,-2.43109926604885,
5.04126964097114));
#15440=CARTESIAN_POINT('Ctrl Pts',(-3.80515433874078,-2.40005255540964,
5.03959252805377));
#15441=CARTESIAN_POINT('Ctrl Pts',(-3.80520912268496,-2.39988380060309,
5.11540747194623));
#15442=CARTESIAN_POINT('Ctrl Pts',(-3.80534690105405,-2.37325776244818,
5.11396821047934));
#15443=CARTESIAN_POINT('Ctrl Pts',(-3.78816006360229,-2.27826799235566,
5.10882435266019));
#15444=CARTESIAN_POINT('Ctrl Pts',(-3.64483147519039,-2.16130911215383,
5.09997589848876));
#15445=CARTESIAN_POINT('Ctrl Pts',(-3.42377645640768,-2.23288040078699,
5.08886210943196));
#15446=CARTESIAN_POINT('Ctrl Pts',(-3.36401956629289,-2.45741970591997,
5.07774832037515));
#15447=CARTESIAN_POINT('Ctrl Pts',(-3.52025888222192,-2.62940132794335,
5.06663453131835));
#15448=CARTESIAN_POINT('Ctrl Pts',(-3.74260711073009,-2.59254976529191,
5.05585424850871));
#15449=CARTESIAN_POINT('Ctrl Pts',(-3.8053560973714,-2.46184055125472,5.04877856205134));
#15450=CARTESIAN_POINT('Ctrl Pts',(-3.80574710647333,-2.39989343748479,
5.04540747194623));
#15451=CARTESIAN_POINT('Origin',(-3.6,-2.4,5.35459252805377));
#15452=CARTESIAN_POINT('',(-3.80526708169851,-2.40022955265959,5.18540747194623));
#15453=CARTESIAN_POINT('',(-3.80565733457988,-2.39985006589819,5.17959252805377));
#15454=CARTESIAN_POINT('',(-3.805475,-2.39999999999999,5.35459252805377));
#15455=CARTESIAN_POINT('',(-3.65301702171886,-2.59851743256717,5.2));
#15456=CARTESIAN_POINT('Ctrl Pts',(-3.65301702171886,-2.59851743256717,
5.2));
#15457=CARTESIAN_POINT('Ctrl Pts',(-3.71902879097456,-2.58088801151799,
5.19629540364773));
#15458=CARTESIAN_POINT('Ctrl Pts',(-3.79249438127854,-2.51127182149751,
5.19143122762981));
#15459=CARTESIAN_POINT('Ctrl Pts',(-3.80542872863858,-2.42165306802236,
5.18656705161189));
#15460=CARTESIAN_POINT('Ctrl Pts',(-3.80526708169851,-2.40022955265959,
5.18540747194623));
#15461=CARTESIAN_POINT('',(-3.54686845990025,-2.59887322544328,5.2));
#15462=CARTESIAN_POINT('Origin',(-3.6,-2.4,5.2));
#15463=CARTESIAN_POINT('Ctrl Pts',(-3.54686838721289,-2.59887345127292,
5.2));
#15464=CARTESIAN_POINT('Ctrl Pts',(-3.61132827149734,-2.61600531405712,
5.19636770818144));
#15465=CARTESIAN_POINT('Ctrl Pts',(-3.74930830903252,-2.58406706978518,
5.18956521753271));
#15466=CARTESIAN_POINT('Ctrl Pts',(-3.80517197262043,-2.45815906273072,
5.18276272688396));
#15467=CARTESIAN_POINT('Ctrl Pts',(-3.80565733457988,-2.39985006589818,
5.17959252805377));
#15468=CARTESIAN_POINT('Origin',(3.6,-2.4,4.7));
#15469=CARTESIAN_POINT('',(3.4332441194689,-2.40012144310043,4.38714803633902));
#15470=CARTESIAN_POINT('',(3.43319918361158,-2.39990306414324,4.36785196366098));
#15471=CARTESIAN_POINT('',(3.4334,-2.4,4.7));
#15472=CARTESIAN_POINT('',(3.43648706727485,-2.43192304546281,4.3));
#15473=CARTESIAN_POINT('Ctrl Pts',(3.43319918361158,-2.39990306414324,4.36785196366098));
#15474=CARTESIAN_POINT('Ctrl Pts',(3.43315842575224,-2.39409443322767,4.36746222055426));
#15475=CARTESIAN_POINT('Ctrl Pts',(3.43343544638748,-2.38828969410672,4.36707247744754));
#15476=CARTESIAN_POINT('Ctrl Pts',(3.43404308035483,-2.38251974365232,4.36668273434082));
#15477=CARTESIAN_POINT('Ctrl Pts',(3.43981877860357,-2.32767505996788,4.36297813798856));
#15478=CARTESIAN_POINT('Ctrl Pts',(3.47546516768456,-2.27597350876472,4.35927354163629));
#15479=CARTESIAN_POINT('Ctrl Pts',(3.52467802663468,-2.2510856178596,4.35556894528402));
#15480=CARTESIAN_POINT('Ctrl Pts',(3.57389088558479,-2.22619772695447,4.35186434893175));
#15481=CARTESIAN_POINT('Ctrl Pts',(3.63667021440403,-2.22812349634739,4.34815975257949));
#15482=CARTESIAN_POINT('Ctrl Pts',(3.68426556377096,-2.25596352517201,4.34445515622722));
#15483=CARTESIAN_POINT('Ctrl Pts',(3.73186091313788,-2.28380355399663,4.34075055987495));
#15484=CARTESIAN_POINT('Ctrl Pts',(3.7642722830525,-2.33755784225296,4.33704596352268));
#15485=CARTESIAN_POINT('Ctrl Pts',(3.76670489686818,-2.39266164590465,4.33334136717041));
#15486=CARTESIAN_POINT('Ctrl Pts',(3.76913751068386,-2.44776544955635,4.32963677081814));
#15487=CARTESIAN_POINT('Ctrl Pts',(3.74159136840061,-2.50421876860342,4.32593217446587));
#15488=CARTESIAN_POINT('Ctrl Pts',(3.69659414024548,-2.53611221831126,4.32222757811361));
#15489=CARTESIAN_POINT('Ctrl Pts',(3.65159691209034,-2.56800566801911,4.31852298176134));
#15490=CARTESIAN_POINT('Ctrl Pts',(3.58914859806332,-2.57533924838774,4.31481838540907));
#15491=CARTESIAN_POINT('Ctrl Pts',(3.53802492988379,-2.55491157781525,4.3111137890568));
#15492=CARTESIAN_POINT('Ctrl Pts',(3.48690126170426,-2.53448390724277,4.30740919270454));
#15493=CARTESIAN_POINT('Ctrl Pts',(3.44710223937223,-2.48629498572918,4.30370459635227));
#15494=CARTESIAN_POINT('Ctrl Pts',(3.43648706727485,-2.43192304546281,4.3));
#15495=CARTESIAN_POINT('',(3.59474332937116,-2.23318013131002,4.3));
#15496=CARTESIAN_POINT('Origin',(3.6,-2.4,4.3));
#15497=CARTESIAN_POINT('',(3.43365449489478,-2.40006497081539,4.31714803633902));
#15498=CARTESIAN_POINT('Ctrl Pts',(3.5947433329992,-2.23317993884958,4.3));
#15499=CARTESIAN_POINT('Ctrl Pts',(3.54069367702075,-2.23495318942066,4.30363229181855));
#15500=CARTESIAN_POINT('Ctrl Pts',(3.48748281579126,-2.26542182682866,4.30726458363711));
#15501=CARTESIAN_POINT('Ctrl Pts',(3.45871387185408,-2.31121589220503,4.31089687545567));
#15502=CARTESIAN_POINT('Ctrl Pts',(3.44221012289161,-2.33748636499654,4.31298059575012));
#15503=CARTESIAN_POINT('Ctrl Pts',(3.43375001435867,-2.36880031414598,4.31506431604457));
#15504=CARTESIAN_POINT('Ctrl Pts',(3.43365449489478,-2.40006497081539,4.31714803633902));
#15505=CARTESIAN_POINT('',(3.4334,-2.4,4.2));
#15506=CARTESIAN_POINT('',(3.4334,-2.4,4.7));
#15507=CARTESIAN_POINT('Origin',(3.6,-2.4,4.2));
#15508=CARTESIAN_POINT('Ctrl Pts',(3.43365449489478,-2.40006497081539,4.31714803633902));
#15509=CARTESIAN_POINT('Ctrl Pts',(3.43358019259399,-2.42438499763772,4.31876891239684));
#15510=CARTESIAN_POINT('Ctrl Pts',(3.43856722876717,-2.44867519801865,4.32038978845465));
#15511=CARTESIAN_POINT('Ctrl Pts',(3.44876666940262,-2.4705384776482,4.32201066451247));
#15512=CARTESIAN_POINT('Ctrl Pts',(3.47207802031749,-2.52050813792769,4.32571526086474));
#15513=CARTESIAN_POINT('Ctrl Pts',(3.52261765592676,-2.55780017703868,4.329419857217));
#15514=CARTESIAN_POINT('Ctrl Pts',(3.57725038923478,-2.56532196913419,4.33312445356927));
#15515=CARTESIAN_POINT('Ctrl Pts',(3.6318831225428,-2.57284376122971,4.33682904992154));
#15516=CARTESIAN_POINT('Ctrl Pts',(3.69060895354956,-2.55059530630975,4.34053364627381));
#15517=CARTESIAN_POINT('Ctrl Pts',(3.72655438362155,-2.50877157126828,4.34423824262608));
#15518=CARTESIAN_POINT('Ctrl Pts',(3.76249981369354,-2.4669478362268,4.34794283897835));
#15519=CARTESIAN_POINT('Ctrl Pts',(3.77566484283074,-2.40554882106382,4.35164743533061));
#15520=CARTESIAN_POINT('Ctrl Pts',(3.76002306731497,-2.35266772394791,4.35535203168288));
#15521=CARTESIAN_POINT('Ctrl Pts',(3.74438129179919,-2.29978662683201,4.35905662803515));
#15522=CARTESIAN_POINT('Ctrl Pts',(3.69993271163044,-2.25542344776319,4.36276122438742));
#15523=CARTESIAN_POINT('Ctrl Pts',(3.64702014743753,-2.23988444780227,4.36646582073969));
#15524=CARTESIAN_POINT('Ctrl Pts',(3.59410758324462,-2.22434544784136,4.37017041709196));
#15525=CARTESIAN_POINT('Ctrl Pts',(3.53273103502755,-2.23763062698835,4.37387501344422));
#15526=CARTESIAN_POINT('Ctrl Pts',(3.49097949059372,-2.27365834937589,4.37757960979649));
#15527=CARTESIAN_POINT('Ctrl Pts',(3.45503346139427,-2.30467644890953,4.38076908531067));
#15528=CARTESIAN_POINT('Ctrl Pts',(3.43363419992272,-2.35255214998637,4.38395856082484));
#15529=CARTESIAN_POINT('Ctrl Pts',(3.4332441194689,-2.40012144310043,4.38714803633902));
#15530=CARTESIAN_POINT('Origin',(3.6,-2.4,4.7));
#15531=CARTESIAN_POINT('',(3.4332753032246,-2.39986752249821,4.45714803633902));
#15532=CARTESIAN_POINT('',(3.43362893615635,-2.39991676750829,4.43785196366098));
#15533=CARTESIAN_POINT('',(3.4334,-2.4,4.7));
#15534=CARTESIAN_POINT('Ctrl Pts',(3.43362893615635,-2.39991676750829,4.43785196366098));
#15535=CARTESIAN_POINT('Ctrl Pts',(3.43352745251214,-2.37748041857078,4.43635646533454));
#15536=CARTESIAN_POINT('Ctrl Pts',(3.43774838897563,-2.35508066415019,4.43486096700809));
#15537=CARTESIAN_POINT('Ctrl Pts',(3.44647311482898,-2.33459946287839,4.43336546868165));
#15538=CARTESIAN_POINT('Ctrl Pts',(3.46808570175023,-2.28386414463698,4.42966087232938));
#15539=CARTESIAN_POINT('Ctrl Pts',(3.51733510423541,-2.24490173470295,4.42595627597711));
#15540=CARTESIAN_POINT('Ctrl Pts',(3.57168220229163,-2.23554374099052,4.42225167962485));
#15541=CARTESIAN_POINT('Ctrl Pts',(3.62602930034785,-2.22618574727809,4.41854708327258));
#15542=CARTESIAN_POINT('Ctrl Pts',(3.68547409397512,-2.24643216978725,4.41484248692031));
#15543=CARTESIAN_POINT('Ctrl Pts',(3.72281103935986,-2.2870168380163,4.41113789056804));
#15544=CARTESIAN_POINT('Ctrl Pts',(3.7601479847446,-2.32760150624535,4.40743329421577));
#15545=CARTESIAN_POINT('Ctrl Pts',(3.77537708188681,-2.38852442019428,4.4037286978635));
#15546=CARTESIAN_POINT('Ctrl Pts',(3.76152924259544,-2.44190442427593,4.40002410151124));
#15547=CARTESIAN_POINT('Ctrl Pts',(3.74768140330407,-2.49528442835759,4.39631950515897));
#15548=CARTESIAN_POINT('Ctrl Pts',(3.70475662757912,-2.54112152257198,4.3926149088067));
#15549=CARTESIAN_POINT('Ctrl Pts',(3.65239849228647,-2.55843697682615,4.38891031245443));
#15550=CARTESIAN_POINT('Ctrl Pts',(3.60004035699382,-2.57575243108032,4.38520571610217));
#15551=CARTESIAN_POINT('Ctrl Pts',(3.53824886213347,-2.56454624537428,4.3815011197499));
#15552=CARTESIAN_POINT('Ctrl Pts',(3.49530561841154,-2.52994924443839,4.37779652339763));
#15553=CARTESIAN_POINT('Ctrl Pts',(3.45688023078761,-2.49899203076829,4.37448167015208));
#15554=CARTESIAN_POINT('Ctrl Pts',(3.43354583842081,-2.4493067834413,4.37116681690653));
#15555=CARTESIAN_POINT('Ctrl Pts',(3.43319918361158,-2.39990306414324,4.36785196366098));
#15556=CARTESIAN_POINT('Ctrl Pts',(3.4332441194689,-2.40012144310043,4.38714803633902));
#15557=CARTESIAN_POINT('Ctrl Pts',(3.4331811189632,-2.40780419031934,4.38766315717711));
#15558=CARTESIAN_POINT('Ctrl Pts',(3.43366612887655,-2.41547894509172,4.3881782780152));
#15559=CARTESIAN_POINT('Ctrl Pts',(3.43472637398198,-2.42307339909524,4.3886933988533));
#15560=CARTESIAN_POINT('Ctrl Pts',(3.44235134245467,-2.47769046079897,4.39239799520556));
#15561=CARTESIAN_POINT('Ctrl Pts',(3.47972782005064,-2.52815431857834,4.39610259155783));
#15562=CARTESIAN_POINT('Ctrl Pts',(3.5297501656918,-2.5513695031952,4.3998071879101));
#15563=CARTESIAN_POINT('Ctrl Pts',(3.57977251133296,-2.57458468781207,4.40351178426237));
#15564=CARTESIAN_POINT('Ctrl Pts',(3.64244072501932,-2.57055119926642,4.40721638061463));
#15565=CARTESIAN_POINT('Ctrl Pts',(3.68907438543537,-2.54111518550135,4.4109209769669));
#15566=CARTESIAN_POINT('Ctrl Pts',(3.73570804585142,-2.51167917173628,4.41462557331917));
#15567=CARTESIAN_POINT('Ctrl Pts',(3.76630715299715,-2.4568406327518,4.41833016967144));
#15568=CARTESIAN_POINT('Ctrl Pts',(3.76686783098938,-2.40169663747488,4.42203476602371));
#15569=CARTESIAN_POINT('Ctrl Pts',(3.7674285089816,-2.34655264219797,4.42573936237597));
#15570=CARTESIAN_POINT('Ctrl Pts',(3.73795075782031,-2.29110319062863,4.42944395872824));
#15571=CARTESIAN_POINT('Ctrl Pts',(3.69192524795617,-2.26072508833266,4.43314855508051));
#15572=CARTESIAN_POINT('Ctrl Pts',(3.64589973809204,-2.23034698603669,4.43685315143278));
#15573=CARTESIAN_POINT('Ctrl Pts',(3.58332646952505,-2.2250402330141,4.44055774778505));
#15574=CARTESIAN_POINT('Ctrl Pts',(3.53284244819528,-2.24723347009038,4.44426234413732));
#15575=CARTESIAN_POINT('Ctrl Pts',(3.48235842686551,-2.26942670716666,4.44796694048958));
#15576=CARTESIAN_POINT('Ctrl Pts',(3.44396365277294,-2.31911993434182,4.45167153684185));
#15577=CARTESIAN_POINT('Ctrl Pts',(3.43522971460805,-2.37357077679719,4.45537613319412));
#15578=CARTESIAN_POINT('Ctrl Pts',(3.43383723789082,-2.38225203019296,4.45596676757575));
#15579=CARTESIAN_POINT('Ctrl Pts',(3.4331987050974,-2.39105421663124,4.45655740195739));
#15580=CARTESIAN_POINT('Ctrl Pts',(3.4332753032246,-2.39986752249821,4.45714803633902));
#15581=CARTESIAN_POINT('Origin',(3.6,-2.4,4.7));
#15582=CARTESIAN_POINT('',(3.43366207720083,-2.39996197521424,4.52714803633902));
#15583=CARTESIAN_POINT('',(3.43350143827108,-2.40014312936039,4.50785196366098));
#15584=CARTESIAN_POINT('',(3.4334,-2.4,4.7));
#15585=CARTESIAN_POINT('Ctrl Pts',(3.43350143827108,-2.40014312936039,4.50785196366098));
#15586=CARTESIAN_POINT('Ctrl Pts',(3.43382055454292,-2.36119271753362,4.50525071011481));
#15587=CARTESIAN_POINT('Ctrl Pts',(3.44745634567654,-2.3220410177822,4.50264945656865));
#15588=CARTESIAN_POINT('Ctrl Pts',(3.4724157519356,-2.29243605104842,4.50004820302248));
#15589=CARTESIAN_POINT('Ctrl Pts',(3.50796189295608,-2.25027389736965,4.49634360667021));
#15590=CARTESIAN_POINT('Ctrl Pts',(3.56647488846456,-2.22747467908062,4.49263901031794));
#15591=CARTESIAN_POINT('Ctrl Pts',(3.62117593657879,-2.23447258988711,4.48893441396567));
#15592=CARTESIAN_POINT('Ctrl Pts',(3.67587698469302,-2.2414705006936,4.4852298176134));
#15593=CARTESIAN_POINT('Ctrl Pts',(3.726766085413,-2.27826554059562,4.48152522126114));
#15594=CARTESIAN_POINT('Ctrl Pts',(3.75055354862185,-2.32801824658462,4.47782062490887));
#15595=CARTESIAN_POINT('Ctrl Pts',(3.7743410118307,-2.37777095257363,4.4741160285566));
#15596=CARTESIAN_POINT('Ctrl Pts',(3.77102683752841,-2.44048132464963,4.47041143220433));
#15597=CARTESIAN_POINT('Ctrl Pts',(3.74212778560952,-2.48744961415947,4.46670683585206));
#15598=CARTESIAN_POINT('Ctrl Pts',(3.71322873369063,-2.53441790366931,4.4630022394998));
#15599=CARTESIAN_POINT('Ctrl Pts',(3.65874480415513,-2.56564411061299,4.45929764314753));
#15600=CARTESIAN_POINT('Ctrl Pts',(3.60361085781629,-2.56683736686161,4.45559304679526));
#15601=CARTESIAN_POINT('Ctrl Pts',(3.54847691147744,-2.56803062311024,4.45188845044299));
#15602=CARTESIAN_POINT('Ctrl Pts',(3.49269294833524,-2.5391909286638,4.44818385409072));
#15603=CARTESIAN_POINT('Ctrl Pts',(3.46178885244281,-2.49351696816619,4.44447925773846));
#15604=CARTESIAN_POINT('Ctrl Pts',(3.44336034614035,-2.46628100333426,4.44227015971263));
#15605=CARTESIAN_POINT('Ctrl Pts',(3.43377884425998,-2.43305896049386,4.4400610616868));
#15606=CARTESIAN_POINT('Ctrl Pts',(3.43362893615635,-2.39991676750829,4.43785196366098));
#15607=CARTESIAN_POINT('Ctrl Pts',(3.4332753032246,-2.39986752249821,4.45714803633902));
#15608=CARTESIAN_POINT('Ctrl Pts',(3.43367914638464,-2.44633332293026,4.46026199830965));
#15609=CARTESIAN_POINT('Ctrl Pts',(3.45396108248041,-2.49310820388228,4.46337596028029));
#15610=CARTESIAN_POINT('Ctrl Pts',(3.48843309316639,-2.52409905740531,4.46648992225092));
#15611=CARTESIAN_POINT('Ctrl Pts',(3.52944351212684,-2.56096803782247,4.47019451860319));
#15612=CARTESIAN_POINT('Ctrl Pts',(3.59053745228497,-2.57549754092119,4.47389911495546));
#15613=CARTESIAN_POINT('Ctrl Pts',(3.64375492615303,-2.56103806030718,4.47760371130773));
#15614=CARTESIAN_POINT('Ctrl Pts',(3.69697240002109,-2.54657857969317,4.48130830766));
#15615=CARTESIAN_POINT('Ctrl Pts',(3.74231340759908,-2.50313011536643,4.48501290401227));
#15616=CARTESIAN_POINT('Ctrl Pts',(3.75902737934242,-2.45057710185421,4.48871750036453));
#15617=CARTESIAN_POINT('Ctrl Pts',(3.77574135108577,-2.39802408834199,4.4924220967168));
#15618=CARTESIAN_POINT('Ctrl Pts',(3.76382828699448,-2.33636652564429,4.49612669306907));
#15619=CARTESIAN_POINT('Ctrl Pts',(3.72874026856414,-2.29382234772163,4.49983128942134));
#15620=CARTESIAN_POINT('Ctrl Pts',(3.6936522501338,-2.25127816979896,4.5035358857736));
#15621=CARTESIAN_POINT('Ctrl Pts',(3.63538927736442,-2.22784737665133,4.50724048212587));
#15622=CARTESIAN_POINT('Ctrl Pts',(3.58061573003626,-2.23425320323999,4.51094507847814));
#15623=CARTESIAN_POINT('Ctrl Pts',(3.52584218270809,-2.24065902982864,4.51464967483041));
#15624=CARTESIAN_POINT('Ctrl Pts',(3.47455806082114,-2.27690147615359,4.51835427118267));
#15625=CARTESIAN_POINT('Ctrl Pts',(3.45023383359826,-2.32639398133752,4.52205886753494));
#15626=CARTESIAN_POINT('Ctrl Pts',(3.43909540927391,-2.34905733333477,4.5237552571363));
#15627=CARTESIAN_POINT('Ctrl Pts',(3.4336100971438,-2.37449903703717,4.52545164673766));
#15628=CARTESIAN_POINT('Ctrl Pts',(3.43366207720083,-2.39996197521424,4.52714803633902));
#15629=CARTESIAN_POINT('Origin',(3.6,-2.4,4.7));
#15630=CARTESIAN_POINT('',(3.43341475097665,-2.4001523433056,4.59714803633902));
#15631=CARTESIAN_POINT('',(3.43312356989615,-2.39999932887968,4.57785196366098));
#15632=CARTESIAN_POINT('',(3.4334,-2.4,4.7));
#15633=CARTESIAN_POINT('Ctrl Pts',(3.4331235712606,-2.39999932888299,4.57785196366098));
#15634=CARTESIAN_POINT('Ctrl Pts',(3.43312027533203,-2.34481656196242,4.57414495489509));
#15635=CARTESIAN_POINT('Ctrl Pts',(3.46320503039949,-2.28963688420389,4.57043794612919));
#15636=CARTESIAN_POINT('Ctrl Pts',(3.50958660961886,-2.25973894891049,4.5667309373633));
#15637=CARTESIAN_POINT('Ctrl Pts',(3.55593800505376,-2.22986047032491,4.56302634101103));
#15638=CARTESIAN_POINT('Ctrl Pts',(3.61856500889817,-2.22523083965654,4.55932174465877));
#15639=CARTESIAN_POINT('Ctrl Pts',(3.66880601775922,-2.24796883366633,4.5556171483065));
#15640=CARTESIAN_POINT('Ctrl Pts',(3.71904702662027,-2.27070682767613,4.55191255195423));
#15641=CARTESIAN_POINT('Ctrl Pts',(3.75690204049796,-2.32081244636408,4.54820795560196));
#15642=CARTESIAN_POINT('Ctrl Pts',(3.765046497567,-2.37535456915184,4.54450335924969));
#15643=CARTESIAN_POINT('Ctrl Pts',(3.77319095463605,-2.4298966919396,4.54079876289742));
#15644=CARTESIAN_POINT('Ctrl Pts',(3.75162485489646,-2.48887531882715,4.53709416654515));
#15645=CARTESIAN_POINT('Ctrl Pts',(3.71021804632554,-2.52529854692327,4.53338957019289));
#15646=CARTESIAN_POINT('Ctrl Pts',(3.66881123775463,-2.56172177501939,4.52968497384062));
#15647=CARTESIAN_POINT('Ctrl Pts',(3.60756372035239,-2.57558960432407,4.52598037748835));
#15648=CARTESIAN_POINT('Ctrl Pts',(3.55450576746795,-2.56055534384899,4.52227578113609));
#15649=CARTESIAN_POINT('Ctrl Pts',(3.5014478145835,-2.5455210833739,4.51857118478382));
#15650=CARTESIAN_POINT('Ctrl Pts',(3.45657942621685,-2.50158473311904,4.51486658843155));
#15651=CARTESIAN_POINT('Ctrl Pts',(3.44043487529976,-2.44885401345736,4.51116199207928));
#15652=CARTESIAN_POINT('Ctrl Pts',(3.43562653117309,-2.43314918230523,4.51005864927318));
#15653=CARTESIAN_POINT('Ctrl Pts',(3.43336608251409,-2.41666426269897,4.50895530646708));
#15654=CARTESIAN_POINT('Ctrl Pts',(3.43350143827108,-2.40014312936039,4.50785196366098));
#15655=CARTESIAN_POINT('Ctrl Pts',(3.43366207720083,-2.39996197521424,4.52714803633902));
#15656=CARTESIAN_POINT('Ctrl Pts',(3.43372361182786,-2.43010531274957,4.52915624308993));
#15657=CARTESIAN_POINT('Ctrl Pts',(3.4415451707818,-2.46027840851952,4.53116444984084));
#15658=CARTESIAN_POINT('Ctrl Pts',(3.45693460775185,-2.48590718316162,4.53317265659175));
#15659=CARTESIAN_POINT('Ctrl Pts',(3.48532394168714,-2.53318531575888,4.53687725294402));
#15660=CARTESIAN_POINT('Ctrl Pts',(3.53946694211655,-2.5649990169105,4.54058184929628));
#15661=CARTESIAN_POINT('Ctrl Pts',(3.59458475789197,-2.56678856593634,4.54428644564855));
#15662=CARTESIAN_POINT('Ctrl Pts',(3.64970257366739,-2.56857811496219,4.54799104200082));
#15663=CARTESIAN_POINT('Ctrl Pts',(3.70579520478882,-2.54034351186226,4.55169563835309));
#15664=CARTESIAN_POINT('Ctrl Pts',(3.73719154055164,-2.49500648282243,4.55540023470536));
#15665=CARTESIAN_POINT('Ctrl Pts',(3.76858787631446,-2.4496694537826,4.55910483105763));
#15666=CARTESIAN_POINT('Ctrl Pts',(3.77528791671867,-2.38722999880286,4.56280942740989));
#15667=CARTESIAN_POINT('Ctrl Pts',(3.75422535028399,-2.33626388852243,4.56651402376216));
#15668=CARTESIAN_POINT('Ctrl Pts',(3.73316278384931,-2.28529777824199,4.57021862011443));
#15669=CARTESIAN_POINT('Ctrl Pts',(3.68433761057573,-2.24580501266085,4.5739232164667));
#15670=CARTESIAN_POINT('Ctrl Pts',(3.63009494786823,-2.23585967988047,4.57762781281896));
#15671=CARTESIAN_POINT('Ctrl Pts',(3.57585228516072,-2.22591434710008,4.58133240917123));
#15672=CARTESIAN_POINT('Ctrl Pts',(3.51619213301928,-2.24551644712046,4.5850370055235));
#15673=CARTESIAN_POINT('Ctrl Pts',(3.47841829836813,-2.28569496771878,4.58874160187577));
#15674=CARTESIAN_POINT('Ctrl Pts',(3.4498462907659,-2.31608587207317,4.59154374669685));
#15675=CARTESIAN_POINT('Ctrl Pts',(3.43379623586762,-2.35824928979842,4.59434589151794));
#15676=CARTESIAN_POINT('Ctrl Pts',(3.43341475097665,-2.4001523433056,4.59714803633902));
#15677=CARTESIAN_POINT('Origin',(3.6,-2.4,4.7));
#15678=CARTESIAN_POINT('',(3.43314572405529,-2.39994496470472,4.66714803633902));
#15679=CARTESIAN_POINT('',(3.43350339621029,-2.39985729254273,4.64785196366098));
#15680=CARTESIAN_POINT('',(3.4334,-2.4,4.7));
#15681=CARTESIAN_POINT('Ctrl Pts',(3.43350339621029,-2.39985729254273,4.64785196366098));
#15682=CARTESIAN_POINT('Ctrl Pts',(3.43336796571017,-2.38326341978069,4.64674379602763));
#15683=CARTESIAN_POINT('Ctrl Pts',(3.43564862259693,-2.36670593582693,4.64563562839428));
#15684=CARTESIAN_POINT('Ctrl Pts',(3.44049848254047,-2.3509387164529,4.64452746076093));
#15685=CARTESIAN_POINT('Ctrl Pts',(3.45671152911857,-2.29822901656582,4.64082286440866));
#15686=CARTESIAN_POINT('Ctrl Pts',(3.50163696254783,-2.25435099787568,4.6371182680564));
#15687=CARTESIAN_POINT('Ctrl Pts',(3.55471440347455,-2.23938568444105,4.63341367170413));
#15688=CARTESIAN_POINT('Ctrl Pts',(3.60779184440126,-2.22442037100641,4.62970907535186));
#15689=CARTESIAN_POINT('Ctrl Pts',(3.66902129282543,-2.23836776282728,4.62600447899959));
#15690=CARTESIAN_POINT('Ctrl Pts',(3.71038074448169,-2.27484475695027,4.62229988264732));
#15691=CARTESIAN_POINT('Ctrl Pts',(3.75174019613796,-2.31132175107326,4.61859528629505));
#15692=CARTESIAN_POINT('Ctrl Pts',(3.77322965102632,-2.37032834749837,4.61489068994278));
#15693=CARTESIAN_POINT('Ctrl Pts',(3.76501433826252,-2.42485984278043,4.61118609359052));
#15694=CARTESIAN_POINT('Ctrl Pts',(3.75679902549871,-2.47939133806249,4.60748149723825));
#15695=CARTESIAN_POINT('Ctrl Pts',(3.71887894508274,-2.52944773220152,4.60377690088598));
#15696=CARTESIAN_POINT('Ctrl Pts',(3.66860843684067,-2.55212043258282,4.60007230453372));
#15697=CARTESIAN_POINT('Ctrl Pts',(3.6183379285986,-2.57479313296412,4.59636770818145));
#15698=CARTESIAN_POINT('Ctrl Pts',(3.55571699253044,-2.5700821395877,4.59266311182918));
#15699=CARTESIAN_POINT('Ctrl Pts',(3.50940445510819,-2.54014346528121,4.58895851547691));
#15700=CARTESIAN_POINT('Ctrl Pts',(3.46312207616628,-2.51022428688169,4.58525633153827));
#15701=CARTESIAN_POINT('Ctrl Pts',(3.43312686289939,-2.45511027311999,4.58155414759963));
#15702=CARTESIAN_POINT('Ctrl Pts',(3.4331235712606,-2.39999932888299,4.57785196366098));
#15703=CARTESIAN_POINT('Ctrl Pts',(3.43341475097665,-2.4001523433056,4.59714803633902));
#15704=CARTESIAN_POINT('Ctrl Pts',(3.43329189093694,-2.41364753260286,4.5980504878702));
#15705=CARTESIAN_POINT('Ctrl Pts',(3.43479419036014,-2.42711571666781,4.59895293940139));
#15706=CARTESIAN_POINT('Ctrl Pts',(3.43802675920227,-2.44015494791281,4.59985539093257));
#15707=CARTESIAN_POINT('Ctrl Pts',(3.45129657184842,-2.49368146633226,4.60355998728484));
#15708=CARTESIAN_POINT('Ctrl Pts',(3.49372371430156,-2.53997956199491,4.60726458363711));
#15709=CARTESIAN_POINT('Ctrl Pts',(3.54589116423991,-2.55786064889342,4.61096917998938));
#15710=CARTESIAN_POINT('Ctrl Pts',(3.59805861417826,-2.57574173579194,4.61467377634165));
#15711=CARTESIAN_POINT('Ctrl Pts',(3.65996637160182,-2.56520581392632,4.61837837269391));
#15712=CARTESIAN_POINT('Ctrl Pts',(3.70328200028476,-2.53107470768073,4.62208296904618));
#15713=CARTESIAN_POINT('Ctrl Pts',(3.74659762896771,-2.49694360143515,4.62578756539845));
#15714=CARTESIAN_POINT('Ctrl Pts',(3.77132112891003,-2.43921731080961,4.62949216175072));
#15715=CARTESIAN_POINT('Ctrl Pts',(3.76613765017139,-2.3843146000394,4.63319675810299));
#15716=CARTESIAN_POINT('Ctrl Pts',(3.76095417143275,-2.32941188926919,4.63690135445526));
#15717=CARTESIAN_POINT('Ctrl Pts',(3.72586371401314,-2.27733275835431,4.64060595080752));
#15718=CARTESIAN_POINT('Ctrl Pts',(3.67692562472706,-2.25191151686662,4.64431054715979));
#15719=CARTESIAN_POINT('Ctrl Pts',(3.62798753544098,-2.22649027537894,4.64801514351206));
#15720=CARTESIAN_POINT('Ctrl Pts',(3.56520181428843,-2.22772692331845,4.65171973986433));
#15721=CARTESIAN_POINT('Ctrl Pts',(3.51730270257413,-2.25505550174341,4.6554243362166));
#15722=CARTESIAN_POINT('Ctrl Pts',(3.46940359085983,-2.28238408016837,4.65912893256887));
#15723=CARTESIAN_POINT('Ctrl Pts',(3.43639108858378,-2.33580458907878,4.66283352892113));
#15724=CARTESIAN_POINT('Ctrl Pts',(3.43337355460624,-2.39086882965689,4.6665381252734));
#15725=CARTESIAN_POINT('Ctrl Pts',(3.43320795605525,-2.39389068741188,4.66674142896194));
#15726=CARTESIAN_POINT('Ctrl Pts',(3.43313269272996,-2.39691749555954,4.66694473265048));
#15727=CARTESIAN_POINT('Ctrl Pts',(3.43314572405529,-2.39994496470472,4.66714803633902));
#15728=CARTESIAN_POINT('Origin',(3.6,-2.4,4.7));
#15729=CARTESIAN_POINT('',(3.43357723227316,-2.39988235337877,4.73714803633902));
#15730=CARTESIAN_POINT('',(3.43362781745768,-2.40008425136911,4.71785196366098));
#15731=CARTESIAN_POINT('',(3.4334,-2.4,4.7));
#15732=CARTESIAN_POINT('Ctrl Pts',(3.43362781745768,-2.40008425136911,4.71785196366098));
#15733=CARTESIAN_POINT('Ctrl Pts',(3.43377992278221,-2.36687021363152,4.7156380408079));
#15734=CARTESIAN_POINT('Ctrl Pts',(3.44340627006936,-2.33357497132763,4.71342411795483));
#15735=CARTESIAN_POINT('Ctrl Pts',(3.46191047910031,-2.30630353350919,4.71121019510175));
#15736=CARTESIAN_POINT('Ctrl Pts',(3.49287390006255,-2.260669753216,4.70750559874949));
#15737=CARTESIAN_POINT('Ctrl Pts',(3.54869526474406,-2.23190257855334,4.70380100239722));
#15738=CARTESIAN_POINT('Ctrl Pts',(3.60382760906969,-2.23316747012655,4.70009640604495));
#15739=CARTESIAN_POINT('Ctrl Pts',(3.65895995339532,-2.23443236169976,4.69639180969269));
#15740=CARTESIAN_POINT('Ctrl Pts',(3.71340327736507,-2.26572931950883,4.69268721334041));
#15741=CARTESIAN_POINT('Ctrl Pts',(3.74224128504954,-2.31273511334664,4.68898261698815));
#15742=CARTESIAN_POINT('Ctrl Pts',(3.77107929273401,-2.35974090718445,4.68527802063588));
#15743=CARTESIAN_POINT('Ctrl Pts',(3.7743119841332,-2.42245553705099,4.68157342428361));
#15744=CARTESIAN_POINT('Ctrl Pts',(3.75045989969766,-2.47217729697168,4.67786882793135));
#15745=CARTESIAN_POINT('Ctrl Pts',(3.72660781526212,-2.52189905689238,4.67416423157908));
#15746=CARTESIAN_POINT('Ctrl Pts',(3.67567095499184,-2.55862794686723,4.67045963522681));
#15747=CARTESIAN_POINT('Ctrl Pts',(3.62096086182118,-2.56555478213231,4.66675503887454));
#15748=CARTESIAN_POINT('Ctrl Pts',(3.56625076865053,-2.57248161739739,4.66305044252227));
#15749=CARTESIAN_POINT('Ctrl Pts',(3.50776744257951,-2.54960639795269,4.65934584617));
#15750=CARTESIAN_POINT('Ctrl Pts',(3.47227610940747,-2.50739809768834,4.65564124981773));
#15751=CARTESIAN_POINT('Ctrl Pts',(3.44740141107113,-2.47781569988784,4.65304482109882));
#15752=CARTESIAN_POINT('Ctrl Pts',(3.43382070888877,-2.43873661594181,4.6504483923799));
#15753=CARTESIAN_POINT('Ctrl Pts',(3.43350339621029,-2.39985729254273,4.64785196366098));
#15754=CARTESIAN_POINT('Ctrl Pts',(3.43314572405529,-2.39994496470472,4.66714803633902));
#15755=CARTESIAN_POINT('Ctrl Pts',(3.43337014931821,-2.45208398679426,4.67064932900275));
#15756=CARTESIAN_POINT('Ctrl Pts',(3.45978247638053,-2.50441905856693,4.67415062166648));
#15757=CARTESIAN_POINT('Ctrl Pts',(3.50195948177967,-2.53504002133992,4.67765191433021));
#15758=CARTESIAN_POINT('Ctrl Pts',(3.54658550860969,-2.56743900019905,4.68135651068247));
#15759=CARTESIAN_POINT('Ctrl Pts',(3.60886012794877,-2.57552898567153,4.68506110703474));
#15760=CARTESIAN_POINT('Ctrl Pts',(3.66028300713527,-2.55560755003253,4.68876570338701));
#15761=CARTESIAN_POINT('Ctrl Pts',(3.71170588632177,-2.53568611439352,4.69247029973927));
#15762=CARTESIAN_POINT('Ctrl Pts',(3.7522770253557,-2.48775325764304,4.69617489609154));
#15763=CARTESIAN_POINT('Ctrl Pts',(3.76342881240416,-2.43374572347072,4.69987949244381));
#15764=CARTESIAN_POINT('Ctrl Pts',(3.77458059945262,-2.3797381892984,4.70358408879608));
#15765=CARTESIAN_POINT('Ctrl Pts',(3.75631303451563,-2.31965597770425,4.70728868514835));
#15766=CARTESIAN_POINT('Ctrl Pts',(3.71698637227073,-2.28099605351363,4.71099328150061));
#15767=CARTESIAN_POINT('Ctrl Pts',(3.67765971002583,-2.24233612932302,4.71469787785288));
#15768=CARTESIAN_POINT('Ctrl Pts',(3.61727395047302,-2.22509849253594,4.71840247420515));
#15769=CARTESIAN_POINT('Ctrl Pts',(3.5634649788822,-2.23717204537206,4.72210707055742));
#15770=CARTESIAN_POINT('Ctrl Pts',(3.50965600729138,-2.24924559820818,4.72581166690969));
#15771=CARTESIAN_POINT('Ctrl Pts',(3.46242382366254,-2.29063034066749,4.72951626326196));
#15772=CARTESIAN_POINT('Ctrl Pts',(3.44338450465812,-2.34238631069604,4.73322085961423));
#15773=CARTESIAN_POINT('Ctrl Pts',(3.43665675680651,-2.36067483856233,4.73452991852249));
#15774=CARTESIAN_POINT('Ctrl Pts',(3.43344927751834,-2.38025835744364,4.73583897743076));
#15775=CARTESIAN_POINT('Ctrl Pts',(3.43357723227316,-2.39988235337877,4.73714803633902));
#15776=CARTESIAN_POINT('Origin',(3.6,-2.4,4.7));
#15777=CARTESIAN_POINT('',(3.43357088161517,-2.40012064492246,4.80714803633902));
#15778=CARTESIAN_POINT('',(3.43319592655187,-2.40009747379871,4.78785196366098));
#15779=CARTESIAN_POINT('',(3.4334,-2.4,4.7));
#15780=CARTESIAN_POINT('Ctrl Pts',(3.43319592655187,-2.40009747379871,4.78785196366098));
#15781=CARTESIAN_POINT('Ctrl Pts',(3.43353982295269,-2.35062359307345,4.78453228558818));
#15782=CARTESIAN_POINT('Ctrl Pts',(3.45695304474081,-2.30086703036466,4.78121260751538));
#15783=CARTESIAN_POINT('Ctrl Pts',(3.49547520498793,-2.2699142173685,4.77789292944258));
#15784=CARTESIAN_POINT('Ctrl Pts',(3.53846402836278,-2.23537241072238,4.77418833309031));
#15785=CARTESIAN_POINT('Ctrl Pts',(3.6002686999986,-2.22424776884202,4.77048373673804));
#15786=CARTESIAN_POINT('Ctrl Pts',(3.65260396146494,-2.24163154716497,4.76677914038577));
#15787=CARTESIAN_POINT('Ctrl Pts',(3.70493922293128,-2.25901532548792,4.76307454403351));
#15788=CARTESIAN_POINT('Ctrl Pts',(3.74780507422814,-2.30490752401418,4.75936994768124));
#15789=CARTESIAN_POINT('Ctrl Pts',(3.7615837154436,-2.35830531786175,4.75566535132897));
#15790=CARTESIAN_POINT('Ctrl Pts',(3.77536235665906,-2.41170311170932,4.75196075497671));
#15791=CARTESIAN_POINT('Ctrl Pts',(3.76005378779311,-2.4726065008782,4.74825615862444));
#15792=CARTESIAN_POINT('Ctrl Pts',(3.72266406219276,-2.51314270396953,4.74455156227217));
#15793=CARTESIAN_POINT('Ctrl Pts',(3.68527433659241,-2.55367890706087,4.7408469659199));
#15794=CARTESIAN_POINT('Ctrl Pts',(3.62580345425764,-2.57384792407467,4.73714236956763));
#15795=CARTESIAN_POINT('Ctrl Pts',(3.57146860171181,-2.56441929000846,4.73343777321536));
#15796=CARTESIAN_POINT('Ctrl Pts',(3.51713374916598,-2.55499065594226,4.7297331768631));
#15797=CARTESIAN_POINT('Ctrl Pts',(3.46793492640908,-2.51596437079605,4.72602858051083));
#15798=CARTESIAN_POINT('Ctrl Pts',(3.4463882536521,-2.46520103526108,4.72232398415856));
#15799=CARTESIAN_POINT('Ctrl Pts',(3.43771819866623,-2.44477463739825,4.72083331065937));
#15800=CARTESIAN_POINT('Ctrl Pts',(3.43352540224658,-2.42244785170318,4.71934263716017));
#15801=CARTESIAN_POINT('Ctrl Pts',(3.43362781745768,-2.40008425136911,4.71785196366098));
#15802=CARTESIAN_POINT('Ctrl Pts',(3.43357723227316,-2.39988235337877,4.73714803633902));
#15803=CARTESIAN_POINT('Ctrl Pts',(3.43381138552965,-2.4357936609347,4.73954357378302));
#15804=CARTESIAN_POINT('Ctrl Pts',(3.44521519749436,-2.4718405175289,4.74193911122702));
#15805=CARTESIAN_POINT('Ctrl Pts',(3.46665596946098,-2.50033503922361,4.74433464867103));
#15806=CARTESIAN_POINT('Ctrl Pts',(3.49981320764826,-2.54440060012484,4.74803924502329));
#15807=CARTESIAN_POINT('Ctrl Pts',(3.55697413840284,-2.57040452432951,4.75174384137556));
#15808=CARTESIAN_POINT('Ctrl Pts',(3.61197873764036,-2.56644596847307,4.75544843772783));
#15809=CARTESIAN_POINT('Ctrl Pts',(3.66698333687788,-2.56248741261664,4.7591530340801));
#15810=CARTESIAN_POINT('Ctrl Pts',(3.71983160459833,-2.52856637669909,4.76285763043237));
#15811=CARTESIAN_POINT('Ctrl Pts',(3.7463372314094,-2.48020701515346,4.76656222678464));
#15812=CARTESIAN_POINT('Ctrl Pts',(3.77284285822047,-2.43184765360783,4.7702668231369));
#15813=CARTESIAN_POINT('Ctrl Pts',(3.77300584412214,-2.36904996643411,4.77397141948917));
#15814=CARTESIAN_POINT('Ctrl Pts',(3.74675159769234,-2.32055367125447,4.77767601584144));
#15815=CARTESIAN_POINT('Ctrl Pts',(3.72049735126253,-2.27205737607482,4.78138061219371));
#15816=CARTESIAN_POINT('Ctrl Pts',(3.66782587250124,-2.23786247288924,4.78508520854598));
#15817=CARTESIAN_POINT('Ctrl Pts',(3.61284256233116,-2.23361845303891,4.78878980489824));
#15818=CARTESIAN_POINT('Ctrl Pts',(3.55785925216109,-2.22937443318857,4.79249440125051));
#15819=CARTESIAN_POINT('Ctrl Pts',(3.50056411058224,-2.25508129667347,4.79619899760278));
#15820=CARTESIAN_POINT('Ctrl Pts',(3.46717858402372,-2.29897415165191,4.79990359395505));
#15821=CARTESIAN_POINT('Ctrl Pts',(3.44541647189655,-2.32758538921762,4.80231840808304));
#15822=CARTESIAN_POINT('Ctrl Pts',(3.43381352935432,-2.36392383491678,4.80473322221103));
#15823=CARTESIAN_POINT('Ctrl Pts',(3.43357088161517,-2.40012064492246,4.80714803633902));
#15824=CARTESIAN_POINT('Origin',(3.6,-2.4,4.7));
#15825=CARTESIAN_POINT('',(3.43314189260959,-2.4000500574177,4.87714803633902));
#15826=CARTESIAN_POINT('',(3.43333250832843,-2.39985412494998,4.85785196366098));
#15827=CARTESIAN_POINT('',(3.4334,-2.4,4.7));
#15828=CARTESIAN_POINT('Ctrl Pts',(3.43333250832843,-2.39985412494998,4.85785196366098));
#15829=CARTESIAN_POINT('Ctrl Pts',(3.43323384369475,-2.3890884237173,4.85713112672072));
#15830=CARTESIAN_POINT('Ctrl Pts',(3.43418764919828,-2.37834013090661,4.85641028978047));
#15831=CARTESIAN_POINT('Ctrl Pts',(3.4362574396422,-2.36781122023692,4.85568945284021));
#15832=CARTESIAN_POINT('Ctrl Pts',(3.44689471098651,-2.31370000328629,4.85198485648794));
#15833=CARTESIAN_POINT('Ctrl Pts',(3.48700781310569,-2.26538319325753,4.84828026013567));
#15834=CARTESIAN_POINT('Ctrl Pts',(3.53823875735816,-2.24497325223528,4.8445756637834));
#15835=CARTESIAN_POINT('Ctrl Pts',(3.58946970161063,-2.22456331121304,4.84087106743114));
#15836=CARTESIAN_POINT('Ctrl Pts',(3.65181848799641,-2.23206023919731,4.83716647107887));
#15837=CARTESIAN_POINT('Ctrl Pts',(3.69675084088435,-2.26403302458561,4.8334618747266));
#15838=CARTESIAN_POINT('Ctrl Pts',(3.74168319377229,-2.2960058099739,4.82975727837434));
#15839=CARTESIAN_POINT('Ctrl Pts',(3.76919911316239,-2.35245445276622,4.82605268202207));
#15840=CARTESIAN_POINT('Ctrl Pts',(3.76670578251992,-2.40754491150309,4.8223480856698));
#15841=CARTESIAN_POINT('Ctrl Pts',(3.76421245187744,-2.46263537023996,4.81864348931753));
#15842=CARTESIAN_POINT('Ctrl Pts',(3.73170987120238,-2.51636764492139,4.81493889296526));
#15843=CARTESIAN_POINT('Ctrl Pts',(3.68407303084285,-2.54415085535669,4.81123429661299));
#15844=CARTESIAN_POINT('Ctrl Pts',(3.63643619048332,-2.57193406579199,4.80752970026073));
#15845=CARTESIAN_POINT('Ctrl Pts',(3.57366509043931,-2.57376821198116,4.80382510390846));
#15846=CARTESIAN_POINT('Ctrl Pts',(3.52448728058231,-2.54881388652042,4.80012050755619));
#15847=CARTESIAN_POINT('Ctrl Pts',(3.47530947072531,-2.52385956105968,4.79641591120392));
#15848=CARTESIAN_POINT('Ctrl Pts',(3.43972495105532,-2.47211676394902,4.79271131485165));
#15849=CARTESIAN_POINT('Ctrl Pts',(3.43401917877726,-2.41726587968776,4.78900671849938));
#15850=CARTESIAN_POINT('Ctrl Pts',(3.43342633252912,-2.41156671411356,4.78862180021992));
#15851=CARTESIAN_POINT('Ctrl Pts',(3.43315605159773,-2.40583399421718,4.78823688194045));
#15852=CARTESIAN_POINT('Ctrl Pts',(3.43319592655187,-2.40009747379871,4.78785196366098));
#15853=CARTESIAN_POINT('Ctrl Pts',(3.43357088161517,-2.40012064492246,4.80714803633902));
#15854=CARTESIAN_POINT('Ctrl Pts',(3.43344128044335,-2.4194538108087,4.8084378185633));
#15855=CARTESIAN_POINT('Ctrl Pts',(3.43655249964156,-2.4387465714195,4.80972760078758));
#15856=CARTESIAN_POINT('Ctrl Pts',(3.44308755405667,-2.45679995496896,4.81101738301185));
#15857=CARTESIAN_POINT('Ctrl Pts',(3.46185796218633,-2.50865405683559,4.81472197936412));
#15858=CARTESIAN_POINT('Ctrl Pts',(3.50887468998386,-2.55028341409687,4.81842657571639));
#15859=CARTESIAN_POINT('Ctrl Pts',(3.56262026536972,-2.56263611534763,4.82213117206866));
#15860=CARTESIAN_POINT('Ctrl Pts',(3.61636584075558,-2.5749888165984,4.82583576842092));
#15861=CARTESIAN_POINT('Ctrl Pts',(3.67684026372979,-2.55806486183865,4.82954036477319));
#15862=CARTESIAN_POINT('Ctrl Pts',(3.71636707170489,-2.51960959492959,4.83324496112546));
#15863=CARTESIAN_POINT('Ctrl Pts',(3.75589387967999,-2.48115432802054,4.83694955747773));
#15864=CARTESIAN_POINT('Ctrl Pts',(3.77447307265599,-2.42116774896216,4.84065415383));
#15865=CARTESIAN_POINT('Ctrl Pts',(3.76360177761623,-2.36710305580748,4.84435875018227));
#15866=CARTESIAN_POINT('Ctrl Pts',(3.75273048257646,-2.3130383626528,4.84806334653453));
#15867=CARTESIAN_POINT('Ctrl Pts',(3.71240869952093,-2.26489555540181,4.8517679428868));
#15868=CARTESIAN_POINT('Ctrl Pts',(3.66108992110507,-2.24470746278141,4.85547253923907));
#15869=CARTESIAN_POINT('Ctrl Pts',(3.60977114268922,-2.224519370161,4.85917713559134));
#15870=CARTESIAN_POINT('Ctrl Pts',(3.54745536891304,-2.23228599217118,4.86288173194361));
#15871=CARTESIAN_POINT('Ctrl Pts',(3.50266176699964,-2.26445289020885,4.86658632829587));
#15872=CARTESIAN_POINT('Ctrl Pts',(3.4600933015382,-2.29502188733407,4.87010689764359));
#15873=CARTESIAN_POINT('Ctrl Pts',(3.43334940736011,-2.34762718854044,4.87362746699131));
#15874=CARTESIAN_POINT('Ctrl Pts',(3.43314189260959,-2.4000500574177,4.87714803633902));
#15875=CARTESIAN_POINT('Origin',(3.6,-2.4,4.7));
#15876=CARTESIAN_POINT('',(3.43342339329134,-2.39984780956037,4.94714803633902));
#15877=CARTESIAN_POINT('',(3.43366987537036,-2.39999366746476,4.92785196366098));
#15878=CARTESIAN_POINT('',(3.4334,-2.4,4.7));
#15879=CARTESIAN_POINT('Ctrl Pts',(3.43366987537036,-2.39999366746476,4.92785196366098));
#15880=CARTESIAN_POINT('Ctrl Pts',(3.43366057869757,-2.37257318362641,4.926025371501));
#15881=CARTESIAN_POINT('Ctrl Pts',(3.44006468998231,-2.34515678783965,4.92419877934102));
#15882=CARTESIAN_POINT('Ctrl Pts',(3.45290605548974,-2.32118937188857,4.92237218718104));
#15883=CARTESIAN_POINT('Ctrl Pts',(3.47895022498703,-2.27257994300186,4.91866759082877));
#15884=CARTESIAN_POINT('Ctrl Pts',(3.53147325377826,-2.23815747156893,4.9149629944765));
#15885=CARTESIAN_POINT('Ctrl Pts',(3.58643767991325,-2.23367559683213,4.91125839812423));
#15886=CARTESIAN_POINT('Ctrl Pts',(3.64140210604824,-2.22919372209532,4.90755380177196));
#15887=CARTESIAN_POINT('Ctrl Pts',(3.69880792952698,-2.25465244405464,4.9038492054197));
#15888=CARTESIAN_POINT('Ctrl Pts',(3.7323830497203,-2.29840043424344,4.90014460906743));
#15889=CARTESIAN_POINT('Ctrl Pts',(3.76595816991362,-2.34214842443224,4.89644001271516));
#15890=CARTESIAN_POINT('Ctrl Pts',(3.77570258682152,-2.40418568285053,4.89273541636289));
#15891=CARTESIAN_POINT('Ctrl Pts',(3.75715671279198,-2.45612050640859,4.88903082001062));
#15892=CARTESIAN_POINT('Ctrl Pts',(3.73861083876244,-2.50805532996664,4.88532622365835));
#15893=CARTESIAN_POINT('Ctrl Pts',(3.69177467379546,-2.54988771866446,4.88162162730609));
#15894=CARTESIAN_POINT('Ctrl Pts',(3.63808305436706,-2.56247284260842,4.87791703095382));
#15895=CARTESIAN_POINT('Ctrl Pts',(3.58439143493865,-2.57505796655237,4.87421243460155));
#15896=CARTESIAN_POINT('Ctrl Pts',(3.52384436104883,-2.55839582574246,4.87050783824928));
#15897=CARTESIAN_POINT('Ctrl Pts',(3.48415154438863,-2.52011194340126,4.86680324189701));
#15898=CARTESIAN_POINT('Ctrl Pts',(3.45218211937245,-2.4892773035642,4.863819482485));
#15899=CARTESIAN_POINT('Ctrl Pts',(3.4337409107187,-2.4444165781012,4.86083572307299));
#15900=CARTESIAN_POINT('Ctrl Pts',(3.43333250832843,-2.39985412494998,4.85785196366098));
#15901=CARTESIAN_POINT('Ctrl Pts',(3.43314189260959,-2.4000500574177,4.87714803633902));
#15902=CARTESIAN_POINT('Ctrl Pts',(3.43313104541013,-2.4027903026953,4.87733206334358));
#15903=CARTESIAN_POINT('Ctrl Pts',(3.43319270505025,-2.40553004950279,4.87751609034813));
#15904=CARTESIAN_POINT('Ctrl Pts',(3.43332840145004,-2.40826612443654,4.87770011735268));
#15905=CARTESIAN_POINT('Ctrl Pts',(3.43606006786446,-2.46334528656136,4.88140471370495));
#15906=CARTESIAN_POINT('Ctrl Pts',(3.46879483074392,-2.51693643674581,4.88510931005721));
#15907=CARTESIAN_POINT('Ctrl Pts',(3.51655144023777,-2.54451328122398,4.88881390640948));
#15908=CARTESIAN_POINT('Ctrl Pts',(3.56430804973163,-2.57209012570216,4.89251850276175));
#15909=CARTESIAN_POINT('Ctrl Pts',(3.62708650583988,-2.57365266447405,4.89622309911402));
#15910=CARTESIAN_POINT('Ctrl Pts',(3.67615589214678,-2.54848579281353,4.89992769546629));
#15911=CARTESIAN_POINT('Ctrl Pts',(3.72522527845368,-2.52331892115301,4.90363229181856));
#15912=CARTESIAN_POINT('Ctrl Pts',(3.76058559495924,-2.47142263906009,4.90733688817082));
#15913=CARTESIAN_POINT('Ctrl Pts',(3.76605399230753,-2.41654757430046,4.91104148452309));
#15914=CARTESIAN_POINT('Ctrl Pts',(3.77152238965583,-2.36167250954082,4.91474608087536));
#15915=CARTESIAN_POINT('Ctrl Pts',(3.74709886784687,-2.30381866211447,4.91845067722763));
#15916=CARTESIAN_POINT('Ctrl Pts',(3.70396099012833,-2.26946317336186,4.9221552735799));
#15917=CARTESIAN_POINT('Ctrl Pts',(3.6608231124098,-2.23510768460924,4.92585986993216));
#15918=CARTESIAN_POINT('Ctrl Pts',(3.5989708787817,-2.22425055453036,4.92956446628443));
#15919=CARTESIAN_POINT('Ctrl Pts',(3.54671131468788,-2.24186061024559,4.9332690626367));
#15920=CARTESIAN_POINT('Ctrl Pts',(3.49445175059407,-2.25947066596082,4.93697365898896));
#15921=CARTESIAN_POINT('Ctrl Pts',(3.45178485603454,-2.30554790747016,4.94067825534124));
#15922=CARTESIAN_POINT('Ctrl Pts',(3.43823737724635,-2.35900482396987,4.94438285169351));
#15923=CARTESIAN_POINT('Ctrl Pts',(3.43486667440692,-2.37230526038685,4.94530457990868));
#15924=CARTESIAN_POINT('Ctrl Pts',(3.43329860172231,-2.38606253373953,4.94622630812385));
#15925=CARTESIAN_POINT('Ctrl Pts',(3.43342339329134,-2.39984780956037,4.94714803633902));
#15926=CARTESIAN_POINT('Origin',(3.6,-2.4,4.7));
#15927=CARTESIAN_POINT('',(3.43365998837939,-2.40004261214837,5.01714803633902));
#15928=CARTESIAN_POINT('',(3.4333557533513,-2.40014916294441,4.99785196366098));
#15929=CARTESIAN_POINT('',(3.4334,-2.4,4.7));
#15930=CARTESIAN_POINT('Ctrl Pts',(3.4333557533513,-2.40014916294441,4.99785196366098));
#15931=CARTESIAN_POINT('Ctrl Pts',(3.43376006878861,-2.35633883086337,4.99491961628128));
#15932=CARTESIAN_POINT('Ctrl Pts',(3.45150379646176,-2.31223873171809,4.99198726890157));
#15933=CARTESIAN_POINT('Ctrl Pts',(3.48249984549986,-2.28150334481789,4.98905492152186));
#15934=CARTESIAN_POINT('Ctrl Pts',(3.5216588656746,-2.24267363351424,4.98535032516959));
#15935=CARTESIAN_POINT('Ctrl Pts',(3.58196947066853,-2.22517489033693,4.98164572881732));
#15936=CARTESIAN_POINT('Ctrl Pts',(3.63583017024712,-2.23701551447795,4.97794113246505));
#15937=CARTESIAN_POINT('Ctrl Pts',(3.68969086982571,-2.24885613861896,4.97423653611278));
#15938=CARTESIAN_POINT('Ctrl Pts',(3.73710166398897,-2.29003613007831,4.97053193976052));
#15939=CARTESIAN_POINT('Ctrl Pts',(3.75636473388799,-2.34170923218213,4.96682734340825));
#15940=CARTESIAN_POINT('Ctrl Pts',(3.775627803787,-2.39338233428594,4.96312274705599));
#15941=CARTESIAN_POINT('Ctrl Pts',(3.76674314942177,-2.45554854703422,4.95941815070372));
#15942=CARTESIAN_POINT('Ctrl Pts',(3.73377688327324,-2.49975715069431,4.95571355435145));
#15943=CARTESIAN_POINT('Ctrl Pts',(3.7008106171247,-2.54396575435439,4.95200895799918));
#15944=CARTESIAN_POINT('Ctrl Pts',(3.64376273919286,-2.57021674892629,4.94830436164691));
#15945=CARTESIAN_POINT('Ctrl Pts',(3.58874153428106,-2.56649621787192,4.94459976529464));
#15946=CARTESIAN_POINT('Ctrl Pts',(3.53372032936927,-2.56277568681755,4.94089516894238));
#15947=CARTESIAN_POINT('Ctrl Pts',(3.48072579747752,-2.52908363013692,4.93719057259011));
#15948=CARTESIAN_POINT('Ctrl Pts',(3.45401118663332,-2.48083940862635,4.93348597623784));
#15949=CARTESIAN_POINT('Ctrl Pts',(3.4404685098097,-2.45638253353524,4.93160797204555));
#15950=CARTESIAN_POINT('Ctrl Pts',(3.43367943371122,-2.42818593979086,4.92972996785327));
#15951=CARTESIAN_POINT('Ctrl Pts',(3.43366987537036,-2.39999366746476,4.92785196366098));
#15952=CARTESIAN_POINT('Ctrl Pts',(3.43342339329134,-2.39984780956037,4.94714803633902));
#15953=CARTESIAN_POINT('Ctrl Pts',(3.43380016214308,-2.44146810957007,4.94993090447612));
#15954=CARTESIAN_POINT('Ctrl Pts',(3.44960819947038,-2.48334366548894,4.95271377261321));
#15955=CARTESIAN_POINT('Ctrl Pts',(3.47782660292827,-2.51367238728015,4.95549664075031));
#15956=CARTESIAN_POINT('Ctrl Pts',(3.51539137041525,-2.55404644260063,4.95920123710258));
#15957=CARTESIAN_POINT('Ctrl Pts',(3.57494896840608,-2.57395796175148,4.96290583345484));
#15958=CARTESIAN_POINT('Ctrl Pts',(3.62924252448225,-2.56429432528282,4.96661042980711));
#15959=CARTESIAN_POINT('Ctrl Pts',(3.68353608055842,-2.55463068881416,4.97031502615938));
#15960=CARTESIAN_POINT('Ctrl Pts',(3.73256559471993,-2.51539189672599,4.97401962251165));
#15961=CARTESIAN_POINT('Ctrl Pts',(3.75389243176138,-2.46453580432507,4.97772421886392));
#15962=CARTESIAN_POINT('Ctrl Pts',(3.77521926880282,-2.41367971192415,4.98142881521619));
#15963=CARTESIAN_POINT('Ctrl Pts',(3.7688434287242,-2.35120631921049,4.98513341156845));
#15964=CARTESIAN_POINT('Ctrl Pts',(3.73768285095733,-2.30570692939164,4.98883800792072));
#15965=CARTESIAN_POINT('Ctrl Pts',(3.70652227319045,-2.26020753957279,4.99254260427299));
#15966=CARTESIAN_POINT('Ctrl Pts',(3.65057695773533,-2.23168215264876,4.99624720062526));
#15967=CARTESIAN_POINT('Ctrl Pts',(3.59545059530862,-2.23318557212546,4.99995179697752));
#15968=CARTESIAN_POINT('Ctrl Pts',(3.5403242328819,-2.23468899160217,5.00365639332979));
#15969=CARTESIAN_POINT('Ctrl Pts',(3.48601682348359,-2.2662212174796,5.00736098968206));
#15970=CARTESIAN_POINT('Ctrl Pts',(3.4573824612349,-2.31335135092863,5.01106558603433));
#15971=CARTESIAN_POINT('Ctrl Pts',(3.44171120056098,-2.3391451367466,5.01309306946923));
#15972=CARTESIAN_POINT('Ctrl Pts',(3.43372965513495,-2.36961088327844,5.01512055290413));
#15973=CARTESIAN_POINT('Ctrl Pts',(3.43365998837939,-2.40004261214837,5.01714803633902));
#15974=CARTESIAN_POINT('Origin',(3.6,-2.4,4.7));
#15975=CARTESIAN_POINT('',(3.43326718206005,-2.40013003210005,5.08714803633902));
#15976=CARTESIAN_POINT('',(3.43317939237559,-2.39991359865598,5.06785196366098));
#15977=CARTESIAN_POINT('',(3.4334,-2.4,4.7));
#15978=CARTESIAN_POINT('Ctrl Pts',(3.43317939237559,-2.39991359865598,5.06785196366098));
#15979=CARTESIAN_POINT('Ctrl Pts',(3.43314802801357,-2.39494457971841,5.06751845741381));
#15980=CARTESIAN_POINT('Ctrl Pts',(3.43335080279482,-2.38997815623028,5.06718495116665));
#15981=CARTESIAN_POINT('Ctrl Pts',(3.43379605546717,-2.38503356765244,5.06685144491949));
#15982=CARTESIAN_POINT('Ctrl Pts',(3.43874193411214,-2.33010894490636,5.06314684856722));
#15983=CARTESIAN_POINT('Ctrl Pts',(3.47360673801625,-2.27787849376484,5.05944225221495));
#15984=CARTESIAN_POINT('Ctrl Pts',(3.52243437581894,-2.25224575672994,5.05573765586269));
#15985=CARTESIAN_POINT('Ctrl Pts',(3.57126201362163,-2.22661301969504,5.05203305951042));
#15986=CARTESIAN_POINT('Ctrl Pts',(3.63405248532289,-2.22757799676674,5.04832846315815));
#15987=CARTESIAN_POINT('Ctrl Pts',(3.68206938357278,-2.25469907052132,5.04462386680588));
#15988=CARTESIAN_POINT('Ctrl Pts',(3.73008628182266,-2.28182014427589,5.04091927045361));
#15989=CARTESIAN_POINT('Ctrl Pts',(3.76332960662116,-2.33509731471334,5.03721467410135));
#15990=CARTESIAN_POINT('Ctrl Pts',(3.7665853578407,-2.39014797778335,5.03351007774908));
#15991=CARTESIAN_POINT('Ctrl Pts',(3.76984110906023,-2.44519864085336,5.02980548139681));
#15992=CARTESIAN_POINT('Ctrl Pts',(3.7431092867008,-2.50202279655593,5.02610088504454));
#15993=CARTESIAN_POINT('Ctrl Pts',(3.69862386285843,-2.53461455026518,5.02239628869228));
#15994=CARTESIAN_POINT('Ctrl Pts',(3.65413843901607,-2.56720630397444,5.01869169234001));
#15995=CARTESIAN_POINT('Ctrl Pts',(3.59189941369078,-2.57556565569037,5.01498709598774));
#15996=CARTESIAN_POINT('Ctrl Pts',(3.54039082873623,-2.55586689947754,5.01128249963547));
#15997=CARTESIAN_POINT('Ctrl Pts',(3.48888224378167,-2.53616814326471,5.0075779032832));
#15998=CARTESIAN_POINT('Ctrl Pts',(3.44810409919785,-2.48841127912311,5.00387330693093));
#15999=CARTESIAN_POINT('Ctrl Pts',(3.43671874458371,-2.43445250733732,5.00016871057866));
#16000=CARTESIAN_POINT('Ctrl Pts',(3.43434538792972,-2.42320442465572,4.9993964616061));
#16001=CARTESIAN_POINT('Ctrl Pts',(3.43324927477267,-2.41168684233781,4.99862421263354));
#16002=CARTESIAN_POINT('Ctrl Pts',(3.4333557533513,-2.40014916294441,4.99785196366098));
#16003=CARTESIAN_POINT('Ctrl Pts',(3.43365998837939,-2.40004261214837,5.01714803633902));
#16004=CARTESIAN_POINT('Ctrl Pts',(3.43360236077384,-2.42521541736454,5.01882514925639));
#16005=CARTESIAN_POINT('Ctrl Pts',(3.43895837597341,-2.45036494625428,5.02050226217376));
#16006=CARTESIAN_POINT('Ctrl Pts',(3.44985377805168,-2.47282762403026,5.02217937509113));
#16007=CARTESIAN_POINT('Ctrl Pts',(3.47392077221621,-2.52244572266223,5.0258839714434));
#16008=CARTESIAN_POINT('Ctrl Pts',(3.52501607564434,-2.55895387890556,5.02958856779567));
#16009=CARTESIAN_POINT('Ctrl Pts',(3.57975563405926,-2.56564394064586,5.03329316414793));
#16010=CARTESIAN_POINT('Ctrl Pts',(3.63449519247418,-2.57233400238615,5.0369977605002));
#16011=CARTESIAN_POINT('Ctrl Pts',(3.69287900587587,-2.54920596962341,5.04070235685248));
#16012=CARTESIAN_POINT('Ctrl Pts',(3.72818738886538,-2.5068444924534,5.04440695320474));
#16013=CARTESIAN_POINT('Ctrl Pts',(3.76349577185488,-2.4644830152834,5.04811154955701));
#16014=CARTESIAN_POINT('Ctrl Pts',(3.77572872443219,-2.40288809370614,5.05181614590928));
#16015=CARTESIAN_POINT('Ctrl Pts',(3.75928777076399,-2.35024904339754,5.05552074226154));
#16016=CARTESIAN_POINT('Ctrl Pts',(3.74284681709578,-2.29760999308894,5.05922533861381));
#16017=CARTESIAN_POINT('Ctrl Pts',(3.69773195718207,-2.25392681404901,5.06292993496608));
#16018=CARTESIAN_POINT('Ctrl Pts',(3.6445902539118,-2.239191259641,5.06663453131835));
#16019=CARTESIAN_POINT('Ctrl Pts',(3.59144855064154,-2.22445570523299,5.07033912767062));
#16020=CARTESIAN_POINT('Ctrl Pts',(3.53028000401472,-2.2386677754569,5.07404372402289));
#16021=CARTESIAN_POINT('Ctrl Pts',(3.48907876340423,-2.27532343849,5.07774832037515));
#16022=CARTESIAN_POINT('Ctrl Pts',(3.45423196569032,-2.3063257203596,5.08088155902977));
#16023=CARTESIAN_POINT('Ctrl Pts',(3.43366833898609,-2.35338253026132,5.0840147976844));
#16024=CARTESIAN_POINT('Ctrl Pts',(3.43326718206005,-2.40013003210005,5.08714803633902));
#16025=CARTESIAN_POINT('Origin',(3.6,-2.4,4.7));
#16026=CARTESIAN_POINT('',(3.43325215766083,-2.39987843114813,5.15714803633902));
#16027=CARTESIAN_POINT('',(3.43361559198215,-2.39990578567643,5.13785196366098));
#16028=CARTESIAN_POINT('',(3.4334,-2.4,4.7));
#16029=CARTESIAN_POINT('',(3.72690708798524,-2.29206413469515,5.2));
#16030=CARTESIAN_POINT('Ctrl Pts',(3.43325215766083,-2.39987843114813,5.15714803633902));
#16031=CARTESIAN_POINT('Ctrl Pts',(3.43364568926707,-2.44715561674071,5.16031823516921));
#16032=CARTESIAN_POINT('Ctrl Pts',(3.45475450700198,-2.49473162154361,5.1634884339994));
#16033=CARTESIAN_POINT('Ctrl Pts',(3.49032381647516,-2.52575978121339,5.16665863282959));
#16034=CARTESIAN_POINT('Ctrl Pts',(3.53188901196771,-2.56201832942672,5.17036322918186));
#16035=CARTESIAN_POINT('Ctrl Pts',(3.59320078561411,-2.575679906312,5.17406782553413));
#16036=CARTESIAN_POINT('Ctrl Pts',(3.64619137793262,-2.5603849196725,5.17777242188639));
#16037=CARTESIAN_POINT('Ctrl Pts',(3.69918197025112,-2.545089933033,5.18147701823866));
#16038=CARTESIAN_POINT('Ctrl Pts',(3.74385138124173,-2.50083838286872,5.18518161459093));
#16039=CARTESIAN_POINT('Ctrl Pts',(3.75975547145412,-2.44813183978448,5.1888862109432));
#16040=CARTESIAN_POINT('Ctrl Pts',(3.7756595616665,-2.39542529670025,5.19259080729546));
#16041=CARTESIAN_POINT('Ctrl Pts',(3.76279833110066,-2.33426376069605,5.19629540364773));
#16042=CARTESIAN_POINT('Ctrl Pts',(3.72690708798524,-2.29206413469515,5.2));
#16043=CARTESIAN_POINT('',(3.47285247305911,-2.29187966783456,5.2));
#16044=CARTESIAN_POINT('Origin',(3.6,-2.4,5.2));
#16045=CARTESIAN_POINT('Ctrl Pts',(3.47285232078578,-2.29187955100914,5.2));
#16046=CARTESIAN_POINT('Ctrl Pts',(3.50793811899511,-2.25072740472549,5.19636770818144));
#16047=CARTESIAN_POINT('Ctrl Pts',(3.5649358740211,-2.22812243199181,5.19273541636289));
#16048=CARTESIAN_POINT('Ctrl Pts',(3.61867624862122,-2.23418211249055,5.18910312454433));
#16049=CARTESIAN_POINT('Ctrl Pts',(3.67348638108252,-2.24036241721079,5.18539852819207));
#16050=CARTESIAN_POINT('Ctrl Pts',(3.72490815931237,-2.27635993281072,5.1816939318398));
#16051=CARTESIAN_POINT('Ctrl Pts',(3.74944162123119,-2.32574103985171,5.17798933548753));
#16052=CARTESIAN_POINT('Ctrl Pts',(3.77397508315002,-2.37512214689269,5.17428473913527));
#16053=CARTESIAN_POINT('Ctrl Pts',(3.77162022875783,-2.43788684537472,5.17058014278299));
#16054=CARTESIAN_POINT('Ctrl Pts',(3.74343805414309,-2.48529019582313,5.16687554643072));
#16055=CARTESIAN_POINT('Ctrl Pts',(3.71525587952836,-2.53269354627153,5.16317095007846));
#16056=CARTESIAN_POINT('Ctrl Pts',(3.66124638469108,-2.5647355486863,5.15946635372619));
#16057=CARTESIAN_POINT('Ctrl Pts',(3.60613566942556,-2.56676214228893,5.15576175737392));
#16058=CARTESIAN_POINT('Ctrl Pts',(3.55102495416005,-2.56878873589157,5.15205716102166));
#16059=CARTESIAN_POINT('Ctrl Pts',(3.49481301846629,-2.54079992068208,5.14835256466939));
#16060=CARTESIAN_POINT('Ctrl Pts',(3.46322140367409,-2.49559987057215,5.14464796831712));
#16061=CARTESIAN_POINT('Ctrl Pts',(3.44390335110665,-2.46796035452279,5.14238263343174));
#16062=CARTESIAN_POINT('Ctrl Pts',(3.43379142096037,-2.43388514918463,5.14011729854636));
#16063=CARTESIAN_POINT('Ctrl Pts',(3.43361559198215,-2.39990578567643,5.13785196366098));
#16064=CARTESIAN_POINT('Origin',(3.6,-2.4,5.35459252805377));
#16065=CARTESIAN_POINT('',(3.39427732444531,-2.39988044480691,4.34540747194623));
#16066=CARTESIAN_POINT('',(3.39483887958286,-2.40008013132228,4.33959252805377));
#16067=CARTESIAN_POINT('',(3.394525,-2.39999999999999,5.35459252805377));
#16068=CARTESIAN_POINT('',(3.78826275096636,-2.48232321801033,4.3));
#16069=CARTESIAN_POINT('Ctrl Pts',(3.39483887958286,-2.40008013132228,4.33959252805377));
#16070=CARTESIAN_POINT('Ctrl Pts',(3.39495668787724,-2.361520075325,4.33750880775932));
#16071=CARTESIAN_POINT('Ctrl Pts',(3.4239416532562,-2.25423614055743,4.3317204911126));
#16072=CARTESIAN_POINT('Ctrl Pts',(3.59702530195382,-2.15700945407857,4.32222757811361));
#16073=CARTESIAN_POINT('Ctrl Pts',(3.80250230755732,-2.26611609660926,4.31111378905681));
#16074=CARTESIAN_POINT('Ctrl Pts',(3.81563717950601,-2.41972137435598,4.30370459635227));
#16075=CARTESIAN_POINT('Ctrl Pts',(3.78826275096636,-2.48232321801033,4.3));
#16076=CARTESIAN_POINT('',(3.72235839003881,-2.56553532314028,4.3));
#16077=CARTESIAN_POINT('Origin',(3.6,-2.4,4.3));
#16078=CARTESIAN_POINT('Ctrl Pts',(3.39427732444531,-2.39988044480691,4.34540747194623));
#16079=CARTESIAN_POINT('Ctrl Pts',(3.39422705601106,-2.39271640856816,4.34501772883951));
#16080=CARTESIAN_POINT('Ctrl Pts',(3.39781628789546,-2.31750701228878,4.34092338938053));
#16081=CARTESIAN_POINT('Ctrl Pts',(3.49037003077072,-2.18326698967564,4.33312445356928));
#16082=CARTESIAN_POINT('Ctrl Pts',(3.72265543153543,-2.19039239422561,4.32201066451247));
#16083=CARTESIAN_POINT('Ctrl Pts',(3.84179827282652,-2.38799091139141,4.31096917998938));
#16084=CARTESIAN_POINT('Ctrl Pts',(3.77594285680537,-2.52582029152411,4.30363229181855));
#16085=CARTESIAN_POINT('Ctrl Pts',(3.72235852099786,-2.56553552032367,4.3));
#16086=CARTESIAN_POINT('Origin',(3.6,-2.4,5.35459252805377));
#16087=CARTESIAN_POINT('',(3.39480735688311,-2.3998973457609,4.41540747194623));
#16088=CARTESIAN_POINT('',(3.39433274578554,-2.4001497810388,4.40959252805377));
#16089=CARTESIAN_POINT('',(3.394525,-2.39999999999999,5.35459252805377));
#16090=CARTESIAN_POINT('Ctrl Pts',(3.39433274578554,-2.4001497810388,4.40959252805377));
#16091=CARTESIAN_POINT('Ctrl Pts',(3.39481384891428,-2.34148051031483,4.40640305253959));
#16092=CARTESIAN_POINT('Ctrl Pts',(3.45186170282621,-2.21384965704481,4.39950898067315));
#16093=CARTESIAN_POINT('Ctrl Pts',(3.66843098386609,-2.16697244123634,4.38891031245443));
#16094=CARTESIAN_POINT('Ctrl Pts',(3.83289206448147,-2.33111753521892,4.37779652339763));
#16095=CARTESIAN_POINT('Ctrl Pts',(3.7841810615649,-2.55829573402952,4.36668273434082));
#16096=CARTESIAN_POINT('Ctrl Pts',(3.56689372435994,-2.6406156849541,4.35556894528403));
#16097=CARTESIAN_POINT('Ctrl Pts',(3.4149557748622,-2.52850415334516,4.34653887652167));
#16098=CARTESIAN_POINT('Ctrl Pts',(3.39474723933523,-2.4300750743674,4.34121340411158));
#16099=CARTESIAN_POINT('Ctrl Pts',(3.39483887958286,-2.40008013132228,4.33959252805377));
#16100=CARTESIAN_POINT('Ctrl Pts',(3.39480735688311,-2.3998973457609,4.41540747194623));
#16101=CARTESIAN_POINT('Ctrl Pts',(3.39468219270667,-2.3722256242847,4.41391197361979));
#16102=CARTESIAN_POINT('Ctrl Pts',(3.4127838411683,-2.27616341542302,4.40871187894107));
#16103=CARTESIAN_POINT('Ctrl Pts',(3.55878722400007,-2.16065655916503,4.3998071879101));
#16104=CARTESIAN_POINT('Ctrl Pts',(3.77873474447839,-2.23556893008468,4.38869339885329));
#16105=CARTESIAN_POINT('Ctrl Pts',(3.83508286096032,-2.4609855401145,4.37757960979649));
#16106=CARTESIAN_POINT('Ctrl Pts',(3.67625990251943,-2.63058416437082,4.36646582073969));
#16107=CARTESIAN_POINT('Ctrl Pts',(3.45564722516575,-2.59057499098668,4.3557417747896));
#16108=CARTESIAN_POINT('Ctrl Pts',(3.39470486884463,-2.46081219284274,4.34872232519178));
#16109=CARTESIAN_POINT('Ctrl Pts',(3.39427732444531,-2.39988044480691,4.34540747194623));
#16110=CARTESIAN_POINT('Origin',(3.6,-2.4,5.35459252805377));
#16111=CARTESIAN_POINT('',(3.39465010821578,-2.400176527643,4.48540747194623));
#16112=CARTESIAN_POINT('',(3.39437120606287,-2.39983660975581,4.47959252805377));
#16113=CARTESIAN_POINT('',(3.394525,-2.39999999999999,5.35459252805377));
#16114=CARTESIAN_POINT('Ctrl Pts',(3.39437120606287,-2.39983660975581,4.47959252805376));
#16115=CARTESIAN_POINT('Ctrl Pts',(3.39427673427304,-2.3889667776849,4.47900189367213));
#16116=CARTESIAN_POINT('Ctrl Pts',(3.40000383699504,-2.31001856010007,4.47470666293823));
#16117=CARTESIAN_POINT('Ctrl Pts',(3.50226148839652,-2.17766948860297,4.46670683585206));
#16118=CARTESIAN_POINT('Ctrl Pts',(3.73378446004359,-2.19730463405286,4.45559304679526));
#16119=CARTESIAN_POINT('Ctrl Pts',(3.84285302402677,-2.40246926900864,4.44447925773845));
#16120=CARTESIAN_POINT('Ctrl Pts',(3.72963540924699,-2.60537350906572,4.43336546868165));
#16121=CARTESIAN_POINT('Ctrl Pts',(3.49776113780875,-2.62029753773771,4.42225167962485));
#16122=CARTESIAN_POINT('Ctrl Pts',(3.39915518843152,-2.48716469789757,4.41432736608222));
#16123=CARTESIAN_POINT('Ctrl Pts',(3.3942550445316,-2.40962524613366,4.41010764889186));
#16124=CARTESIAN_POINT('Ctrl Pts',(3.39433274578554,-2.4001497810388,4.40959252805377));
#16125=CARTESIAN_POINT('Ctrl Pts',(3.39465010821578,-2.400176527643,4.48540747194623));
#16126=CARTESIAN_POINT('Ctrl Pts',(3.3950436881435,-2.35213729673001,4.48280621840006));
#16127=CARTESIAN_POINT('Ctrl Pts',(3.43581223913156,-2.23508079066125,4.47650036850162));
#16128=CARTESIAN_POINT('Ctrl Pts',(3.63081864021225,-2.15909778094929,4.46648992225093));
#16129=CARTESIAN_POINT('Ctrl Pts',(3.81910984016012,-2.29524053287965,4.45537613319411));
#16130=CARTESIAN_POINT('Ctrl Pts',(3.80684729577664,-2.52727079162485,4.44426234413733));
#16131=CARTESIAN_POINT('Ctrl Pts',(3.60525512132335,-2.64280869447754,4.4331485550805));
#16132=CARTESIAN_POINT('Ctrl Pts',(3.42662678112532,-2.55045981030713,4.42353026435015));
#16133=CARTESIAN_POINT('Ctrl Pts',(3.39499224504393,-2.44077304866432,4.41761656997206));
#16134=CARTESIAN_POINT('Ctrl Pts',(3.39480735688311,-2.3998973457609,4.41540747194623));
#16135=CARTESIAN_POINT('Origin',(3.6,-2.4,5.35459252805377));
#16136=CARTESIAN_POINT('',(3.39418406677318,-2.39999917227821,4.55540747194623));
#16137=CARTESIAN_POINT('',(3.39484823116951,-2.39995310238382,4.54959252805377));
#16138=CARTESIAN_POINT('',(3.394525,-2.39999999999999,5.35459252805377));
#16139=CARTESIAN_POINT('Ctrl Pts',(3.39484823116951,-2.39995310238382,4.54959252805377));
#16140=CARTESIAN_POINT('Ctrl Pts',(3.3947841219125,-2.36854855723416,4.54789613845241));
#16141=CARTESIAN_POINT('Ctrl Pts',(3.41632348134282,-2.26864576454574,4.54249515249878));
#16142=CARTESIAN_POINT('Ctrl Pts',(3.57178888017207,-2.15877849637109,4.53338957019289));
#16143=CARTESIAN_POINT('Ctrl Pts',(3.78736362800739,-2.2454731342224,4.52227578113608));
#16144=CARTESIAN_POINT('Ctrl Pts',(3.83144232268012,-2.47360796667095,4.51116199207928));
#16145=CARTESIAN_POINT('Ctrl Pts',(3.66367923386702,-2.6343685886554,4.50004820302247));
#16146=CARTESIAN_POINT('Ctrl Pts',(3.44964305628728,-2.58346600654441,4.48952504834731));
#16147=CARTESIAN_POINT('Ctrl Pts',(3.39486928333363,-2.45714489513262,4.4827064900244));
#16148=CARTESIAN_POINT('Ctrl Pts',(3.39437120606287,-2.39983660975581,4.47959252805376));
#16149=CARTESIAN_POINT('Ctrl Pts',(3.39418406845602,-2.39999917228229,4.55540747194623));
#16150=CARTESIAN_POINT('Ctrl Pts',(3.39418406581063,-2.39995488126817,4.55540505953261));
#16151=CARTESIAN_POINT('Ctrl Pts',(3.39420413582033,-2.33189558582108,4.55169805076672));
#16152=CARTESIAN_POINT('Ctrl Pts',(3.46841583417461,-2.19586946879708,4.54428644564855));
#16153=CARTESIAN_POINT('Ctrl Pts',(3.70013762796088,-2.17873969637961,4.53317265659175));
#16154=CARTESIAN_POINT('Ctrl Pts',(3.84020231541317,-2.36413198929513,4.52205886753494));
#16155=CARTESIAN_POINT('Ctrl Pts',(3.7604070991348,-2.58235467884591,4.51094507847814));
#16156=CARTESIAN_POINT('Ctrl Pts',(3.53378944658573,-2.63366606347461,4.49983128942134));
#16157=CARTESIAN_POINT('Ctrl Pts',(3.40663179333208,-2.50914981953724,4.4913187539107));
#16158=CARTESIAN_POINT('Ctrl Pts',(3.39448316809474,-2.42055275737136,4.48651081475233));
#16159=CARTESIAN_POINT('Ctrl Pts',(3.39465010821578,-2.400176527643,4.48540747194623));
#16160=CARTESIAN_POINT('Origin',(3.6,-2.4,5.35459252805377));
#16161=CARTESIAN_POINT('',(3.39465252302706,-2.39982399270837,4.62540747194623));
#16162=CARTESIAN_POINT('',(3.39454319301877,-2.40018789160095,4.61959252805377));
#16163=CARTESIAN_POINT('',(3.394525,-2.39999999999999,5.35459252805377));
#16164=CARTESIAN_POINT('Ctrl Pts',(3.39454319301877,-2.40018789160095,4.61959252805377));
#16165=CARTESIAN_POINT('Ctrl Pts',(3.39501369486734,-2.34850703974388,4.61679038323268));
#16166=CARTESIAN_POINT('Ctrl Pts',(3.44097935155591,-2.22775547868952,4.61028364205933));
#16167=CARTESIAN_POINT('Ctrl Pts',(3.64379902793915,-2.16111650041238,4.60007230453371));
#16168=CARTESIAN_POINT('Ctrl Pts',(3.82445363439269,-2.30724091831967,4.58895851547691));
#16169=CARTESIAN_POINT('Ctrl Pts',(3.79966328381548,-2.53826877567792,4.57784472642011));
#16170=CARTESIAN_POINT('Ctrl Pts',(3.59211886521387,-2.64273765452468,4.5667309373633));
#16171=CARTESIAN_POINT('Ctrl Pts',(3.42236627541046,-2.54299330864641,4.55731353790785));
#16172=CARTESIAN_POINT('Ctrl Pts',(3.39492412449178,-2.43713018689806,4.55160073480468));
#16173=CARTESIAN_POINT('Ctrl Pts',(3.39484823116951,-2.39995310238382,4.54959252805377));
#16174=CARTESIAN_POINT('Ctrl Pts',(3.39465252302706,-2.39982399270837,4.62540747194623));
#16175=CARTESIAN_POINT('Ctrl Pts',(3.39448549072207,-2.37935805029673,4.62429930431288));
#16176=CARTESIAN_POINT('Ctrl Pts',(3.40670160391397,-2.29066952405396,4.61948654032727));
#16177=CARTESIAN_POINT('Ctrl Pts',(3.53409308711521,-2.16624811163355,4.61096917998937));
#16178=CARTESIAN_POINT('Ctrl Pts',(3.76064388390312,-2.21785387995996,4.59985539093258));
#16179=CARTESIAN_POINT('Ctrl Pts',(3.8401555119317,-2.4361800576391,4.58874160187577));
#16180=CARTESIAN_POINT('Ctrl Pts',(3.69985007633495,-2.62139021824623,4.57762781281896));
#16181=CARTESIAN_POINT('Ctrl Pts',(3.4682010273,-2.60396318498582,4.56651643617578));
#16182=CARTESIAN_POINT('Ctrl Pts',(3.39418812817678,-2.46796988817124,4.55910965588488));
#16183=CARTESIAN_POINT('Ctrl Pts',(3.39418406845602,-2.39999917228229,4.55540747194623));
#16184=CARTESIAN_POINT('Origin',(3.6,-2.4,5.35459252805377));
#16185=CARTESIAN_POINT('',(3.39480597714356,-2.40010391086475,4.69540747194623));
#16186=CARTESIAN_POINT('',(3.39421139045774,-2.39993212258527,4.68959252805377));
#16187=CARTESIAN_POINT('',(3.394525,-2.39999999999999,5.35459252805377));
#16188=CARTESIAN_POINT('Ctrl Pts',(3.39421139045774,-2.39993212258527,4.68959252805377));
#16189=CARTESIAN_POINT('Ctrl Pts',(3.39419531835948,-2.39619821368606,4.68938922436523));
#16190=CARTESIAN_POINT('Ctrl Pts',(3.3959796089401,-2.32444075084805,4.68548132432442));
#16191=CARTESIAN_POINT('Ctrl Pts',(3.47964553863801,-2.18905336016944,4.67786882793135));
#16192=CARTESIAN_POINT('Ctrl Pts',(3.71195459122784,-2.18447772567898,4.66675503887453));
#16193=CARTESIAN_POINT('Ctrl Pts',(3.84179033681535,-2.37717207306315,4.65564124981774));
#16194=CARTESIAN_POINT('Ctrl Pts',(3.75031264502696,-2.59076108085938,4.64452746076093));
#16195=CARTESIAN_POINT('Ctrl Pts',(3.52125208458385,-2.6297443079663,4.63341367170413));
#16196=CARTESIAN_POINT('Ctrl Pts',(3.40385053605922,-2.50163131684181,4.6251020274684));
#16197=CARTESIAN_POINT('Ctrl Pts',(3.39439166440737,-2.4168320934068,4.62049497958495));
#16198=CARTESIAN_POINT('Ctrl Pts',(3.39454319301877,-2.40018789160095,4.61959252805377));
#16199=CARTESIAN_POINT('Ctrl Pts',(3.39480597714356,-2.40010391086475,4.69540747194623));
#16200=CARTESIAN_POINT('Ctrl Pts',(3.39499357523214,-2.35913959871511,4.69319354909316));
#16201=CARTESIAN_POINT('Ctrl Pts',(3.42673278397032,-2.24936123585863,4.68727502988782));
#16202=CARTESIAN_POINT('Ctrl Pts',(3.60557055480924,-2.15719836203143,4.6776519143302));
#16203=CARTESIAN_POINT('Ctrl Pts',(3.8070124874506,-2.27299804520947,4.6665381252734));
#16204=CARTESIAN_POINT('Ctrl Pts',(3.81897354264718,-2.50504405790744,4.65542433621659));
#16205=CARTESIAN_POINT('Ctrl Pts',(3.63050563092984,-2.64094205312202,4.64431054715979));
#16206=CARTESIAN_POINT('Ctrl Pts',(3.4356920506335,-2.56474249848871,4.63430492573633));
#16207=CARTESIAN_POINT('Ctrl Pts',(3.39504387850492,-2.44777554718273,4.62800390066515));
#16208=CARTESIAN_POINT('Ctrl Pts',(3.39465252302706,-2.39982399270837,4.62540747194623));
#16209=CARTESIAN_POINT('Origin',(3.6,-2.4,5.35459252805377));
#16210=CARTESIAN_POINT('',(3.39427330737243,-2.40012021866021,4.76540747194624));
#16211=CARTESIAN_POINT('',(3.39474358824326,-2.39985490132356,4.75959252805377));
#16212=CARTESIAN_POINT('',(3.394525,-2.39999999999999,5.35459252805377));
#16213=CARTESIAN_POINT('Ctrl Pts',(3.39474358824326,-2.39985490132356,4.75959252805377));
#16214=CARTESIAN_POINT('Ctrl Pts',(3.39458577609892,-2.37565177668507,4.75828346914551));
#16215=CARTESIAN_POINT('Ctrl Pts',(3.40973684003147,-2.28314575562072,4.75326981388497));
#16216=CARTESIAN_POINT('Ctrl Pts',(3.546828337511,-2.16302646659663,4.74455156227216));
#16217=CARTESIAN_POINT('Ctrl Pts',(3.77025746015408,-2.22680624004484,4.73343777321537));
#16218=CARTESIAN_POINT('Ctrl Pts',(3.83784799866721,-2.44911222613084,4.72232398415856));
#16219=CARTESIAN_POINT('Ctrl Pts',(3.68773356662048,-2.62646523466876,4.71121019510175));
#16220=CARTESIAN_POINT('Ctrl Pts',(3.46153062411222,-2.59707961114918,4.7002997097335));
#16221=CARTESIAN_POINT('Ctrl Pts',(3.3944881838605,-2.46423743809455,4.6930938207175));
#16222=CARTESIAN_POINT('Ctrl Pts',(3.39421139045774,-2.39993212258527,4.68959252805377));
#16223=CARTESIAN_POINT('Ctrl Pts',(3.39427330737243,-2.40012021866021,4.76540747194624));
#16224=CARTESIAN_POINT('Ctrl Pts',(3.39469744970711,-2.3391019374956,4.76208779387343));
#16225=CARTESIAN_POINT('Ctrl Pts',(3.45579878082125,-2.20925256261312,4.75506351944836));
#16226=CARTESIAN_POINT('Ctrl Pts',(3.67655777933124,-2.16951665373617,4.74433464867103));
#16227=CARTESIAN_POINT('Ctrl Pts',(3.83516271561975,-2.33931916560024,4.73322085961422));
#16228=CARTESIAN_POINT('Ctrl Pts',(3.77852055137491,-2.56466353335787,4.72210707055742));
#16229=CARTESIAN_POINT('Ctrl Pts',(3.55847650189588,-2.63928950162157,4.71099328150062));
#16230=CARTESIAN_POINT('Ctrl Pts',(3.41270209403565,-2.52365597038275,4.70209341529688));
#16231=CARTESIAN_POINT('Ctrl Pts',(3.3946796640253,-2.4276859083356,4.69689814544542));
#16232=CARTESIAN_POINT('Ctrl Pts',(3.39480597714356,-2.40010391086475,4.69540747194623));
#16233=CARTESIAN_POINT('Origin',(3.6,-2.4,5.35459252805377));
#16234=CARTESIAN_POINT('',(3.39444175959654,-2.39982008597895,4.83540747194623));
#16235=CARTESIAN_POINT('',(3.39473575570154,-2.40014879661129,4.82959252805377));
#16236=CARTESIAN_POINT('',(3.394525,-2.39999999999999,5.35459252805377));
#16237=CARTESIAN_POINT('Ctrl Pts',(3.39473575570154,-2.40014879661129,4.82959252805377));
#16238=CARTESIAN_POINT('Ctrl Pts',(3.39503502367394,-2.35550570215801,4.82717771392578));
#16239=CARTESIAN_POINT('Ctrl Pts',(3.43129921618784,-2.24193240937533,4.82105830344552));
#16240=CARTESIAN_POINT('Ctrl Pts',(3.61869057055051,-2.15785470519124,4.81123429661299));
#16241=CARTESIAN_POINT('Ctrl Pts',(3.81357662274397,-2.28437687323548,4.80012050755619));
#16242=CARTESIAN_POINT('Ctrl Pts',(3.81297357001622,-2.51673020046272,4.78900671849938));
#16243=CARTESIAN_POINT('Ctrl Pts',(3.61743339336808,-2.64223905139592,4.77789292944258));
#16244=CARTESIAN_POINT('Ctrl Pts',(3.43084783163214,-2.55735665460818,4.76808819929404));
#16245=CARTESIAN_POINT('Ctrl Pts',(3.39503237960207,-2.44414587323265,4.76198806549777));
#16246=CARTESIAN_POINT('Ctrl Pts',(3.39474358824326,-2.39985490132356,4.75959252805377));
#16247=CARTESIAN_POINT('Ctrl Pts',(3.39444175959654,-2.39982008597895,4.83540747194623));
#16248=CARTESIAN_POINT('Ctrl Pts',(3.39432007222796,-2.3865422800919,4.83468663500598));
#16249=CARTESIAN_POINT('Ctrl Pts',(3.40154215697383,-2.30515767781734,4.83026120171345));
#16250=CARTESIAN_POINT('Ctrl Pts',(3.51011506636152,-2.17438004258061,4.82213117206865));
#16251=CARTESIAN_POINT('Ctrl Pts',(3.74080744720095,-2.20211890112026,4.81101738301186));
#16252=CARTESIAN_POINT('Ctrl Pts',(3.84261717475225,-2.41098057358878,4.79990359395505));
#16253=CARTESIAN_POINT('Ctrl Pts',(3.72235665078693,-2.60979160252334,4.78878980489825));
#16254=CARTESIAN_POINT('Ctrl Pts',(3.49010169673754,-2.61657799846968,4.77767601584144));
#16255=CARTESIAN_POINT('Ctrl Pts',(3.3977657533099,-2.4823139974067,4.76988190485744));
#16256=CARTESIAN_POINT('Ctrl Pts',(3.39422412786341,-2.40719531789781,4.7657923902257));
#16257=CARTESIAN_POINT('Ctrl Pts',(3.39427330737243,-2.40012021866021,4.76540747194624));
#16258=CARTESIAN_POINT('Origin',(3.6,-2.4,5.35459252805377));
#16259=CARTESIAN_POINT('',(3.39485784898994,-2.39999218980985,4.90540747194623));
#16260=CARTESIAN_POINT('',(3.39420666496973,-2.4000617379826,4.89959252805377));
#16261=CARTESIAN_POINT('',(3.394525,-2.39999999999999,5.35459252805377));
#16262=CARTESIAN_POINT('Ctrl Pts',(3.39420666496973,-2.4000617379826,4.89959252805377));
#16263=CARTESIAN_POINT('Ctrl Pts',(3.39446260190468,-2.33540634192885,4.89607195870605));
#16264=CARTESIAN_POINT('Ctrl Pts',(3.46215556821269,-2.20225412189412,4.88884679300607));
#16265=CARTESIAN_POINT('Ctrl Pts',(3.68890791813162,-2.17399322284688,4.87791703095382));
#16266=CARTESIAN_POINT('Ctrl Pts',(3.83809972557463,-2.3521230545377,4.86680324189701));
#16267=CARTESIAN_POINT('Ctrl Pts',(3.76935615396461,-2.57407519737118,4.85568945284021));
#16268=CARTESIAN_POINT('Ctrl Pts',(3.54559897400137,-2.63669433790405,4.8445756637834));
#16269=CARTESIAN_POINT('Ctrl Pts',(3.4094345739418,-2.51613221625325,4.83587668885459));
#16270=CARTESIAN_POINT('Ctrl Pts',(3.39457591295976,-2.42399322794668,4.83088231027805));
#16271=CARTESIAN_POINT('Ctrl Pts',(3.39473575570154,-2.40014879661129,4.82959252805377));
#16272=CARTESIAN_POINT('Ctrl Pts',(3.39485784898994,-2.39999218980985,4.90540747194623));
#16273=CARTESIAN_POINT('Ctrl Pts',(3.3948463830005,-2.36617331876133,4.90358087978625));
#16274=CARTESIAN_POINT('Ctrl Pts',(3.41876410056102,-2.26378009325356,4.898049691274));
#16275=CARTESIAN_POINT('Ctrl Pts',(3.5802619217345,-2.1579378700657,4.88881390640948));
#16276=CARTESIAN_POINT('Ctrl Pts',(3.7926651914697,-2.25213590538246,4.87770011735268));
#16277=CARTESIAN_POINT('Ctrl Pts',(3.8287198264784,-2.48167562339262,4.86658632829587));
#16278=CARTESIAN_POINT('Ctrl Pts',(3.65542461045338,-2.63645671704841,4.85547253923907));
#16279=CARTESIAN_POINT('Ctrl Pts',(3.44592887677019,-2.57880492333736,4.84507958712252));
#16280=CARTESIAN_POINT('Ctrl Pts',(3.39494545996352,-2.45478089066832,4.83839123135824));
#16281=CARTESIAN_POINT('Ctrl Pts',(3.39444175959654,-2.39982008597895,4.83540747194623));
#16282=CARTESIAN_POINT('Origin',(3.6,-2.4,5.35459252805377));
#16283=CARTESIAN_POINT('',(3.39447042869063,-2.40018396912367,4.97540747194623));
#16284=CARTESIAN_POINT('',(3.39455385196002,-2.39981229693528,4.96959252805377));
#16285=CARTESIAN_POINT('',(3.394525,-2.39999999999999,5.35459252805377));
#16286=CARTESIAN_POINT('Ctrl Pts',(3.39455385196002,-2.39981229693529,4.96959252805377));
#16287=CARTESIAN_POINT('Ctrl Pts',(3.39439994110979,-2.38281031884833,4.9686707998386));
#16288=CARTESIAN_POINT('Ctrl Pts',(3.40410690463755,-2.29764758883809,4.96404447527116));
#16289=CARTESIAN_POINT('Ctrl Pts',(3.52244569995759,-2.16985002334435,4.95571355435144));
#16290=CARTESIAN_POINT('Ctrl Pts',(3.75130082069111,-2.21002173048044,4.94459976529465));
#16291=CARTESIAN_POINT('Ctrl Pts',(3.84166858438312,-2.42408270226789,4.93348597623783));
#16292=CARTESIAN_POINT('Ctrl Pts',(3.71083435207858,-2.61610050352316,4.92237218718104));
#16293=CARTESIAN_POINT('Ctrl Pts',(3.47855218037073,-2.61031906317225,4.91125839812423));
#16294=CARTESIAN_POINT('Ctrl Pts',(3.3958002253152,-2.47484313295797,4.90366517841514));
#16295=CARTESIAN_POINT('Ctrl Pts',(3.39419328664854,-2.40344140123838,4.89977655505832));
#16296=CARTESIAN_POINT('Ctrl Pts',(3.39420666496973,-2.4000617379826,4.89959252805377));
#16297=CARTESIAN_POINT('Ctrl Pts',(3.39447042869063,-2.40018396912367,4.97540747194623));
#16298=CARTESIAN_POINT('Ctrl Pts',(3.39496908844141,-2.34615078794508,4.97247512456653));
#16299=CARTESIAN_POINT('Ctrl Pts',(3.44450059908404,-2.22304562253723,4.96583818083456));
#16300=CARTESIAN_POINT('Ctrl Pts',(3.65214584962031,-2.16279865748873,4.9554966407503));
#16301=CARTESIAN_POINT('Ctrl Pts',(3.82756721091734,-2.31516586178242,4.94438285169351));
#16302=CARTESIAN_POINT('Ctrl Pts',(3.79469372311971,-2.54518271468373,4.9332690626367));
#16303=CARTESIAN_POINT('Ctrl Pts',(3.58361486265069,-2.64231218244471,4.9221552735799));
#16304=CARTESIAN_POINT('Ctrl Pts',(3.41976019754822,-2.53813915804107,4.91286807668307));
#16305=CARTESIAN_POINT('Ctrl Pts',(3.39486963770596,-2.43476294104758,4.90728547613852));
#16306=CARTESIAN_POINT('Ctrl Pts',(3.39485784898994,-2.39999218980985,4.90540747194623));
#16307=CARTESIAN_POINT('Origin',(3.6,-2.4,5.35459252805377));
#16308=CARTESIAN_POINT('',(3.39425291505627,-2.39989343747799,5.04540747194623));
#16309=CARTESIAN_POINT('',(3.39484565493551,-2.40005255540929,5.03959252805377));
#16310=CARTESIAN_POINT('',(3.394525,-2.39999999999999,5.35459252805377));
#16311=CARTESIAN_POINT('Ctrl Pts',(3.39484565493551,-2.40005255540928,5.03959252805377));
#16312=CARTESIAN_POINT('Ctrl Pts',(3.39493157796431,-2.36251978536397,5.03756504461887));
#16313=CARTESIAN_POINT('Ctrl Pts',(3.42276239101834,-2.25628891765328,5.03183296483171));
#16314=CARTESIAN_POINT('Ctrl Pts',(3.59337897177386,-2.15722470850713,5.02239628869227));
#16315=CARTESIAN_POINT('Ctrl Pts',(3.8003783179889,-2.26276949623011,5.01128249963547));
#16316=CARTESIAN_POINT('Ctrl Pts',(3.82396911763155,-2.49392292422242,5.00016871057867));
#16317=CARTESIAN_POINT('Ctrl Pts',(3.64255844375993,-2.63910763258347,4.98905492152186));
#16318=CARTESIAN_POINT('Ctrl Pts',(3.44046962807591,-2.57154454308001,4.97886286068022));
#16319=CARTESIAN_POINT('Ctrl Pts',(3.39501853731303,-2.45114441665013,4.97237539619086));
#16320=CARTESIAN_POINT('Ctrl Pts',(3.39455385196002,-2.39981229693529,4.96959252805377));
#16321=CARTESIAN_POINT('Ctrl Pts',(3.39425291505627,-2.39989343747799,5.04540747194623));
#16322=CARTESIAN_POINT('Ctrl Pts',(3.39421423202935,-2.39376493107826,5.04507396569907));
#16323=CARTESIAN_POINT('Ctrl Pts',(3.39724233967252,-2.31959956972988,5.04103586309963));
#16324=CARTESIAN_POINT('Ctrl Pts',(3.48711398605093,-2.18496417501817,5.03329316414794));
#16325=CARTESIAN_POINT('Ctrl Pts',(3.71944061581356,-2.18853461914439,5.02217937509113));
#16326=CARTESIAN_POINT('Ctrl Pts',(3.84244191526684,-2.38566174871763,5.01106558603433));
#16327=CARTESIAN_POINT('Ctrl Pts',(3.74353337026135,-2.59591283022398,4.99995179697752));
#16328=CARTESIAN_POINT('Ctrl Pts',(3.51324710863985,-2.62684268245385,4.98883800792072));
#16329=CARTESIAN_POINT('Ctrl Pts',(3.40217618139952,-2.49676321865199,4.98065656624362));
#16330=CARTESIAN_POINT('Ctrl Pts',(3.3943391040451,-2.41441388913183,4.97617972091879));
#16331=CARTESIAN_POINT('Ctrl Pts',(3.39447042869063,-2.40018396912367,4.97540747194623));
#16332=CARTESIAN_POINT('Origin',(3.6,-2.4,5.35459252805377));
#16333=CARTESIAN_POINT('',(3.39479089893477,-2.39988380139174,5.11540747194623));
#16334=CARTESIAN_POINT('',(3.39436118987868,-2.40016037422423,5.10959252805377));
#16335=CARTESIAN_POINT('',(3.394525,-2.39999999999999,5.35459252805377));
#16336=CARTESIAN_POINT('Ctrl Pts',(3.39436118987868,-2.40016037422423,5.10959252805377));
#16337=CARTESIAN_POINT('Ctrl Pts',(3.39485595410064,-2.34250465429438,5.10645928939914));
#16338=CARTESIAN_POINT('Ctrl Pts',(3.45020483509149,-2.21584694899168,5.09962145439226));
#16339=CARTESIAN_POINT('Ctrl Pts',(3.66489494634582,-2.16596525152154,5.08907902303309));
#16340=CARTESIAN_POINT('Ctrl Pts',(3.83182128201397,-2.32759432498908,5.07796523397629));
#16341=CARTESIAN_POINT('Ctrl Pts',(3.78655899034249,-2.55549738341204,5.06685144491949));
#16342=CARTESIAN_POINT('Ctrl Pts',(3.57053712854092,-2.64107179875281,5.05573765586268));
#16343=CARTESIAN_POINT('Ctrl Pts',(3.4159720352905,-2.53063333972521,5.04665135024078));
#16344=CARTESIAN_POINT('Ctrl Pts',(3.39477458031215,-2.43109926700468,5.04126964097114));
#16345=CARTESIAN_POINT('Ctrl Pts',(3.39484565493551,-2.40005255540928,5.03959252805377));
#16346=CARTESIAN_POINT('Ctrl Pts',(3.39479089893477,-2.39988380139174,5.11540747194623));
#16347=CARTESIAN_POINT('Ctrl Pts',(3.39465312034679,-2.37325776527266,5.11396821047934));
#16348=CARTESIAN_POINT('Ctrl Pts',(3.41183995517004,-2.27826800227929,5.10882435266019));
#16349=CARTESIAN_POINT('Ctrl Pts',(3.55516853033383,-2.16130913937078,5.09997589848876));
#16350=CARTESIAN_POINT('Ctrl Pts',(3.77622352465696,-2.23288041708187,5.08886210943196));
#16351=CARTESIAN_POINT('Ctrl Pts',(3.83598040928192,-2.457419700552,5.07774832037515));
#16352=CARTESIAN_POINT('Ctrl Pts',(3.67974110927284,-2.62940130358481,5.06663453131835));
#16353=CARTESIAN_POINT('Ctrl Pts',(3.45739290427932,-2.59254974530072,5.05585424850871));
#16354=CARTESIAN_POINT('Ctrl Pts',(3.39464392413157,-2.46184054479285,5.04877856205133));
#16355=CARTESIAN_POINT('Ctrl Pts',(3.39425291505627,-2.39989343747799,5.04540747194623));
#16356=CARTESIAN_POINT('Origin',(3.6,-2.4,5.35459252805377));
#16357=CARTESIAN_POINT('',(3.39473290683218,-2.40022967700174,5.18540747194623));
#16358=CARTESIAN_POINT('',(3.39434265963601,-2.39985006386652,5.17959252805377));
#16359=CARTESIAN_POINT('',(3.394525,-2.39999999999999,5.35459252805377));
#16360=CARTESIAN_POINT('',(3.54698297828114,-2.59851743256717,5.2));
#16361=CARTESIAN_POINT('Ctrl Pts',(3.54698297828114,-2.59851743256717,5.2));
#16362=CARTESIAN_POINT('Ctrl Pts',(3.48097120902544,-2.58088801151799,5.19629540364773));
#16363=CARTESIAN_POINT('Ctrl Pts',(3.40750558819668,-2.51127201784738,5.19143122762981));
#16364=CARTESIAN_POINT('Ctrl Pts',(3.39457125535004,-2.42165321144002,5.18656705161189));
#16365=CARTESIAN_POINT('Ctrl Pts',(3.39473290683218,-2.40022967700174,5.18540747194623));
#16366=CARTESIAN_POINT('',(3.65313154707148,-2.59887322485902,5.2));
#16367=CARTESIAN_POINT('Origin',(3.6,-2.4,5.2));
#16368=CARTESIAN_POINT('Ctrl Pts',(3.65313161981587,-2.59887345085171,5.2));
#16369=CARTESIAN_POINT('Ctrl Pts',(3.58867174169549,-2.61600530781671,5.19636770818145));
#16370=CARTESIAN_POINT('Ctrl Pts',(3.45069167513782,-2.58406709125274,5.1895652175327));
#16371=CARTESIAN_POINT('Ctrl Pts',(3.3948280192206,-2.45815906572508,5.18276272688396));
#16372=CARTESIAN_POINT('Ctrl Pts',(3.39434265963601,-2.39985006386652,5.17959252805377));
#16373=CARTESIAN_POINT('Origin',(3.6,2.4,4.7));
#16374=CARTESIAN_POINT('',(3.43324411482341,2.39987855685961,4.38714803633902));
#16375=CARTESIAN_POINT('',(3.43319917606922,2.4000969362753,4.36785196366098));
#16376=CARTESIAN_POINT('',(3.4334,2.4,4.7));
#16377=CARTESIAN_POINT('',(3.43648706727485,2.36807695453719,4.3));
#16378=CARTESIAN_POINT('Ctrl Pts',(3.43319917606922,2.4000969362753,4.36785196366098));
#16379=CARTESIAN_POINT('Ctrl Pts',(3.43315841823699,2.40590556741068,4.36746222055426));
#16380=CARTESIAN_POINT('Ctrl Pts',(3.43343543893775,2.41171030674387,4.36707247744754));
#16381=CARTESIAN_POINT('Ctrl Pts',(3.43404307301465,2.41748025740019,4.36668273434083));
#16382=CARTESIAN_POINT('Ctrl Pts',(3.43981877230484,2.47232494300381,4.36297813798856));
#16383=CARTESIAN_POINT('Ctrl Pts',(3.475465166407,2.52402649519299,4.35927354163629));
#16384=CARTESIAN_POINT('Ctrl Pts',(3.52467802575654,2.54891438715568,4.35556894528402));
#16385=CARTESIAN_POINT('Ctrl Pts',(3.57389088510608,2.57380227911837,4.35186434893175));
#16386=CARTESIAN_POINT('Ctrl Pts',(3.636670209703,2.57187651085455,4.34815975257948));
#16387=CARTESIAN_POINT('Ctrl Pts',(3.68426556342447,2.54403648109996,4.34445515622722));
#16388=CARTESIAN_POINT('Ctrl Pts',(3.73186091714595,2.51619645134536,4.34075055987495));
#16389=CARTESIAN_POINT('Ctrl Pts',(3.76427229999197,2.46244216009999,4.33704596352268));
#16390=CARTESIAN_POINT('Ctrl Pts',(3.76670490932883,2.40733835348838,4.33334136717041));
#16391=CARTESIAN_POINT('Ctrl Pts',(3.76913751866569,2.35223454687676,4.32963677081814));
#16392=CARTESIAN_POINT('Ctrl Pts',(3.74159135449339,2.29578122489891,4.32593217446588));
#16393=CARTESIAN_POINT('Ctrl Pts',(3.69659413605431,2.26388777656513,4.32222757811361));
#16394=CARTESIAN_POINT('Ctrl Pts',(3.65159691761524,2.23199432823136,4.31852298176134));
#16395=CARTESIAN_POINT('Ctrl Pts',(3.5891486449094,2.22466075354166,4.31481838540907));
#16396=CARTESIAN_POINT('Ctrl Pts',(3.53802497534865,2.24508842505152,4.3111137890568));
#16397=CARTESIAN_POINT('Ctrl Pts',(3.4869013057879,2.26551609656139,4.30740919270454));
#16398=CARTESIAN_POINT('Ctrl Pts',(3.44710223937223,2.31370501427082,4.30370459635227));
#16399=CARTESIAN_POINT('Ctrl Pts',(3.43648706727485,2.36807695453719,4.3));
#16400=CARTESIAN_POINT('',(3.5947433343941,2.5668198697629,4.3));
#16401=CARTESIAN_POINT('Origin',(3.6,2.4,4.3));
#16402=CARTESIAN_POINT('',(3.43365448824955,2.39993503013922,4.31714803633902));
#16403=CARTESIAN_POINT('Ctrl Pts',(3.59474333802771,2.56682006235004,4.3));
#16404=CARTESIAN_POINT('Ctrl Pts',(3.54069368762274,2.56504680898901,4.30363229181856));
#16405=CARTESIAN_POINT('Ctrl Pts',(3.48748281235487,2.53457817870515,4.30726458363711));
#16406=CARTESIAN_POINT('Ctrl Pts',(3.45871386452964,2.48878411340601,4.31089687545566));
#16407=CARTESIAN_POINT('Ctrl Pts',(3.44221011333674,2.46251364065879,4.31298059575012));
#16408=CARTESIAN_POINT('Ctrl Pts',(3.43375000591375,2.43119968923457,4.31506431604457));
#16409=CARTESIAN_POINT('Ctrl Pts',(3.43365448824955,2.39993503013922,4.31714803633902));
#16410=CARTESIAN_POINT('',(3.4334,2.4,4.2));
#16411=CARTESIAN_POINT('',(3.4334,2.4,4.7));
#16412=CARTESIAN_POINT('Origin',(3.6,2.4,4.2));
#16413=CARTESIAN_POINT('Ctrl Pts',(3.43365448824955,2.39993503013922,4.31714803633902));
#16414=CARTESIAN_POINT('Ctrl Pts',(3.4335801873487,2.37561500142982,4.31876891239684));
#16415=CARTESIAN_POINT('Ctrl Pts',(3.43856722533918,2.35132479907035,4.32038978845465));
#16416=CARTESIAN_POINT('Ctrl Pts',(3.44876666696164,2.32946151839122,4.32201066451247));
#16417=CARTESIAN_POINT('Ctrl Pts',(3.47207802013238,2.27949185571287,4.32571526086474));
#16418=CARTESIAN_POINT('Ctrl Pts',(3.52261765366037,2.24219981905568,4.32941985721701));
#16419=CARTESIAN_POINT('Ctrl Pts',(3.57725038766107,2.23467802743392,4.33312445356927));
#16420=CARTESIAN_POINT('Ctrl Pts',(3.63188312166177,2.22715623581217,4.33682904992154));
#16421=CARTESIAN_POINT('Ctrl Pts',(3.69060895613519,2.24940468922586,4.34053364627381));
#16422=CARTESIAN_POINT('Ctrl Pts',(3.72655438764877,2.29122842499976,4.34423824262608));
#16423=CARTESIAN_POINT('Ctrl Pts',(3.76249981916235,2.33305216077365,4.34794283897835));
#16424=CARTESIAN_POINT('Ctrl Pts',(3.77566484771609,2.39445117890775,4.35164743533062));
#16425=CARTESIAN_POINT('Ctrl Pts',(3.76002307153489,2.44733227776831,4.35535203168288));
#16426=CARTESIAN_POINT('Ctrl Pts',(3.7443812953537,2.50021337662887,4.35905662803515));
#16427=CARTESIAN_POINT('Ctrl Pts',(3.69993271443756,2.5445765562159,4.36276122438742));
#16428=CARTESIAN_POINT('Ctrl Pts',(3.64702014888419,2.56011555645441,4.36646582073968));
#16429=CARTESIAN_POINT('Ctrl Pts',(3.59410758333083,2.57565455669293,4.37017041709195));
#16430=CARTESIAN_POINT('Ctrl Pts',(3.53273103314024,2.56236937758293,4.37387501344422));
#16431=CARTESIAN_POINT('Ctrl Pts',(3.49097948747713,2.52634165427837,4.37757960979649));
#16432=CARTESIAN_POINT('Ctrl Pts',(3.45503345721934,2.49532355395523,4.38076908531067));
#16433=CARTESIAN_POINT('Ctrl Pts',(3.43363419524109,2.44744785138174,4.38395856082484));
#16434=CARTESIAN_POINT('Ctrl Pts',(3.43324411482341,2.39987855685961,4.38714803633902));
#16435=CARTESIAN_POINT('Origin',(3.6,2.4,4.7));
#16436=CARTESIAN_POINT('',(3.43327529856389,2.40013247750357,4.45714803633902));
#16437=CARTESIAN_POINT('',(3.43362892985438,2.40008323250784,4.43785196366098));
#16438=CARTESIAN_POINT('',(3.4334,2.4,4.7));
#16439=CARTESIAN_POINT('Ctrl Pts',(3.43362892985438,2.40008323250784,4.43785196366098));
#16440=CARTESIAN_POINT('Ctrl Pts',(3.43352744619908,2.42251958229607,4.43635646533454));
#16441=CARTESIAN_POINT('Ctrl Pts',(3.43774838281902,2.44491933756368,4.43486096700809));
#16442=CARTESIAN_POINT('Ctrl Pts',(3.44647310901037,2.4654005396039,4.43336546868165));
#16443=CARTESIAN_POINT('Ctrl Pts',(3.46808569676891,2.5161358597488,4.42966087232938));
#16444=CARTESIAN_POINT('Ctrl Pts',(3.51733510120548,2.55509827110394,4.42595627597712));
#16445=CARTESIAN_POINT('Ctrl Pts',(3.57168220127168,2.56445626518835,4.42225167962485));
#16446=CARTESIAN_POINT('Ctrl Pts',(3.62602930133789,2.57381425927275,4.41854708327258));
#16447=CARTESIAN_POINT('Ctrl Pts',(3.68547409703373,2.55356783608644,4.41484248692031));
#16448=CARTESIAN_POINT('Ctrl Pts',(3.7228110439026,2.51298316629394,4.41113789056804));
#16449=CARTESIAN_POINT('Ctrl Pts',(3.76014799077148,2.47239849650144,4.40743329421577));
#16450=CARTESIAN_POINT('Ctrl Pts',(3.77537708881339,2.41147558010275,4.4037286978635));
#16451=CARTESIAN_POINT('Ctrl Pts',(3.76152924886074,2.35809557405986,4.40002410151124));
#16452=CARTESIAN_POINT('Ctrl Pts',(3.74768140890809,2.30471556801697,4.39631950515897));
#16453=CARTESIAN_POINT('Ctrl Pts',(3.70475663096088,2.25887847232986,4.3926149088067));
#16454=CARTESIAN_POINT('Ctrl Pts',(3.65239849394634,2.24156301733926,4.38891031245443));
#16455=CARTESIAN_POINT('Ctrl Pts',(3.6000403569318,2.22424756234866,4.38520571610217));
#16456=CARTESIAN_POINT('Ctrl Pts',(3.53824886084993,2.23545374805455,4.3815011197499));
#16457=CARTESIAN_POINT('Ctrl Pts',(3.49530561504809,2.27005075041653,4.37779652339763));
#16458=CARTESIAN_POINT('Ctrl Pts',(3.45688022556308,2.30100796536268,4.37448167015208));
#16459=CARTESIAN_POINT('Ctrl Pts',(3.43354583064794,2.35069321510765,4.37116681690653));
#16460=CARTESIAN_POINT('Ctrl Pts',(3.43319917606922,2.4000969362753,4.36785196366098));
#16461=CARTESIAN_POINT('Ctrl Pts',(3.43324411482341,2.39987855685961,4.38714803633902));
#16462=CARTESIAN_POINT('Ctrl Pts',(3.43318111432356,2.39219580941329,4.38766315717711));
#16463=CARTESIAN_POINT('Ctrl Pts',(3.4336661242569,2.38452105441581,4.3881782780152));
#16464=CARTESIAN_POINT('Ctrl Pts',(3.43472636939645,2.37692660019285,4.38869339885329));
#16465=CARTESIAN_POINT('Ctrl Pts',(3.44235133811452,2.32230953691099,4.39239799520556));
#16466=CARTESIAN_POINT('Ctrl Pts',(3.47972781668628,2.27184567784637,4.39610259155783));
#16467=CARTESIAN_POINT('Ctrl Pts',(3.52975016370933,2.24863049260891,4.3998071879101));
#16468=CARTESIAN_POINT('Ctrl Pts',(3.57977251073239,2.22541530737146,4.40351178426237));
#16469=CARTESIAN_POINT('Ctrl Pts',(3.64244072620675,2.22944879596115,4.40721638061463));
#16470=CARTESIAN_POINT('Ctrl Pts',(3.6890743879353,2.25888481053352,4.4109209769669));
#16471=CARTESIAN_POINT('Ctrl Pts',(3.73570804966386,2.28832082510588,4.41462557331917));
#16472=CARTESIAN_POINT('Ctrl Pts',(3.76630715764661,2.34315936566092,4.41833016967144));
#16473=CARTESIAN_POINT('Ctrl Pts',(3.76686783565003,2.39830336248822,4.4220347660237));
#16474=CARTESIAN_POINT('Ctrl Pts',(3.76742851365345,2.45344735931552,4.42573936237597));
#16475=CARTESIAN_POINT('Ctrl Pts',(3.73795076167754,2.5088968124151,4.42944395872824));
#16476=CARTESIAN_POINT('Ctrl Pts',(3.69192525052887,2.53927491555576,4.43314855508051));
#16477=CARTESIAN_POINT('Ctrl Pts',(3.6458997393802,2.56965301869642,4.43685315143278));
#16478=CARTESIAN_POINT('Ctrl Pts',(3.58332646905877,2.57495977187817,4.44055774778505));
#16479=CARTESIAN_POINT('Ctrl Pts',(3.5328424463163,2.55276653418389,4.44426234413732));
#16480=CARTESIAN_POINT('Ctrl Pts',(3.48235842357382,2.53057329648961,4.44796694048958));
#16481=CARTESIAN_POINT('Ctrl Pts',(3.4439636484103,2.4808800679193,4.45167153684185));
#16482=CARTESIAN_POINT('Ctrl Pts',(3.43522971000183,2.42642922394017,4.45537613319412));
#16483=CARTESIAN_POINT('Ctrl Pts',(3.43383723324577,2.41774797030146,4.45596676757575));
#16484=CARTESIAN_POINT('Ctrl Pts',(3.43319870043454,2.40894578361697,4.45655740195739));
#16485=CARTESIAN_POINT('Ctrl Pts',(3.43327529856389,2.40013247750357,4.45714803633902));
#16486=CARTESIAN_POINT('Origin',(3.6,2.4,4.7));
#16487=CARTESIAN_POINT('',(3.43366207255012,2.4000380247868,4.52714803633902));
#16488=CARTESIAN_POINT('',(3.43350143198867,2.39985687063426,4.50785196366098));
#16489=CARTESIAN_POINT('',(3.4334,2.4,4.7));
#16490=CARTESIAN_POINT('Ctrl Pts',(3.43350143198867,2.39985687063426,4.50785196366098));
#16491=CARTESIAN_POINT('Ctrl Pts',(3.43382054827219,2.43880728393095,4.50525071011481));
#16492=CARTESIAN_POINT('Ctrl Pts',(3.44745633991989,2.47795898515992,4.50264945656865));
#16493=CARTESIAN_POINT('Ctrl Pts',(3.47241574712106,2.50756395301054,4.50004820302248));
#16494=CARTESIAN_POINT('Ctrl Pts',(3.50796188948324,2.54972610827987,4.49634360667021));
#16495=CARTESIAN_POINT('Ctrl Pts',(3.56647488720154,2.57252532742787,4.49263901031794));
#16496=CARTESIAN_POINT('Ctrl Pts',(3.62117593737884,2.56552741635789,4.48893441396567));
#16497=CARTESIAN_POINT('Ctrl Pts',(3.67587698755613,2.55852950528791,4.4852298176134));
#16498=CARTESIAN_POINT('Ctrl Pts',(3.72676609019243,2.52173446399995,4.48152522126113));
#16499=CARTESIAN_POINT('Ctrl Pts',(3.75055355430056,2.47198175613265,4.47782062490887));
#16500=CARTESIAN_POINT('Ctrl Pts',(3.77434101840868,2.42222904826535,4.4741160285566));
#16501=CARTESIAN_POINT('Ctrl Pts',(3.77102684398863,2.3595186738187,4.47041143220433));
#16502=CARTESIAN_POINT('Ctrl Pts',(3.74212779097605,2.31255038253853,4.46670683585206));
#16503=CARTESIAN_POINT('Ctrl Pts',(3.71322873796346,2.26558209125837,4.4630022394998));
#16504=CARTESIAN_POINT('Ctrl Pts',(3.65874480635833,2.23435588314469,4.45929764314753));
#16505=CARTESIAN_POINT('Ctrl Pts',(3.60361085794536,2.23316262684763,4.45559304679526));
#16506=CARTESIAN_POINT('Ctrl Pts',(3.54847690953239,2.23196937055057,4.45188845044299));
#16507=CARTESIAN_POINT('Ctrl Pts',(3.49269294431159,2.26080906607012,4.44818385409072));
#16508=CARTESIAN_POINT('Ctrl Pts',(3.46178884724144,2.30648302829723,4.44447925773845));
#16509=CARTESIAN_POINT('Ctrl Pts',(3.44336034023669,2.33371899416048,4.44227015971263));
#16510=CARTESIAN_POINT('Ctrl Pts',(3.43377883797438,2.36694103826561,4.44006106168681));
#16511=CARTESIAN_POINT('Ctrl Pts',(3.43362892985438,2.40008323250784,4.43785196366098));
#16512=CARTESIAN_POINT('Ctrl Pts',(3.43327529856389,2.40013247750357,4.45714803633902));
#16513=CARTESIAN_POINT('Ctrl Pts',(3.43367914173529,2.35366667577227,4.46026199830965));
#16514=CARTESIAN_POINT('Ctrl Pts',(3.45396107839716,2.3068917935147,4.46337596028029));
#16515=CARTESIAN_POINT('Ctrl Pts',(3.48843309004669,2.27590093912579,4.46648992225093));
#16516=CARTESIAN_POINT('Ctrl Pts',(3.52944351015346,2.23903195767851,4.47019451860319));
#16517=CARTESIAN_POINT('Ctrl Pts',(3.59053745202041,2.22450245417194,4.47389911495546));
#16518=CARTESIAN_POINT('Ctrl Pts',(3.64375492737657,2.23896193518984,4.47760371130773));
#16519=CARTESIAN_POINT('Ctrl Pts',(3.69697240273272,2.25342141620775,4.48130830765999));
#16520=CARTESIAN_POINT('Ctrl Pts',(3.74231341157808,2.29686988175014,4.48501290401227));
#16521=CARTESIAN_POINT('Ctrl Pts',(3.75902738378866,2.34942289673192,4.48871750036453));
#16522=CARTESIAN_POINT('Ctrl Pts',(3.77574135599923,2.40197591171369,4.4924220967168));
#16523=CARTESIAN_POINT('Ctrl Pts',(3.76382829157503,2.46363347613485,4.49612669306907));
#16524=CARTESIAN_POINT('Ctrl Pts',(3.7287402721637,2.50617765524692,4.49983128942134));
#16525=CARTESIAN_POINT('Ctrl Pts',(3.69365225275236,2.54872183435899,4.5035358857736));
#16526=CARTESIAN_POINT('Ctrl Pts',(3.63538927835389,2.57215262816197,4.50724048212587));
#16527=CARTESIAN_POINT('Ctrl Pts',(3.58061572949426,2.56574680139426,4.51094507847814));
#16528=CARTESIAN_POINT('Ctrl Pts',(3.52584218063463,2.55934097462656,4.51464967483041));
#16529=CARTESIAN_POINT('Ctrl Pts',(3.47455805731385,2.52309852728818,4.51835427118268));
#16530=CARTESIAN_POINT('Ctrl Pts',(3.45023382941089,2.47360602072044,4.52205886753494));
#16531=CARTESIAN_POINT('Ctrl Pts',(3.43909540477512,2.45094266808951,4.5237552571363));
#16532=CARTESIAN_POINT('Ctrl Pts',(3.43361009249165,2.42550096367579,4.52545164673766));
#16533=CARTESIAN_POINT('Ctrl Pts',(3.43366207255012,2.4000380247868,4.52714803633902));
#16534=CARTESIAN_POINT('Origin',(3.6,2.4,4.7));
#16535=CARTESIAN_POINT('',(3.43341474631901,2.39984765669014,4.59714803633902));
#16536=CARTESIAN_POINT('',(3.43312356359968,2.40000067112034,4.57785196366098));
#16537=CARTESIAN_POINT('',(3.4334,2.4,4.7));
#16538=CARTESIAN_POINT('Ctrl Pts',(3.43312356496403,2.40000067111703,4.57785196366098));
#16539=CARTESIAN_POINT('Ctrl Pts',(3.43312026903532,2.45518344011976,4.57414495489509));
#16540=CARTESIAN_POINT('Ctrl Pts',(3.46320502523792,2.51036311996034,4.5704379461292));
#16541=CARTESIAN_POINT('Ctrl Pts',(3.50958660620738,2.54026105638185,4.5667309373633));
#16542=CARTESIAN_POINT('Ctrl Pts',(3.55593800339121,2.57013953609479,4.56302634101103));
#16543=CARTESIAN_POINT('Ctrl Pts',(3.6185650095987,2.57476916693782,4.55932174465876));
#16544=CARTESIAN_POINT('Ctrl Pts',(3.66880602035543,2.55203117207009,4.55561714830649));
#16545=CARTESIAN_POINT('Ctrl Pts',(3.71904703111215,2.52929317720236,4.55191255195423));
#16546=CARTESIAN_POINT('Ctrl Pts',(3.7569020464181,2.47918755662387,4.54820795560196));
#16547=CARTESIAN_POINT('Ctrl Pts',(3.76504650379449,2.42464543177811,4.54450335924969));
#16548=CARTESIAN_POINT('Ctrl Pts',(3.77319096117088,2.37010330693235,4.54079876289743));
#16549=CARTESIAN_POINT('Ctrl Pts',(3.75162486061771,2.31112467781931,4.53709416654516));
#16550=CARTESIAN_POINT('Ctrl Pts',(3.71021805048437,2.27470144834891,4.53338957019289));
#16551=CARTESIAN_POINT('Ctrl Pts',(3.66881124035102,2.23827821887852,4.52968497384062));
#16552=CARTESIAN_POINT('Ctrl Pts',(3.60756372063751,2.22441038905077,4.52598037748835));
#16553=CARTESIAN_POINT('Ctrl Pts',(3.55450576575121,2.23944465009304,4.52227578113609));
#16554=CARTESIAN_POINT('Ctrl Pts',(3.50144781086492,2.25447891113532,4.51857118478382));
#16555=CARTESIAN_POINT('Ctrl Pts',(3.45657942080584,2.29841526304761,4.51486658843155));
#16556=CARTESIAN_POINT('Ctrl Pts',(3.44043486927933,2.35114598469909,4.51116199207928));
#16557=CARTESIAN_POINT('Ctrl Pts',(3.43562652497117,2.36685081644385,4.51005864927318));
#16558=CARTESIAN_POINT('Ctrl Pts',(3.43336607622673,2.38333573667221,4.50895530646708));
#16559=CARTESIAN_POINT('Ctrl Pts',(3.43350143198867,2.39985687063426,4.50785196366098));
#16560=CARTESIAN_POINT('Ctrl Pts',(3.43366207255012,2.4000380247868,4.52714803633902));
#16561=CARTESIAN_POINT('Ctrl Pts',(3.43372360717887,2.36989468640869,4.52915624308993));
#16562=CARTESIAN_POINT('Ctrl Pts',(3.44154516635149,2.33972158979514,4.53116444984084));
#16563=CARTESIAN_POINT('Ctrl Pts',(3.45693460375181,2.31409281443648,4.53317265659175));
#16564=CARTESIAN_POINT('Ctrl Pts',(3.48532393848085,2.26681468051736,4.53687725294402));
#16565=CARTESIAN_POINT('Ctrl Pts',(3.53946694042407,2.23500097847622,4.54058184929629));
#16566=CARTESIAN_POINT('Ctrl Pts',(3.59458475774056,2.23321142940033,4.54428644564855));
#16567=CARTESIAN_POINT('Ctrl Pts',(3.64970257505705,2.23142188032444,4.54799104200082));
#16568=CARTESIAN_POINT('Ctrl Pts',(3.7057952077468,2.25965648421381,4.55169563835309));
#16569=CARTESIAN_POINT('Ctrl Pts',(3.73719154438744,2.30499351452124,4.55540023470536));
#16570=CARTESIAN_POINT('Ctrl Pts',(3.76858788102808,2.35033054482868,4.55910483105763));
#16571=CARTESIAN_POINT('Ctrl Pts',(3.77528792161962,2.41277000155418,4.56280942740989));
#16572=CARTESIAN_POINT('Ctrl Pts',(3.75422535459604,2.4637361132596,4.56651402376216));
#16573=CARTESIAN_POINT('Ctrl Pts',(3.73316278757246,2.51470222496502,4.57021862011443));
#16574=CARTESIAN_POINT('Ctrl Pts',(3.68433761293377,2.55419499165036,4.5739232164667));
#16575=CARTESIAN_POINT('Ctrl Pts',(3.63009494870967,2.56414032470881,4.57762781281897));
#16576=CARTESIAN_POINT('Ctrl Pts',(3.57585228448556,2.57408565776726,4.58133240917124));
#16577=CARTESIAN_POINT('Ctrl Pts',(3.51619213067606,2.55448355719882,4.5850370055235));
#16578=CARTESIAN_POINT('Ctrl Pts',(3.47841829496877,2.51430503547713,4.58874160187577));
#16579=CARTESIAN_POINT('Ctrl Pts',(3.44984628656769,2.48391413027303,4.59154374669685));
#16580=CARTESIAN_POINT('Ctrl Pts',(3.43379623122065,2.44175071136891,4.59434589151794));
#16581=CARTESIAN_POINT('Ctrl Pts',(3.43341474631901,2.39984765669014,4.59714803633902));
#16582=CARTESIAN_POINT('Origin',(3.6,2.4,4.7));
#16583=CARTESIAN_POINT('',(3.43314571939013,2.4000550352968,4.66714803633902));
#16584=CARTESIAN_POINT('',(3.43350338992805,2.40014270746267,4.64785196366098));
#16585=CARTESIAN_POINT('',(3.4334,2.4,4.7));
#16586=CARTESIAN_POINT('Ctrl Pts',(3.43350338992805,2.40014270746267,4.64785196366098));
#16587=CARTESIAN_POINT('Ctrl Pts',(3.43336795942281,2.41673658085083,4.64674379602763));
#16588=CARTESIAN_POINT('Ctrl Pts',(3.43564861639563,2.43329406542932,4.64563562839428));
#16589=CARTESIAN_POINT('Ctrl Pts',(3.44049847652216,2.44906128539828,4.64452746076093));
#16590=CARTESIAN_POINT('Ctrl Pts',(3.45671152371201,2.5017709872742,4.64082286440866));
#16591=CARTESIAN_POINT('Ctrl Pts',(3.5016369588364,2.54564900761994,4.63711826805639));
#16592=CARTESIAN_POINT('Ctrl Pts',(3.55471440176584,2.56061432161925,4.63341367170412));
#16593=CARTESIAN_POINT('Ctrl Pts',(3.60779184469527,2.57557963561855,4.62970907535186));
#16594=CARTESIAN_POINT('Ctrl Pts',(3.66902129542974,2.56163224327142,4.62600447899959));
#16595=CARTESIAN_POINT('Ctrl Pts',(3.71038074864658,2.52515524777208,4.62229988264732));
#16596=CARTESIAN_POINT('Ctrl Pts',(3.75174020186341,2.48867825227274,4.61859528629505));
#16597=CARTESIAN_POINT('Ctrl Pts',(3.77322965756262,2.42967165362121,4.61489068994278));
#16598=CARTESIAN_POINT('Ctrl Pts',(3.76501434448883,2.37514015628156,4.61118609359052));
#16599=CARTESIAN_POINT('Ctrl Pts',(3.75679903141505,2.32060865894192,4.60748149723825));
#16600=CARTESIAN_POINT('Ctrl Pts',(3.71887894956827,2.27055226291416,4.60377690088598));
#16601=CARTESIAN_POINT('Ctrl Pts',(3.6686084394294,2.24787956167738,4.60007230453371));
#16602=CARTESIAN_POINT('Ctrl Pts',(3.61833792929053,2.22520686044059,4.59636770818145));
#16603=CARTESIAN_POINT('Ctrl Pts',(3.55571699085956,2.22991785399477,4.59266311182918));
#16604=CARTESIAN_POINT('Ctrl Pts',(3.50940445168984,2.2598565294309,4.58895851547691));
#16605=CARTESIAN_POINT('Ctrl Pts',(3.46312207100161,2.28977570895933,4.58525633153827));
#16606=CARTESIAN_POINT('Ctrl Pts',(3.43312685660295,2.34488972480058,4.58155414759962));
#16607=CARTESIAN_POINT('Ctrl Pts',(3.43312356496403,2.40000067111703,4.57785196366098));
#16608=CARTESIAN_POINT('Ctrl Pts',(3.43341474631901,2.39984765669014,4.59714803633902));
#16609=CARTESIAN_POINT('Ctrl Pts',(3.43329188627587,2.38635246701557,4.59805048787021));
#16610=CARTESIAN_POINT('Ctrl Pts',(3.43479418574107,2.37288428257405,4.59895293940139));
#16611=CARTESIAN_POINT('Ctrl Pts',(3.43802675467359,2.35984505096448,4.59985539093258));
#16612=CARTESIAN_POINT('Ctrl Pts',(3.45129656769075,2.30631853104845,4.60355998728484));
#16613=CARTESIAN_POINT('Ctrl Pts',(3.49372371133013,2.26002043409134,4.60726458363711));
#16614=CARTESIAN_POINT('Ctrl Pts',(3.54589116272705,2.24213934669288,4.61096917998938));
#16615=CARTESIAN_POINT('Ctrl Pts',(3.59805861412397,2.22425825929442,4.61467377634164));
#16616=CARTESIAN_POINT('Ctrl Pts',(3.65996637327845,2.23479418145462,4.61837837269391));
#16617=CARTESIAN_POINT('Ctrl Pts',(3.70328200317247,2.26892528865449,4.62208296904618));
#16618=CARTESIAN_POINT('Ctrl Pts',(3.7465976330665,2.30305639585435,4.62578756539845));
#16619=CARTESIAN_POINT('Ctrl Pts',(3.77132113370008,2.3607826880939,4.62949216175072));
#16620=CARTESIAN_POINT('Ctrl Pts',(3.76613765481651,2.41568540039916,4.63319675810299));
#16621=CARTESIAN_POINT('Ctrl Pts',(3.76095417593294,2.47058811270442,4.63690135445526));
#16622=CARTESIAN_POINT('Ctrl Pts',(3.72586371753223,2.5226672450754,4.64060595080753));
#16623=CARTESIAN_POINT('Ctrl Pts',(3.67692562687786,2.54808848727385,4.64431054715979));
#16624=CARTESIAN_POINT('Ctrl Pts',(3.6279875362235,2.5735097294723,4.64801514351206));
#16625=CARTESIAN_POINT('Ctrl Pts',(3.56520181331549,2.57227308149821,4.65171973986433));
#16626=CARTESIAN_POINT('Ctrl Pts',(3.51730270026196,2.54494450230916,4.65542433621659));
#16627=CARTESIAN_POINT('Ctrl Pts',(3.46940358720842,2.51761592312011,4.65912893256886));
#16628=CARTESIAN_POINT('Ctrl Pts',(3.43639108400936,2.46419541271609,4.66283352892113));
#16629=CARTESIAN_POINT('Ctrl Pts',(3.43337354994745,2.40913117059842,4.6665381252734));
#16630=CARTESIAN_POINT('Ctrl Pts',(3.43320795139183,2.40610931275893,4.66674142896194));
#16631=CARTESIAN_POINT('Ctrl Pts',(3.43313268806444,2.40308250452664,4.66694473265048));
#16632=CARTESIAN_POINT('Ctrl Pts',(3.43314571939013,2.4000550352968,4.66714803633902));
#16633=CARTESIAN_POINT('Origin',(3.6,2.4,4.7));
#16634=CARTESIAN_POINT('',(3.43357722762007,2.40011764662452,4.73714803633902));
#16635=CARTESIAN_POINT('',(3.43362781118013,2.39991574862771,4.71785196366098));
#16636=CARTESIAN_POINT('',(3.4334,2.4,4.7));
#16637=CARTESIAN_POINT('Ctrl Pts',(3.43362781118013,2.39991574862771,4.71785196366098));
#16638=CARTESIAN_POINT('Ctrl Pts',(3.4337799165104,2.43312978761853,4.71563804080791));
#16639=CARTESIAN_POINT('Ctrl Pts',(3.44340626416077,2.46642503117871,4.71342411795483));
#16640=CARTESIAN_POINT('Ctrl Pts',(3.46191047388993,2.49369647002616,4.71121019510175));
#16641=CARTESIAN_POINT('Ctrl Pts',(3.49287389602047,2.5393302520412,4.70750559874949));
#16642=CARTESIAN_POINT('Ctrl Pts',(3.54869526280824,2.56809742778931,4.70380100239722));
#16643=CARTESIAN_POINT('Ctrl Pts',(3.60382760921412,2.56683253616837,4.70009640604495));
#16644=CARTESIAN_POINT('Ctrl Pts',(3.65895995562,2.56556764454744,4.69639180969268));
#16645=CARTESIAN_POINT('Ctrl Pts',(3.71340328164399,2.53427068555747,4.69268721334041));
#16646=CARTESIAN_POINT('Ctrl Pts',(3.74224129041658,2.48726488994604,4.68898261698815));
#16647=CARTESIAN_POINT('Ctrl Pts',(3.77107929918916,2.44025909433461,4.68527802063588));
#16648=CARTESIAN_POINT('Ctrl Pts',(3.77431199071034,2.37754446210172,4.68157342428361));
#16649=CARTESIAN_POINT('Ctrl Pts',(3.75045990537481,2.32782270030492,4.67786882793134));
#16650=CARTESIAN_POINT('Ctrl Pts',(3.72660782003928,2.27810093850813,4.67416423157907));
#16651=CARTESIAN_POINT('Ctrl Pts',(3.67567095784705,2.24137204714742,4.6704596352268));
#16652=CARTESIAN_POINT('Ctrl Pts',(3.62096086261208,2.23444521162098,4.66675503887454));
#16653=CARTESIAN_POINT('Ctrl Pts',(3.56625076737711,2.22751837609454,4.66305044252227));
#16654=CARTESIAN_POINT('Ctrl Pts',(3.5077674390994,2.25039359640236,4.65934584617));
#16655=CARTESIAN_POINT('Ctrl Pts',(3.4722761045882,2.29260189825932,4.65564124981774));
#16656=CARTESIAN_POINT('Ctrl Pts',(3.44740140531328,2.32218429717603,4.65304482109882));
#16657=CARTESIAN_POINT('Ctrl Pts',(3.43382070261849,2.36126338259659,4.6504483923799));
#16658=CARTESIAN_POINT('Ctrl Pts',(3.43350338992805,2.40014270746267,4.64785196366098));
#16659=CARTESIAN_POINT('Ctrl Pts',(3.43314571939013,2.4000550352968,4.66714803633902));
#16660=CARTESIAN_POINT('Ctrl Pts',(3.43337014465933,2.34791601174949,4.67064932900275));
#16661=CARTESIAN_POINT('Ctrl Pts',(3.45978247246013,2.29558093851357,4.67415062166648));
#16662=CARTESIAN_POINT('Ctrl Pts',(3.50195947903851,2.26495997488444,4.67765191433021));
#16663=CARTESIAN_POINT('Ctrl Pts',(3.54658550711625,2.23256099511944,4.68135651068247));
#16664=CARTESIAN_POINT('Ctrl Pts',(3.60886012819649,2.22447100942077,4.68506110703474));
#16665=CARTESIAN_POINT('Ctrl Pts',(3.66028300882075,2.24439244561677,4.68876570338701));
#16666=CARTESIAN_POINT('Ctrl Pts',(3.71170588944501,2.26431388181277,4.69247029973928));
#16667=CARTESIAN_POINT('Ctrl Pts',(3.75227702961328,2.31224673990343,4.69617489609154));
#16668=CARTESIAN_POINT('Ctrl Pts',(3.76342881697354,2.36625427558577,4.69987949244381));
#16669=CARTESIAN_POINT('Ctrl Pts',(3.7745806043338,2.42026181126811,4.70358408879608));
#16670=CARTESIAN_POINT('Ctrl Pts',(3.75631303888606,2.48034402454213,4.70728868514835));
#16671=CARTESIAN_POINT('Ctrl Pts',(3.71698637554161,2.51900394981365,4.71099328150062));
#16672=CARTESIAN_POINT('Ctrl Pts',(3.67765971219715,2.55766387508518,4.71469787785288));
#16673=CARTESIAN_POINT('Ctrl Pts',(3.617273950956,2.57490151235421,4.71840247420515));
#16674=CARTESIAN_POINT('Ctrl Pts',(3.5634649778607,2.56282795918052,4.72210707055742));
#16675=CARTESIAN_POINT('Ctrl Pts',(3.50965600476541,2.55075440600683,4.72581166690969));
#16676=CARTESIAN_POINT('Ctrl Pts',(3.46242381981598,2.50936966239043,4.72951626326196));
#16677=CARTESIAN_POINT('Ctrl Pts',(3.44338450027923,2.45761369091481,4.73322085961423));
#16678=CARTESIAN_POINT('Ctrl Pts',(3.43665675223952,2.43932516253718,4.73452991852249));
#16679=CARTESIAN_POINT('Ctrl Pts',(3.43344927286167,2.41974164310833,4.73583897743076));
#16680=CARTESIAN_POINT('Ctrl Pts',(3.43357722762007,2.40011764662452,4.73714803633902));
#16681=CARTESIAN_POINT('Origin',(3.6,2.4,4.7));
#16682=CARTESIAN_POINT('',(3.4335708769619,2.39987935507417,4.80714803633902));
#16683=CARTESIAN_POINT('',(3.43319592025803,2.39990252619761,4.78785196366098));
#16684=CARTESIAN_POINT('',(3.4334,2.4,4.7));
#16685=CARTESIAN_POINT('Ctrl Pts',(3.43319592025803,2.39990252619761,4.78785196366098));
#16686=CARTESIAN_POINT('Ctrl Pts',(3.43353981667182,2.44937640878962,4.78453228558818));
#16687=CARTESIAN_POINT('Ctrl Pts',(3.45695303934336,2.49913297337583,4.78121260751538));
#16688=CARTESIAN_POINT('Ctrl Pts',(3.495475201044,2.5300857875399,4.77789292944258));
#16689=CARTESIAN_POINT('Ctrl Pts',(3.5384640260409,2.56462759548935,4.77418833309031));
#16690=CARTESIAN_POINT('Ctrl Pts',(3.60026870000874,2.57575223778946,4.77048373673805));
#16691=CARTESIAN_POINT('Ctrl Pts',(3.6526039634498,2.55836845881058,4.76677914038578));
#16692=CARTESIAN_POINT('Ctrl Pts',(3.70493922689085,2.54098467983171,4.76307454403351));
#16693=CARTESIAN_POINT('Ctrl Pts',(3.74780507980512,2.49509247957384,4.75936994768124));
#16694=CARTESIAN_POINT('Ctrl Pts',(3.76158372154047,2.44169468371147,4.75566535132897));
#16695=CARTESIAN_POINT('Ctrl Pts',(3.77536236327582,2.38829688784909,4.7519607549767));
#16696=CARTESIAN_POINT('Ctrl Pts',(3.76005379383226,2.32739349638222,4.74825615862444));
#16697=CARTESIAN_POINT('Ctrl Pts',(3.72266406682112,2.28685729176137,4.74455156227217));
#16698=CARTESIAN_POINT('Ctrl Pts',(3.68527433980998,2.24632108714052,4.7408469659199));
#16699=CARTESIAN_POINT('Ctrl Pts',(3.62580345523126,2.22615206936571,4.73714236956763));
#16700=CARTESIAN_POINT('Ctrl Pts',(3.57146860063526,2.23558070378767,4.73343777321536));
#16701=CARTESIAN_POINT('Ctrl Pts',(3.51713374603927,2.24500933820964,4.72973317686309));
#16702=CARTESIAN_POINT('Ctrl Pts',(3.467934921426,2.28403562482839,4.72602858051083));
#16703=CARTESIAN_POINT('Ctrl Pts',(3.44638824785603,2.33479896227876,4.72232398415856));
#16704=CARTESIAN_POINT('Ctrl Pts',(3.43771819254303,2.35522536091232,4.72083331065937));
#16705=CARTESIAN_POINT('Ctrl Pts',(3.43352539596517,2.37755214744982,4.71934263716017));
#16706=CARTESIAN_POINT('Ctrl Pts',(3.43362781118013,2.39991574862771,4.71785196366098));
#16707=CARTESIAN_POINT('Ctrl Pts',(3.43357722762007,2.40011764662452,4.73714803633902));
#16708=CARTESIAN_POINT('Ctrl Pts',(3.4338113808831,2.36420633806453,4.73954357378302));
#16709=CARTESIAN_POINT('Ctrl Pts',(3.44521519316665,2.32815948046248,4.74193911122703));
#16710=CARTESIAN_POINT('Ctrl Pts',(3.46665596573275,2.29966495797107,4.74433464867103));
#16711=CARTESIAN_POINT('Ctrl Pts',(3.49981320484709,2.25559939583779,4.7480392450233));
#16712=CARTESIAN_POINT('Ctrl Pts',(3.55697413719987,2.22959547090607,4.75174384137556));
#16713=CARTESIAN_POINT('Ctrl Pts',(3.61197873797528,2.23355402687319,4.75544843772783));
#16714=CARTESIAN_POINT('Ctrl Pts',(3.6669833387507,2.2375125828403,4.7591530340801));
#16715=CARTESIAN_POINT('Ctrl Pts',(3.71983160794876,2.27143361970626,4.76285763043237));
#16716=CARTESIAN_POINT('Ctrl Pts',(3.74633723550091,2.31979298260399,4.76656222678464));
#16717=CARTESIAN_POINT('Ctrl Pts',(3.77284286305306,2.36815234550172,4.7702668231369));
#16718=CARTESIAN_POINT('Ctrl Pts',(3.77300584895929,2.43095003443123,4.77397141948917));
#16719=CARTESIAN_POINT('Ctrl Pts',(3.74675160179543,2.47944633096681,4.77767601584144));
#16720=CARTESIAN_POINT('Ctrl Pts',(3.72049735463157,2.52794262750239,4.78138061219371));
#16721=CARTESIAN_POINT('Ctrl Pts',(3.66782587439761,2.56213753164403,4.78508520854598));
#16722=CARTESIAN_POINT('Ctrl Pts',(3.61284256269023,2.56638155161303,4.78878980489825));
#16723=CARTESIAN_POINT('Ctrl Pts',(3.55785925098286,2.57062557158203,4.79249440125052));
#16724=CARTESIAN_POINT('Ctrl Pts',(3.50056410780207,2.54491870737838,4.79619899760278));
#16725=CARTESIAN_POINT('Ctrl Pts',(3.4671785803101,2.50102585117272,4.79990359395505));
#16726=CARTESIAN_POINT('Ctrl Pts',(3.44541646757448,2.47241461280706,4.80231840808304));
#16727=CARTESIAN_POINT('Ctrl Pts',(3.43381352470784,2.43607616609189,4.80473322221103));
#16728=CARTESIAN_POINT('Ctrl Pts',(3.4335708769619,2.39987935507417,4.80714803633902));
#16729=CARTESIAN_POINT('Origin',(3.6,2.4,4.7));
#16730=CARTESIAN_POINT('',(3.43314188794433,2.3999499425809,4.87714803633902));
#16731=CARTESIAN_POINT('',(3.43333250203974,2.40014587505553,4.85785196366098));
#16732=CARTESIAN_POINT('',(3.4334,2.4,4.7));
#16733=CARTESIAN_POINT('Ctrl Pts',(3.43333250203974,2.40014587505553,4.85785196366098));
#16734=CARTESIAN_POINT('Ctrl Pts',(3.43323383740233,2.41091157669441,4.85713112672073));
#16735=CARTESIAN_POINT('Ctrl Pts',(3.43418764294185,2.42165986991066,4.85641028978047));
#16736=CARTESIAN_POINT('Ctrl Pts',(3.43625743346387,2.43218878097762,4.85568945284021));
#16737=CARTESIAN_POINT('Ctrl Pts',(3.44689470520955,2.48629999996998,4.85198485648794));
#16738=CARTESIAN_POINT('Ctrl Pts',(3.48700780884227,2.53461681182183,4.84828026013567));
#16739=CARTESIAN_POINT('Ctrl Pts',(3.53823875502779,2.55502675361418,4.8445756637834));
#16740=CARTESIAN_POINT('Ctrl Pts',(3.58946970121331,2.57543669540653,4.84087106743113));
#16741=CARTESIAN_POINT('Ctrl Pts',(3.65181848995162,2.56793976713939,4.83716647107887));
#16742=CARTESIAN_POINT('Ctrl Pts',(3.69675084453495,2.5359669805447,4.8334618747266));
#16743=CARTESIAN_POINT('Ctrl Pts',(3.74168319911827,2.50399419395,4.82975727837433));
#16744=CARTESIAN_POINT('Ctrl Pts',(3.7691991195466,2.44754554902777,4.82605268202206));
#16745=CARTESIAN_POINT('Ctrl Pts',(3.76670578881005,2.39245508821223,4.8223480856698));
#16746=CARTESIAN_POINT('Ctrl Pts',(3.7642124580735,2.33736462739668,4.81864348931753));
#16747=CARTESIAN_POINT('Ctrl Pts',(3.73170987617206,2.28363235068783,4.81493889296526));
#16748=CARTESIAN_POINT('Ctrl Pts',(3.68407303401509,2.25584913920422,4.811234296613));
#16749=CARTESIAN_POINT('Ctrl Pts',(3.63643619185813,2.2280659277206,4.80752970026073));
#16750=CARTESIAN_POINT('Ctrl Pts',(3.57366508944564,2.22623178146222,4.80382510390846));
#16751=CARTESIAN_POINT('Ctrl Pts',(3.52448727773306,2.25118610786454,4.80012050755619));
#16752=CARTESIAN_POINT('Ctrl Pts',(3.47530946602049,2.27614043426686,4.79641591120392));
#16753=CARTESIAN_POINT('Ctrl Pts',(3.43972494500783,2.32788323332987,4.79271131485165));
#16754=CARTESIAN_POINT('Ctrl Pts',(3.43401917251448,2.38273411966077,4.78900671849938));
#16755=CARTESIAN_POINT('Ctrl Pts',(3.43342632624397,2.38843328545001,4.78862180021992));
#16756=CARTESIAN_POINT('Ctrl Pts',(3.43315604530238,2.39416600556269,4.78823688194045));
#16757=CARTESIAN_POINT('Ctrl Pts',(3.43319592025803,2.39990252619761,4.78785196366098));
#16758=CARTESIAN_POINT('Ctrl Pts',(3.4335708769619,2.39987935507417,4.80714803633902));
#16759=CARTESIAN_POINT('Ctrl Pts',(3.43344127578645,2.38054618864739,4.8084378185633));
#16760=CARTESIAN_POINT('Ctrl Pts',(3.43655249507166,2.36125342749717,4.80972760078758));
#16761=CARTESIAN_POINT('Ctrl Pts',(3.44308754966948,2.34320004344294,4.81101738301185));
#16762=CARTESIAN_POINT('Ctrl Pts',(3.46185795832395,2.2913459401265,4.81472197936412));
#16763=CARTESIAN_POINT('Ctrl Pts',(3.50887468743604,2.24971658170129,4.81842657571639));
#16764=CARTESIAN_POINT('Ctrl Pts',(3.5626202643246,2.23736388010515,4.82213117206866));
#16765=CARTESIAN_POINT('Ctrl Pts',(3.61636584121316,2.22501117850901,4.82583576842092));
#16766=CARTESIAN_POINT('Ctrl Pts',(3.6768402658782,2.24193513374194,4.82954036477319));
#16767=CARTESIAN_POINT('Ctrl Pts',(3.71636707495845,2.28039040172619,4.83324496112546));
#16768=CARTESIAN_POINT('Ctrl Pts',(3.7558938840387,2.31884566971043,4.83694955747773));
#16769=CARTESIAN_POINT('Ctrl Pts',(3.77447307753417,2.378832250446,4.84065415383));
#16770=CARTESIAN_POINT('Ctrl Pts',(3.76360178219044,2.4328969451123,4.84435875018227));
#16771=CARTESIAN_POINT('Ctrl Pts',(3.75273048684672,2.4869616397786,4.84806334653454));
#16772=CARTESIAN_POINT('Ctrl Pts',(3.71240870266382,2.53510444837563,4.8517679428868));
#16773=CARTESIAN_POINT('Ctrl Pts',(3.66108992281312,2.55529254156049,4.85547253923907));
#16774=CARTESIAN_POINT('Ctrl Pts',(3.60977114296242,2.57548063474534,4.85917713559134));
#16775=CARTESIAN_POINT('Ctrl Pts',(3.54745536744392,2.56771401251802,4.86288173194361));
#16776=CARTESIAN_POINT('Ctrl Pts',(3.50266176427811,2.53554711358097,4.86658632829587));
#16777=CARTESIAN_POINT('Ctrl Pts',(3.46009329762648,2.50497811560107,4.87010689764359));
#16778=CARTESIAN_POINT('Ctrl Pts',(3.43334940270065,2.45237281292388,4.87362746699131));
#16779=CARTESIAN_POINT('Ctrl Pts',(3.43314188794433,2.3999499425809,4.87714803633902));
#16780=CARTESIAN_POINT('Origin',(3.6,2.4,4.7));
#16781=CARTESIAN_POINT('',(3.43342338863395,2.40015219044389,4.94714803633902));
#16782=CARTESIAN_POINT('',(3.4336698690944,2.40000633253548,4.92785196366098));
#16783=CARTESIAN_POINT('',(3.4334,2.4,4.7));
#16784=CARTESIAN_POINT('Ctrl Pts',(3.4336698690944,2.40000633253548,4.92785196366098));
#16785=CARTESIAN_POINT('Ctrl Pts',(3.43366057242126,2.42742681740845,4.926025371501));
#16786=CARTESIAN_POINT('Ctrl Pts',(3.44006468394764,2.45484321422969,4.92419877934102));
#16787=CARTESIAN_POINT('Ctrl Pts',(3.4529060499396,2.47881063108511,4.92237218718104));
#16788=CARTESIAN_POINT('Ctrl Pts',(3.47895022041959,2.52742006180595,4.91866759082877));
#16789=CARTESIAN_POINT('Ctrl Pts',(3.53147325119262,2.5618425345377,4.9149629944765));
#16790=CARTESIAN_POINT('Ctrl Pts',(3.58643767940152,2.56632440944362,4.91125839812423));
#16791=CARTESIAN_POINT('Ctrl Pts',(3.64140210761043,2.57080628434953,4.90755380177196));
#16792=CARTESIAN_POINT('Ctrl Pts',(3.6988079332552,2.54534756142961,4.90384920541969));
#16793=CARTESIAN_POINT('Ctrl Pts',(3.73238305471537,2.50159956959011,4.90014460906743));
#16794=CARTESIAN_POINT('Ctrl Pts',(3.76595817617555,2.45785157775061,4.89644001271516));
#16795=CARTESIAN_POINT('Ctrl Pts',(3.77570259345112,2.39581431699153,4.89273541636289));
#16796=CARTESIAN_POINT('Ctrl Pts',(3.75715671872181,2.34387949147388,4.88903082001062));
#16797=CARTESIAN_POINT('Ctrl Pts',(3.7386108439925,2.29194466595622,4.88532622365836));
#16798=CARTESIAN_POINT('Ctrl Pts',(3.6917746772583,2.25011227567998,4.88162162730609));
#16799=CARTESIAN_POINT('Ctrl Pts',(3.638083055804,2.23752715126117,4.87791703095382));
#16800=CARTESIAN_POINT('Ctrl Pts',(3.58439143434971,2.22494202684235,4.87421243460155));
#16801=CARTESIAN_POINT('Ctrl Pts',(3.52384435817533,2.24160416828095,4.87050783824928));
#16802=CARTESIAN_POINT('Ctrl Pts',(3.48415154001745,2.27988805206668,4.86680324189701));
#16803=CARTESIAN_POINT('Ctrl Pts',(3.45218211379499,2.3107226930672,4.863819482485));
#16804=CARTESIAN_POINT('Ctrl Pts',(3.43374090444541,2.35558342022287,4.86083572307299));
#16805=CARTESIAN_POINT('Ctrl Pts',(3.43333250203974,2.40014587505553,4.85785196366098));
#16806=CARTESIAN_POINT('Ctrl Pts',(3.43314188794433,2.3999499425809,4.87714803633902));
#16807=CARTESIAN_POINT('Ctrl Pts',(3.43313104074456,2.39720969722669,4.87733206334358));
#16808=CARTESIAN_POINT('Ctrl Pts',(3.43319270038641,2.39446995034259,4.87751609034813));
#16809=CARTESIAN_POINT('Ctrl Pts',(3.43332839678999,2.39173387533235,4.87770011735268));
#16810=CARTESIAN_POINT('Ctrl Pts',(3.43606006328079,2.33665471166754,4.88140471370495));
#16811=CARTESIAN_POINT('Ctrl Pts',(3.4687948270755,2.28306355998471,4.88510931005722));
#16812=CARTESIAN_POINT('Ctrl Pts',(3.5165514379046,2.2554867147355,4.88881390640948));
#16813=CARTESIAN_POINT('Ctrl Pts',(3.5643080487337,2.2279098694863,4.89251850276175));
#16814=CARTESIAN_POINT('Ctrl Pts',(3.6270865065972,2.22634733067072,4.89622309911402));
#16815=CARTESIAN_POINT('Ctrl Pts',(3.67615589427605,2.25151420303488,4.89992769546629));
#16816=CARTESIAN_POINT('Ctrl Pts',(3.72522528195491,2.27668107539905,4.90363229181856));
#16817=CARTESIAN_POINT('Ctrl Pts',(3.76058559944912,2.32857735894297,4.90733688817082));
#16818=CARTESIAN_POINT('Ctrl Pts',(3.76605399695032,2.38345242523688,4.91104148452309));
#16819=CARTESIAN_POINT('Ctrl Pts',(3.77152239445151,2.43832749153079,4.91474608087536));
#16820=CARTESIAN_POINT('Ctrl Pts',(3.74709887195967,2.4961813405747,4.91845067722763));
#16821=CARTESIAN_POINT('Ctrl Pts',(3.70396099303503,2.53053683028788,4.9221552735799));
#16822=CARTESIAN_POINT('Ctrl Pts',(3.66082311411038,2.56489232000106,4.92585986993216));
#16823=CARTESIAN_POINT('Ctrl Pts',(3.59897087875293,2.57574945038351,4.92956446628443));
#16824=CARTESIAN_POINT('Ctrl Pts',(3.54671131319796,2.55813939417591,4.9332690626367));
#16825=CARTESIAN_POINT('Ctrl Pts',(3.494451747643,2.5405293379683,4.93697365898897));
#16826=CARTESIAN_POINT('Ctrl Pts',(3.45178485189053,2.49445209517064,4.94067825534124));
#16827=CARTESIAN_POINT('Ctrl Pts',(3.43823737272355,2.44099517717631,4.94438285169351));
#16828=CARTESIAN_POINT('Ctrl Pts',(3.43486666978988,2.42769474038747,4.94530457990868));
#16829=CARTESIAN_POINT('Ctrl Pts',(3.43329859706143,2.41393746665015,4.94622630812385));
#16830=CARTESIAN_POINT('Ctrl Pts',(3.43342338863395,2.40015219044389,4.94714803633902));
#16831=CARTESIAN_POINT('Origin',(3.6,2.4,4.7));
#16832=CARTESIAN_POINT('',(3.43365998372879,2.39995738785189,5.01714803633902));
#16833=CARTESIAN_POINT('',(3.43335574706359,2.39985083704977,4.99785196366098));
#16834=CARTESIAN_POINT('',(3.4334,2.4,4.7));
#16835=CARTESIAN_POINT('Ctrl Pts',(3.43335574706359,2.39985083704977,4.99785196366098));
#16836=CARTESIAN_POINT('Ctrl Pts',(3.43376006251615,2.44366117078388,4.99491961628127));
#16837=CARTESIAN_POINT('Ctrl Pts',(3.45150379085869,2.48776127159334,4.99198726890157));
#16838=CARTESIAN_POINT('Ctrl Pts',(3.48249984106631,2.5184966596533,4.98905492152186));
#16839=CARTESIAN_POINT('Ctrl Pts',(3.52165886271855,2.55732637242214,4.98535032516959));
#16840=CARTESIAN_POINT('Ctrl Pts',(3.58196946998821,2.57482511625956,4.98164572881732));
#16841=CARTESIAN_POINT('Ctrl Pts',(3.63583017159909,2.56298449167174,4.97794113246505));
#16842=CARTESIAN_POINT('Ctrl Pts',(3.68969087320997,2.55114386708391,4.97423653611278));
#16843=CARTESIAN_POINT('Ctrl Pts',(3.73710166916209,2.50996387407084,4.97053193976052));
#16844=CARTESIAN_POINT('Ctrl Pts',(3.75636473978792,2.45829077001732,4.96682734340825));
#16845=CARTESIAN_POINT('Ctrl Pts',(3.77562781041376,2.4066176659638,4.96312274705598));
#16846=CARTESIAN_POINT('Ctrl Pts',(3.76674315571332,2.34445145086982,4.95941815070371));
#16847=CARTESIAN_POINT('Ctrl Pts',(3.73377688832091,2.30024284554165,4.95571355435145));
#16848=CARTESIAN_POINT('Ctrl Pts',(3.70081062092849,2.25603424021347,4.95200895799918));
#16849=CARTESIAN_POINT('Ctrl Pts',(3.64376274084411,2.2297832446511,4.94830436164691));
#16850=CARTESIAN_POINT('Ctrl Pts',(3.58874153385625,2.23350377584586,4.94459976529464));
#16851=CARTESIAN_POINT('Ctrl Pts',(3.5337203268684,2.23722430704061,4.94089516894238));
#16852=CARTESIAN_POINT('Ctrl Pts',(3.48072579297707,2.2709163649925,4.93719057259011));
#16853=CARTESIAN_POINT('Ctrl Pts',(3.45401118112487,2.31916058832341,4.93348597623784));
#16854=CARTESIAN_POINT('Ctrl Pts',(3.44046850379027,2.34361746433734,4.93160797204555));
#16855=CARTESIAN_POINT('Ctrl Pts',(3.43367942743562,2.37181405914562,4.92972996785326));
#16856=CARTESIAN_POINT('Ctrl Pts',(3.4336698690944,2.40000633253548,4.92785196366098));
#16857=CARTESIAN_POINT('Ctrl Pts',(3.43342338863395,2.40015219044389,4.94714803633902));
#16858=CARTESIAN_POINT('Ctrl Pts',(3.43380015749623,2.35853188927053,4.94993090447612));
#16859=CARTESIAN_POINT('Ctrl Pts',(3.44960819526551,2.31665633218087,4.95271377261321));
#16860=CARTESIAN_POINT('Ctrl Pts',(3.47782659951237,2.28632760954166,4.95549664075031));
#16861=CARTESIAN_POINT('Ctrl Pts',(3.51539136804964,2.24595355309232,4.95920123710258));
#16862=CARTESIAN_POINT('Ctrl Pts',(3.57494896770565,2.22604203338462,4.96290583345485));
#16863=CARTESIAN_POINT('Ctrl Pts',(3.62924252529985,2.23570567012353,4.96661042980711));
#16864=CARTESIAN_POINT('Ctrl Pts',(3.68353608289404,2.24536930686244,4.97031502615938));
#16865=CARTESIAN_POINT('Ctrl Pts',(3.73256559842641,2.28460810004796,4.97401962251165));
#16866=CARTESIAN_POINT('Ctrl Pts',(3.75389243606413,2.33546419387067,4.97772421886392));
#16867=CARTESIAN_POINT('Ctrl Pts',(3.77521927370186,2.38632028769338,4.98142881521618));
#16868=CARTESIAN_POINT('Ctrl Pts',(3.76884343344493,2.44879368215328,4.98513341156845));
#16869=CARTESIAN_POINT('Ctrl Pts',(3.73768285480685,2.49429307324449,4.98883800792072));
#16870=CARTESIAN_POINT('Ctrl Pts',(3.70652227616876,2.5397924643357,4.99254260427299));
#16871=CARTESIAN_POINT('Ctrl Pts',(3.65057695914952,2.5683178520582,4.99624720062526));
#16872=CARTESIAN_POINT('Ctrl Pts',(3.59545059518146,2.56681443253905,4.99995179697753));
#16873=CARTESIAN_POINT('Ctrl Pts',(3.54032423121339,2.5653110130199,5.00365639332979));
#16874=CARTESIAN_POINT('Ctrl Pts',(3.4860168202965,2.5337787862591,5.00736098968206));
#16875=CARTESIAN_POINT('Ctrl Pts',(3.45738245724731,2.48664865149311,5.01106558603433));
#16876=CARTESIAN_POINT('Ctrl Pts',(3.44171119613527,2.4608548649544,5.01309306946923));
#16877=CARTESIAN_POINT('Ctrl Pts',(3.43372965048622,2.43038911757193,5.01512055290412));
#16878=CARTESIAN_POINT('Ctrl Pts',(3.43365998372879,2.39995738785189,5.01714803633902));
#16879=CARTESIAN_POINT('Origin',(3.6,2.4,4.7));
#16880=CARTESIAN_POINT('',(3.43326717741735,2.39986996798437,5.08714803633902));
#16881=CARTESIAN_POINT('',(3.43317938608394,2.40008640134203,5.06785196366098));
#16882=CARTESIAN_POINT('',(3.4334,2.4,4.7));
#16883=CARTESIAN_POINT('Ctrl Pts',(3.43317938608394,2.40008640134203,5.06785196366098));
#16884=CARTESIAN_POINT('Ctrl Pts',(3.43314802172115,2.40505542046622,5.06751845741382));
#16885=CARTESIAN_POINT('Ctrl Pts',(3.4333507965104,2.41002184414099,5.06718495116665));
#16886=CARTESIAN_POINT('Ctrl Pts',(3.43379604919982,2.41496643290483,5.06685144491949));
#16887=CARTESIAN_POINT('Ctrl Pts',(3.4387419280344,2.46989105771691,5.06314684856722));
#16888=CARTESIAN_POINT('Ctrl Pts',(3.47360673324676,2.52212151084356,5.05944225221496));
#16889=CARTESIAN_POINT('Ctrl Pts',(3.52243437289015,2.54775424884904,5.05573765586269));
#16890=CARTESIAN_POINT('Ctrl Pts',(3.57126201253354,2.57338698685451,5.05203305951042));
#16891=CARTESIAN_POINT('Ctrl Pts',(3.63405248660798,2.57242200973882,5.04832846315815));
#16892=CARTESIAN_POINT('Ctrl Pts',(3.68206938667054,2.54530093495911,5.04462386680588));
#16893=CARTESIAN_POINT('Ctrl Pts',(3.7300862867331,2.51817986017941,5.04091927045361));
#16894=CARTESIAN_POINT('Ctrl Pts',(3.7633296127838,2.4649026877357,5.03721467410135));
#16895=CARTESIAN_POINT('Ctrl Pts',(3.76658536412569,2.40985202258946,5.03351007774908));
#16896=CARTESIAN_POINT('Ctrl Pts',(3.76984111546757,2.35480135744323,5.02980548139681));
#16897=CARTESIAN_POINT('Ctrl Pts',(3.74310929210064,2.29797719959448,5.02610088504454));
#16898=CARTESIAN_POINT('Ctrl Pts',(3.69862386658003,2.26538544465498,5.02239628869227));
#16899=CARTESIAN_POINT('Ctrl Pts',(3.65413844105941,2.23279368971548,5.01869169234));
#16900=CARTESIAN_POINT('Ctrl Pts',(3.59189941338511,2.22443433768522,5.01498709598774));
#16901=CARTESIAN_POINT('Ctrl Pts',(3.54039082648689,2.24413309464159,5.01128249963547));
#16902=CARTESIAN_POINT('Ctrl Pts',(3.48888223958867,2.26383185159795,5.0075779032832));
#16903=CARTESIAN_POINT('Ctrl Pts',(3.44810409346653,2.31158871754094,5.00387330693093));
#16904=CARTESIAN_POINT('Ctrl Pts',(3.43671873842288,2.36554749136257,5.00016871057866));
#16905=CARTESIAN_POINT('Ctrl Pts',(3.43434538167935,2.37679557446855,4.9993964616061));
#16906=CARTESIAN_POINT('Ctrl Pts',(3.43324926848095,2.38831315722103,4.99862421263354));
#16907=CARTESIAN_POINT('Ctrl Pts',(3.43335574706359,2.39985083704977,4.99785196366098));
#16908=CARTESIAN_POINT('Ctrl Pts',(3.43365998372879,2.39995738785189,5.01714803633902));
#16909=CARTESIAN_POINT('Ctrl Pts',(3.43360235612169,2.37478458193251,5.01882514925639));
#16910=CARTESIAN_POINT('Ctrl Pts',(3.43895837147105,2.34963505233992,5.02050226217376));
#16911=CARTESIAN_POINT('Ctrl Pts',(3.44985377385385,2.32717237393524,5.02217937509113));
#16912=CARTESIAN_POINT('Ctrl Pts',(3.47392076869108,2.2775542739145,5.0258839714434));
#16913=CARTESIAN_POINT('Ctrl Pts',(3.52501607354704,2.24104611664418,5.02958856779567));
#16914=CARTESIAN_POINT('Ctrl Pts',(3.57975563349286,2.23435605471958,5.03329316414794));
#16915=CARTESIAN_POINT('Ctrl Pts',(3.63449519343869,2.22766599279499,5.03699776050021));
#16916=CARTESIAN_POINT('Ctrl Pts',(3.69287900847437,2.25079402621613,5.04070235685247));
#16917=CARTESIAN_POINT('Ctrl Pts',(3.72818739245021,2.2931555045654,5.04440695320474));
#16918=CARTESIAN_POINT('Ctrl Pts',(3.76349577642604,2.33551698291468,5.04811154955701));
#16919=CARTESIAN_POINT('Ctrl Pts',(3.77572872934203,2.39711190619209,5.05181614590928));
#16920=CARTESIAN_POINT('Ctrl Pts',(3.75928777521595,2.44975095798197,5.05552074226155));
#16921=CARTESIAN_POINT('Ctrl Pts',(3.74284682108988,2.50239000977184,5.05922533861381));
#16922=CARTESIAN_POINT('Ctrl Pts',(3.69773195992176,2.54607319007419,5.06292993496608));
#16923=CARTESIAN_POINT('Ctrl Pts',(3.64459025516192,2.56080874487665,5.06663453131835));
#16924=CARTESIAN_POINT('Ctrl Pts',(3.59144855040209,2.57554429967911,5.07033912767062));
#16925=CARTESIAN_POINT('Ctrl Pts',(3.53028000205055,2.5613322289817,5.07404372402289));
#16926=CARTESIAN_POINT('Ctrl Pts',(3.48907876029587,2.52467656495583,5.07774832037516));
#16927=CARTESIAN_POINT('Ctrl Pts',(3.45423196161424,2.49367428224656,5.08088155902978));
#16928=CARTESIAN_POINT('Ctrl Pts',(3.43366833435756,2.44661747113372,5.0840147976844));
#16929=CARTESIAN_POINT('Ctrl Pts',(3.43326717741735,2.39986996798437,5.08714803633902));
#16930=CARTESIAN_POINT('Origin',(3.6,2.4,4.7));
#16931=CARTESIAN_POINT('',(3.43325215340634,2.40012157034435,5.15714803633902));
#16932=CARTESIAN_POINT('',(3.43361558566414,2.40009421455432,5.13785196366098));
#16933=CARTESIAN_POINT('',(3.4334,2.4,4.7));
#16934=CARTESIAN_POINT('',(3.72690708798524,2.50793586530485,5.2));
#16935=CARTESIAN_POINT('Ctrl Pts',(3.43325215340634,2.40012157034435,5.15714803633902));
#16936=CARTESIAN_POINT('Ctrl Pts',(3.43364568326786,2.35284438105766,5.16031823516921));
#16937=CARTESIAN_POINT('Ctrl Pts',(3.45475449837728,2.3052683699281,5.1634884339994));
#16938=CARTESIAN_POINT('Ctrl Pts',(3.49032381108024,2.27424021130156,5.16665863282959));
#16939=CARTESIAN_POINT('Ctrl Pts',(3.53188901034701,2.23798166430732,5.17036322918186));
#16940=CARTESIAN_POINT('Ctrl Pts',(3.59320079576331,2.22432009870508,5.17406782553412));
#16941=CARTESIAN_POINT('Ctrl Pts',(3.64619138280368,2.2396150803554,5.17777242188639));
#16942=CARTESIAN_POINT('Ctrl Pts',(3.69918196984405,2.25491006200572,5.18147701823866));
#16943=CARTESIAN_POINT('Ctrl Pts',(3.74385135850849,2.2991615909086,5.18518161459093));
#16944=CARTESIAN_POINT('Ctrl Pts',(3.75975544882264,2.35186813523316,5.1888862109432));
#16945=CARTESIAN_POINT('Ctrl Pts',(3.7756595391368,2.40457467955771,5.19259080729547));
#16946=CARTESIAN_POINT('Ctrl Pts',(3.76279833110066,2.46573623930395,5.19629540364773));
#16947=CARTESIAN_POINT('Ctrl Pts',(3.72690708798524,2.50793586530485,5.2));
#16948=CARTESIAN_POINT('',(3.47285246768952,2.50812032770478,5.2));
#16949=CARTESIAN_POINT('Origin',(3.6,2.4,5.2));
#16950=CARTESIAN_POINT('Ctrl Pts',(3.47285231527688,2.50812044463164,5.2));
#16951=CARTESIAN_POINT('Ctrl Pts',(3.50793811173714,2.54927258268021,5.19636770818145));
#16952=CARTESIAN_POINT('Ctrl Pts',(3.56493587106976,2.57187757629771,5.19273541636289));
#16953=CARTESIAN_POINT('Ctrl Pts',(3.6186762488644,2.56581789998251,5.18910312454433));
#16954=CARTESIAN_POINT('Ctrl Pts',(3.67348638458382,2.55963759952907,5.18539852819207));
#16955=CARTESIAN_POINT('Ctrl Pts',(3.72490816491496,2.52364007082416,5.1816939318398));
#16956=CARTESIAN_POINT('Ctrl Pts',(3.74944162746499,2.4742589593754,5.17798933548753));
#16957=CARTESIAN_POINT('Ctrl Pts',(3.77397509001502,2.42487784792664,5.17428473913527));
#16958=CARTESIAN_POINT('Ctrl Pts',(3.77162023478396,2.36211315373403,5.17058014278299));
#16959=CARTESIAN_POINT('Ctrl Pts',(3.74343805908691,2.31470980295916,5.16687554643072));
#16960=CARTESIAN_POINT('Ctrl Pts',(3.71525588338986,2.2673064521843,5.16317095007846));
#16961=CARTESIAN_POINT('Ctrl Pts',(3.66124638722683,2.23526444482719,5.15946635372619));
#16962=CARTESIAN_POINT('Ctrl Pts',(3.60613566997566,2.23323785031625,5.15576175737392));
#16963=CARTESIAN_POINT('Ctrl Pts',(3.55102495272448,2.23121125580531,5.15205716102166));
#16964=CARTESIAN_POINT('Ctrl Pts',(3.49481301438516,2.25920007414054,5.14835256466939));
#16965=CARTESIAN_POINT('Ctrl Pts',(3.46322139831185,2.30440012642267,5.14464796831712));
#16966=CARTESIAN_POINT('Ctrl Pts',(3.44390334496103,2.33203964380033,5.14238263343174));
#16967=CARTESIAN_POINT('Ctrl Pts',(3.43379141454156,2.36611485011022,5.14011729854636));
#16968=CARTESIAN_POINT('Ctrl Pts',(3.43361558566414,2.40009421455432,5.13785196366098));
#16969=CARTESIAN_POINT('Origin',(3.6,2.4,5.35459252805377));
#16970=CARTESIAN_POINT('',(3.39427731514299,2.4001195557093,4.34540747194623));
#16971=CARTESIAN_POINT('',(3.39483887138702,2.39991986985508,4.33959252805377));
#16972=CARTESIAN_POINT('',(3.394525,2.40000000000001,5.35459252805377));
#16973=CARTESIAN_POINT('',(3.78826275096636,2.31767678198967,4.3));
#16974=CARTESIAN_POINT('Ctrl Pts',(3.39483887138702,2.39991986985508,4.33959252805377));
#16975=CARTESIAN_POINT('Ctrl Pts',(3.39495667746176,2.43847992884438,4.33750880775932));
#16976=CARTESIAN_POINT('Ctrl Pts',(3.42394163903792,2.54576387140554,4.3317204911126));
#16977=CARTESIAN_POINT('Ctrl Pts',(3.59702533363695,2.64299053446886,4.32222757811361));
#16978=CARTESIAN_POINT('Ctrl Pts',(3.80250223745458,2.5338839434383,4.3111137890568));
#16979=CARTESIAN_POINT('Ctrl Pts',(3.81563717950601,2.38027862564402,4.30370459635227));
#16980=CARTESIAN_POINT('Ctrl Pts',(3.78826275096636,2.31767678198967,4.3));
#16981=CARTESIAN_POINT('',(3.72235838409899,2.2344646706273,4.3));
#16982=CARTESIAN_POINT('Origin',(3.6,2.4,4.3));
#16983=CARTESIAN_POINT('Ctrl Pts',(3.394277315143,2.4001195557093,4.34540747194623));
#16984=CARTESIAN_POINT('Ctrl Pts',(3.39422704674216,2.40728359221916,4.34501772883951));
#16985=CARTESIAN_POINT('Ctrl Pts',(3.39781627947545,2.48249299124839,4.34092338938053));
#16986=CARTESIAN_POINT('Ctrl Pts',(3.49037003538787,2.61673301642169,4.33312445356927));
#16987=CARTESIAN_POINT('Ctrl Pts',(3.72265542052987,2.60960761604941,4.32201066451248));
#16988=CARTESIAN_POINT('Ctrl Pts',(3.84179830935629,2.41200908789601,4.31096917998937));
#16989=CARTESIAN_POINT('Ctrl Pts',(3.77594284069862,2.27417970060314,4.30363229181856));
#16990=CARTESIAN_POINT('Ctrl Pts',(3.72235851517117,2.23446447326397,4.3));
#16991=CARTESIAN_POINT('Origin',(3.6,2.4,5.35459252805377));
#16992=CARTESIAN_POINT('',(3.39480734911062,2.40010265425899,4.41540747194623));
#16993=CARTESIAN_POINT('',(3.39433274005607,2.39985021891194,4.40959252805377));
#16994=CARTESIAN_POINT('',(3.394525,2.40000000000001,5.35459252805377));
#16995=CARTESIAN_POINT('Ctrl Pts',(3.39433274005607,2.39985021891194,4.40959252805377));
#16996=CARTESIAN_POINT('Ctrl Pts',(3.39481384314024,2.45851949137253,4.40640305253959));
#16997=CARTESIAN_POINT('Ctrl Pts',(3.45186169840294,2.58615034863243,4.39950898067315));
#16998=CARTESIAN_POINT('Ctrl Pts',(3.66843098640644,2.63302756431036,4.38891031245443));
#16999=CARTESIAN_POINT('Ctrl Pts',(3.83289206978718,2.4688824684104,4.37779652339763));
#17000=CARTESIAN_POINT('Ctrl Pts',(3.78418106902943,2.24170425860662,4.36668273434082));
#17001=CARTESIAN_POINT('Ctrl Pts',(3.56689371899776,2.15938431325527,4.35556894528402));
#17002=CARTESIAN_POINT('Ctrl Pts',(3.41495577575702,2.27149583748734,4.34653887652167));
#17003=CARTESIAN_POINT('Ctrl Pts',(3.39474723286599,2.36992492448255,4.34121340411158));
#17004=CARTESIAN_POINT('Ctrl Pts',(3.39483887138702,2.39991986985508,4.33959252805377));
#17005=CARTESIAN_POINT('Ctrl Pts',(3.39480734911062,2.40010265425899,4.41540747194623));
#17006=CARTESIAN_POINT('Ctrl Pts',(3.3946821849205,2.42777437678442,4.41391197361979));
#17007=CARTESIAN_POINT('Ctrl Pts',(3.41278383405305,2.52383658927861,4.40871187894108));
#17008=CARTESIAN_POINT('Ctrl Pts',(3.55878722266986,2.63934344974957,4.3998071879101));
#17009=CARTESIAN_POINT('Ctrl Pts',(3.77873475080197,2.56443107632444,4.38869339885329));
#17010=CARTESIAN_POINT('Ctrl Pts',(3.8350828706128,2.33901445723046,4.37757960979649));
#17011=CARTESIAN_POINT('Ctrl Pts',(3.67625990394949,2.16941582752504,4.36646582073968));
#17012=CARTESIAN_POINT('Ctrl Pts',(3.45564722223464,2.20942500090864,4.3557417747896));
#17013=CARTESIAN_POINT('Ctrl Pts',(3.394704859258,2.33918780536763,4.34872232519178));
#17014=CARTESIAN_POINT('Ctrl Pts',(3.394277315143,2.4001195557093,4.34540747194623));
#17015=CARTESIAN_POINT('Origin',(3.6,2.4,5.35459252805377));
#17016=CARTESIAN_POINT('',(3.39465010046741,2.39982347235041,4.48540747194623));
#17017=CARTESIAN_POINT('',(3.39437120031462,2.40016339024638,4.47959252805377));
#17018=CARTESIAN_POINT('',(3.394525,2.40000000000001,5.35459252805377));
#17019=CARTESIAN_POINT('Ctrl Pts',(3.39437120031462,2.40016339024638,4.47959252805377));
#17020=CARTESIAN_POINT('Ctrl Pts',(3.39427672852213,2.41103322262123,4.47900189367213));
#17021=CARTESIAN_POINT('Ctrl Pts',(3.40000383140382,2.48998144241434,4.47470666293823));
#17022=CARTESIAN_POINT('Ctrl Pts',(3.5022614856576,2.62233051762717,4.46670683585207));
#17023=CARTESIAN_POINT('Ctrl Pts',(3.73378446379617,2.60269537158839,4.45559304679526));
#17024=CARTESIAN_POINT('Ctrl Pts',(3.84285303079348,2.39753073097072,4.44447925773845));
#17025=CARTESIAN_POINT('Ctrl Pts',(3.72963541291671,2.19462648510256,4.43336546868165));
#17026=CARTESIAN_POINT('Ctrl Pts',(3.49776113486282,2.17970245626759,4.42225167962485));
#17027=CARTESIAN_POINT('Ctrl Pts',(3.39915518291127,2.31283529949844,4.41432736608222));
#17028=CARTESIAN_POINT('Ctrl Pts',(3.39425503880932,2.39037475353659,4.41010764889186));
#17029=CARTESIAN_POINT('Ctrl Pts',(3.39433274005607,2.39985021891194,4.40959252805377));
#17030=CARTESIAN_POINT('Ctrl Pts',(3.39465010046741,2.39982347235041,4.48540747194623));
#17031=CARTESIAN_POINT('Ctrl Pts',(3.39504368040953,2.44786270507631,4.48280621840007));
#17032=CARTESIAN_POINT('Ctrl Pts',(3.43581223293462,2.56491921556266,4.47650036850162));
#17033=CARTESIAN_POINT('Ctrl Pts',(3.63081864137997,2.64090222813732,4.46648992225093));
#17034=CARTESIAN_POINT('Ctrl Pts',(3.81910984841827,2.50475947107891,4.45537613319412));
#17035=CARTESIAN_POINT('Ctrl Pts',(3.80684730359907,2.27272920356226,4.44426234413732));
#17036=CARTESIAN_POINT('Ctrl Pts',(3.60525512148808,2.15719129638054,4.43314855508051));
#17037=CARTESIAN_POINT('Ctrl Pts',(3.42662677463403,2.24954018398722,4.42353026435015));
#17038=CARTESIAN_POINT('Ctrl Pts',(3.39499223729164,2.35922694980568,4.41761656997206));
#17039=CARTESIAN_POINT('Ctrl Pts',(3.39480734911062,2.40010265425899,4.41540747194623));
#17040=CARTESIAN_POINT('Origin',(3.6,2.4,5.35459252805377));
#17041=CARTESIAN_POINT('',(3.39418405900746,2.40000082772182,4.55540747194623));
#17042=CARTESIAN_POINT('',(3.39484822543359,2.40004689761745,4.54959252805377));
#17043=CARTESIAN_POINT('',(3.394525,2.40000000000001,5.35459252805377));
#17044=CARTESIAN_POINT('Ctrl Pts',(3.39484822543359,2.40004689761745,4.54959252805377));
#17045=CARTESIAN_POINT('Ctrl Pts',(3.3947841161748,2.43145144364515,4.54789613845241));
#17046=CARTESIAN_POINT('Ctrl Pts',(3.41632347620735,2.53135423912678,4.54249515249878));
#17047=CARTESIAN_POINT('Ctrl Pts',(3.57178887938318,2.64122151037363,4.5333895701929));
#17048=CARTESIAN_POINT('Ctrl Pts',(3.78736363324621,2.55452687009752,4.52227578113608));
#17049=CARTESIAN_POINT('Ctrl Pts',(3.83144232915068,2.3263920312721,4.51116199207928));
#17050=CARTESIAN_POINT('Ctrl Pts',(3.66367923564831,2.1656314047897,4.50004820302247));
#17051=CARTESIAN_POINT('Ctrl Pts',(3.44964305208187,2.21653398832958,4.48952504834731));
#17052=CARTESIAN_POINT('Ctrl Pts',(3.39486927759939,2.34285510326715,4.4827064900244));
#17053=CARTESIAN_POINT('Ctrl Pts',(3.39437120031462,2.40016339024638,4.47959252805377));
#17054=CARTESIAN_POINT('Ctrl Pts',(3.39418406069018,2.40000082771773,4.55540747194623));
#17055=CARTESIAN_POINT('Ctrl Pts',(3.39418405804479,2.40004511873352,4.55540505953261));
#17056=CARTESIAN_POINT('Ctrl Pts',(3.39420412805525,2.46810441674863,4.55169805076671));
#17057=CARTESIAN_POINT('Ctrl Pts',(3.46841582920963,2.6041305389052,4.54428644564855));
#17058=CARTESIAN_POINT('Ctrl Pts',(3.70013763173937,2.6212603119689,4.53317265659175));
#17059=CARTESIAN_POINT('Ctrl Pts',(3.84020232447629,2.43586801205837,4.52205886753494));
#17060=CARTESIAN_POINT('Ctrl Pts',(3.76040710518764,2.21764531427324,4.51094507847815));
#17061=CARTESIAN_POINT('Ctrl Pts',(3.53378944408678,2.16633392770918,4.49983128942133));
#17062=CARTESIAN_POINT('Ctrl Pts',(3.40663178603677,2.29085017634376,4.4913187539107));
#17063=CARTESIAN_POINT('Ctrl Pts',(3.39448316034026,2.37944724185309,4.48651081475233));
#17064=CARTESIAN_POINT('Ctrl Pts',(3.39465010046741,2.39982347235041,4.48540747194623));
#17065=CARTESIAN_POINT('Origin',(3.6,2.4,5.35459252805377));
#17066=CARTESIAN_POINT('',(3.3946525152789,2.40017600729827,4.62540747194623));
#17067=CARTESIAN_POINT('',(3.39454318727431,2.3998121083938,4.61959252805377));
#17068=CARTESIAN_POINT('',(3.394525,2.40000000000001,5.35459252805377));
#17069=CARTESIAN_POINT('Ctrl Pts',(3.39454318727431,2.3998121083938,4.61959252805377));
#17070=CARTESIAN_POINT('Ctrl Pts',(3.39501368913604,2.45149296169584,4.61679038323269));
#17071=CARTESIAN_POINT('Ctrl Pts',(3.44097934710978,2.57224452612634,4.61028364205933));
#17072=CARTESIAN_POINT('Ctrl Pts',(3.64379902916374,2.63888350626668,4.60007230453372));
#17073=CARTESIAN_POINT('Ctrl Pts',(3.8244536406683,2.49275908427381,4.5889585154769));
#17074=CARTESIAN_POINT('Ctrl Pts',(3.79966328939795,2.26173122045618,4.57784472642011));
#17075=CARTESIAN_POINT('Ctrl Pts',(3.59211886499353,2.15726233868846,4.56673093736329));
#17076=CARTESIAN_POINT('Ctrl Pts',(3.42236627044389,2.25700668735564,4.55731353790786));
#17077=CARTESIAN_POINT('Ctrl Pts',(3.39492411875798,2.36286981206378,4.55160073480468));
#17078=CARTESIAN_POINT('Ctrl Pts',(3.39484822543359,2.40004689761745,4.54959252805377));
#17079=CARTESIAN_POINT('Ctrl Pts',(3.3946525152789,2.40017600729827,4.62540747194623));
#17080=CARTESIAN_POINT('Ctrl Pts',(3.3944854829676,2.42064195048213,4.62429930431288));
#17081=CARTESIAN_POINT('Ctrl Pts',(3.40670159662045,2.50933048007129,4.61948654032727));
#17082=CARTESIAN_POINT('Ctrl Pts',(3.53409308462842,2.63375189718637,4.61096917998938));
#17083=CARTESIAN_POINT('Ctrl Pts',(3.76064388996454,2.58214612691277,4.59985539093257));
#17084=CARTESIAN_POINT('Ctrl Pts',(3.84015552099323,2.36381994099575,4.58874160187577));
#17085=CARTESIAN_POINT('Ctrl Pts',(3.6998500801025,2.17860977340027,4.57762781281896));
#17086=CARTESIAN_POINT('Ctrl Pts',(3.46820102232696,2.19603680731826,4.56651643617579));
#17087=CARTESIAN_POINT('Ctrl Pts',(3.3941881204111,2.33203010926412,4.55910965588488));
#17088=CARTESIAN_POINT('Ctrl Pts',(3.39418406069018,2.40000082771773,4.55540747194623));
#17089=CARTESIAN_POINT('Origin',(3.6,2.4,5.35459252805377));
#17090=CARTESIAN_POINT('',(3.39480596940119,2.39989608913133,4.69540747194623));
#17091=CARTESIAN_POINT('',(3.394211384704,2.40006787741663,4.68959252805377));
#17092=CARTESIAN_POINT('',(3.394525,2.40000000000001,5.35459252805377));
#17093=CARTESIAN_POINT('Ctrl Pts',(3.394211384704,2.40006787741663,4.68959252805377));
#17094=CARTESIAN_POINT('Ctrl Pts',(3.39419531260529,2.40380178642024,4.68938922436523));
#17095=CARTESIAN_POINT('Ctrl Pts',(3.3959796032358,2.47555925126455,4.68548132432442));
#17096=CARTESIAN_POINT('Ctrl Pts',(3.47964553527297,2.61094664572852,4.67786882793135));
#17097=CARTESIAN_POINT('Ctrl Pts',(3.71195459435803,2.61552228034691,4.66675503887453));
#17098=CARTESIAN_POINT('Ctrl Pts',(3.84179034357568,2.42282792757511,4.65564124981774));
#17099=CARTESIAN_POINT('Ctrl Pts',(3.75031264922961,2.20923891380705,4.64452746076093));
#17100=CARTESIAN_POINT('Ctrl Pts',(3.5212520823821,2.17025568561017,4.63341367170412));
#17101=CARTESIAN_POINT('Ctrl Pts',(3.40385053057498,2.29836868031663,4.62510202746841));
#17102=CARTESIAN_POINT('Ctrl Pts',(3.39439165865867,2.38316790612259,4.62049497958496));
#17103=CARTESIAN_POINT('Ctrl Pts',(3.39454318727431,2.3998121083938,4.61959252805377));
#17104=CARTESIAN_POINT('Ctrl Pts',(3.39480596940119,2.39989608913133,4.69540747194623));
#17105=CARTESIAN_POINT('Ctrl Pts',(3.39499356749685,2.44086040282664,4.69319354909316));
#17106=CARTESIAN_POINT('Ctrl Pts',(3.42673277743261,2.55063876982526,4.68727502988781));
#17107=CARTESIAN_POINT('Ctrl Pts',(3.60557055501943,2.64280164712995,4.67765191433021));
#17108=CARTESIAN_POINT('Ctrl Pts',(3.80701249526159,2.52700195958257,4.6665381252734));
#17109=CARTESIAN_POINT('Ctrl Pts',(3.81897355090948,2.29495593812904,4.65542433621659));
#17110=CARTESIAN_POINT('Ctrl Pts',(3.63050563208088,2.15905793778677,4.6443105471598));
#17111=CARTESIAN_POINT('Ctrl Pts',(3.43569204443384,2.23525749529523,4.63430492573634));
#17112=CARTESIAN_POINT('Ctrl Pts',(3.39504387077152,2.35222445101461,4.62800390066515));
#17113=CARTESIAN_POINT('Ctrl Pts',(3.3946525152789,2.40017600729827,4.62540747194623));
#17114=CARTESIAN_POINT('Origin',(3.6,2.4,5.35459252805377));
#17115=CARTESIAN_POINT('',(3.39427329960995,2.39987978133526,4.76540747194623));
#17116=CARTESIAN_POINT('',(3.3947435825044,2.40014509868052,4.75959252805377));
#17117=CARTESIAN_POINT('',(3.394525,2.40000000000001,5.35459252805377));
#17118=CARTESIAN_POINT('Ctrl Pts',(3.3947435825044,2.40014509868052,4.75959252805377));
#17119=CARTESIAN_POINT('Ctrl Pts',(3.39458577035565,2.4243482239957,4.7582834691455));
#17120=CARTESIAN_POINT('Ctrl Pts',(3.40973683471182,2.51685424764646,4.75326981388497));
#17121=CARTESIAN_POINT('Ctrl Pts',(3.54682833602434,2.63697354002902,4.74455156227216));
#17122=CARTESIAN_POINT('Ctrl Pts',(3.77025746491439,2.57319376479756,4.73343777321537));
#17123=CARTESIAN_POINT('Ctrl Pts',(3.83784800531731,2.35088777249601,4.72232398415856));
#17124=CARTESIAN_POINT('Ctrl Pts',(3.68773356907346,2.1735347589994,4.71121019510175));
#17125=CARTESIAN_POINT('Ctrl Pts',(3.46153062024069,2.20292038334059,4.70029970973349));
#17126=CARTESIAN_POINT('Ctrl Pts',(3.3944881781145,2.3357625601094,4.6930938207175));
#17127=CARTESIAN_POINT('Ctrl Pts',(3.394211384704,2.40006787741663,4.68959252805377));
#17128=CARTESIAN_POINT('Ctrl Pts',(3.39427329960995,2.39987978133526,4.76540747194623));
#17129=CARTESIAN_POINT('Ctrl Pts',(3.39469744196064,2.4608980648022,4.76208779387343));
#17130=CARTESIAN_POINT('Ctrl Pts',(3.45579877538026,2.59074744458416,4.75506351944837));
#17131=CARTESIAN_POINT('Ctrl Pts',(3.67655778221991,2.63048335496042,4.74433464867103));
#17132=CARTESIAN_POINT('Ctrl Pts',(3.8351627244929,2.46068083668937,4.73322085961423));
#17133=CARTESIAN_POINT('Ctrl Pts',(3.77852055811084,2.23533646042905,4.72210707055742));
#17134=CARTESIAN_POINT('Ctrl Pts',(3.55847650032912,2.16071048934957,4.71099328150062));
#17135=CARTESIAN_POINT('Ctrl Pts',(3.41270208696854,2.27634402495147,4.70209341529689));
#17136=CARTESIAN_POINT('Ctrl Pts',(3.39467965627817,2.37231409061976,4.69689814544543));
#17137=CARTESIAN_POINT('Ctrl Pts',(3.39480596940119,2.39989608913133,4.69540747194623));
#17138=CARTESIAN_POINT('Origin',(3.6,2.4,5.35459252805377));
#17139=CARTESIAN_POINT('',(3.39444175184043,2.40017991402784,4.83540747194624));
#17140=CARTESIAN_POINT('',(3.39473574996246,2.39985120338455,4.82959252805377));
#17141=CARTESIAN_POINT('',(3.394525,2.40000000000001,5.35459252805377));
#17142=CARTESIAN_POINT('Ctrl Pts',(3.39473574996246,2.39985120338455,4.82959252805377));
#17143=CARTESIAN_POINT('Ctrl Pts',(3.39503501794323,2.44449429908603,4.82717771392578));
#17144=CARTESIAN_POINT('Ctrl Pts',(3.43129921147106,2.55806759504416,4.82105830344552));
#17145=CARTESIAN_POINT('Ctrl Pts',(3.61869057107309,2.64214530157901,4.811234296613));
#17146=CARTESIAN_POINT('Ctrl Pts',(3.81357662871545,2.51562312999728,4.80012050755618));
#17147=CARTESIAN_POINT('Ctrl Pts',(3.81297357597085,2.28326979627357,4.78900671849939));
#17148=CARTESIAN_POINT('Ctrl Pts',(3.61743339385551,2.1577609418312,4.77789292944258));
#17149=CARTESIAN_POINT('Ctrl Pts',(3.43084782690273,2.24264334099221,4.76808819929404));
#17150=CARTESIAN_POINT('Ctrl Pts',(3.39503237387128,2.35585412553307,4.76198806549777));
#17151=CARTESIAN_POINT('Ctrl Pts',(3.3947435825044,2.40014509868052,4.75959252805377));
#17152=CARTESIAN_POINT('Ctrl Pts',(3.39444175184043,2.40017991402784,4.83540747194624));
#17153=CARTESIAN_POINT('Ctrl Pts',(3.39432006446725,2.41345772041588,4.83468663500598));
#17154=CARTESIAN_POINT('Ctrl Pts',(3.40154214948563,2.49484232576125,4.83026120171345));
#17155=CARTESIAN_POINT('Ctrl Pts',(3.51011506296999,2.62561996593247,4.82213117206865));
#17156=CARTESIAN_POINT('Ctrl Pts',(3.74080745251389,2.59788110634618,4.81101738301186));
#17157=CARTESIAN_POINT('Ctrl Pts',(3.84261718390667,2.38901942599691,4.79990359395504));
#17158=CARTESIAN_POINT('Ctrl Pts',(3.72235665540369,2.19020838956081,4.78878980489825));
#17159=CARTESIAN_POINT('Ctrl Pts',(3.49010169259086,2.18342199335841,4.77767601584144));
#17160=CARTESIAN_POINT('Ctrl Pts',(3.3977657456792,2.31768599948744,4.76988190485744));
#17161=CARTESIAN_POINT('Ctrl Pts',(3.39422412009908,2.39280468183069,4.7657923902257));
#17162=CARTESIAN_POINT('Ctrl Pts',(3.39427329960995,2.39987978133526,4.76540747194623));
#17163=CARTESIAN_POINT('Origin',(3.6,2.4,5.35459252805377));
#17164=CARTESIAN_POINT('',(3.39485784124953,2.40000781019044,4.90540747194623));
#17165=CARTESIAN_POINT('',(3.39420665921585,2.39993826201568,4.89959252805377));
#17166=CARTESIAN_POINT('',(3.394525,2.40000000000001,5.35459252805377));
#17167=CARTESIAN_POINT('Ctrl Pts',(3.39420665921585,2.39993826201568,4.89959252805377));
#17168=CARTESIAN_POINT('Ctrl Pts',(3.39446259615796,2.46459365987715,4.89607195870605));
#17169=CARTESIAN_POINT('Ctrl Pts',(3.46215556435864,2.59774588363475,4.88884679300606));
#17170=CARTESIAN_POINT('Ctrl Pts',(3.68890792061744,2.62600678347214,4.87791703095382));
#17171=CARTESIAN_POINT('Ctrl Pts',(3.83809973223177,2.44787694680091,4.86680324189701));
#17172=CARTESIAN_POINT('Ctrl Pts',(3.76935615869971,2.22592479776177,4.85568945284022));
#17173=CARTESIAN_POINT('Ctrl Pts',(3.54559897248035,2.16330565547811,4.8445756637834));
#17174=CARTESIAN_POINT('Ctrl Pts',(3.40943456861369,2.28386778049975,4.83587668885459));
#17175=CARTESIAN_POINT('Ctrl Pts',(3.39457590721621,2.37600677138249,4.83088231027805));
#17176=CARTESIAN_POINT('Ctrl Pts',(3.39473574996246,2.39985120338455,4.82959252805377));
#17177=CARTESIAN_POINT('Ctrl Pts',(3.39485784124953,2.40000781019044,4.90540747194623));
#17178=CARTESIAN_POINT('Ctrl Pts',(3.39484637525965,2.43382668251502,4.90358087978625));
#17179=CARTESIAN_POINT('Ctrl Pts',(3.41876409372263,2.5362199118863,4.898049691274));
#17180=CARTESIAN_POINT('Ctrl Pts',(3.58026192098975,2.64206213906777,4.88881390640948));
#17181=CARTESIAN_POINT('Ctrl Pts',(3.79266519873933,2.54786410019675,4.87770011735268));
#17182=CARTESIAN_POINT('Ctrl Pts',(3.82871983510845,2.3183243735256,4.86658632829587));
#17183=CARTESIAN_POINT('Ctrl Pts',(3.65542461254465,2.16354327402962,4.85547253923907));
#17184=CARTESIAN_POINT('Ctrl Pts',(3.44592887095679,2.22119506991598,4.84507958712252));
#17185=CARTESIAN_POINT('Ctrl Pts',(3.39494545222641,2.34521910726469,4.83839123135825));
#17186=CARTESIAN_POINT('Ctrl Pts',(3.39444175184043,2.40017991402784,4.83540747194624));
#17187=CARTESIAN_POINT('Origin',(3.6,2.4,5.35459252805377));
#17188=CARTESIAN_POINT('',(3.39447042093573,2.39981603086916,4.97540747194623));
#17189=CARTESIAN_POINT('',(3.39455384621585,2.40018770306997,4.96959252805377));
#17190=CARTESIAN_POINT('',(3.394525,2.40000000000001,5.35459252805377));
#17191=CARTESIAN_POINT('Ctrl Pts',(3.39455384621585,2.40018770306997,4.96959252805377));
#17192=CARTESIAN_POINT('Ctrl Pts',(3.39439993536132,2.41718968163228,4.9686707998386));
#17193=CARTESIAN_POINT('Ctrl Pts',(3.40410689916048,2.50235241402357,4.96404447527116));
#17194=CARTESIAN_POINT('Ctrl Pts',(3.52244569778922,2.63014998309056,4.95571355435144));
#17195=CARTESIAN_POINT('Ctrl Pts',(3.7513008249214,2.58997827483123,4.94459976529465));
#17196=CARTESIAN_POINT('Ctrl Pts',(3.84166859114005,2.37591729705878,4.93348597623783));
#17197=CARTESIAN_POINT('Ctrl Pts',(3.71083435517744,2.18389949043478,4.92237218718104));
#17198=CARTESIAN_POINT('Ctrl Pts',(3.47855217697512,2.18968093094735,4.91125839812423));
#17199=CARTESIAN_POINT('Ctrl Pts',(3.39580021960588,2.32515686494945,4.90366517841514));
#17200=CARTESIAN_POINT('Ctrl Pts',(3.39419328089429,2.3965585986654,4.89977655505832));
#17201=CARTESIAN_POINT('Ctrl Pts',(3.39420665921585,2.39993826201568,4.89959252805377));
#17202=CARTESIAN_POINT('Ctrl Pts',(3.39447042093573,2.39981603086916,4.97540747194623));
#17203=CARTESIAN_POINT('Ctrl Pts',(3.39496908070531,2.45384921408654,4.97247512456653));
#17204=CARTESIAN_POINT('Ctrl Pts',(3.44450059321654,2.57695438413994,4.96583818083455));
#17205=CARTESIAN_POINT('Ctrl Pts',(3.652145851588,2.63720135146115,4.95549664075031));
#17206=CARTESIAN_POINT('Ctrl Pts',(3.82756721950384,2.48483414141864,4.9443828516935));
#17207=CARTESIAN_POINT('Ctrl Pts',(3.79469373046592,2.25481727983819,4.9332690626367));
#17208=CARTESIAN_POINT('Ctrl Pts',(3.58361486203243,2.15768780841241,4.9221552735799));
#17209=CARTESIAN_POINT('Ctrl Pts',(3.41976019074743,2.26186083674666,4.91286807668307));
#17210=CARTESIAN_POINT('Ctrl Pts',(3.39486962996599,2.36523705764074,4.90728547613852));
#17211=CARTESIAN_POINT('Ctrl Pts',(3.39485784124953,2.40000781019044,4.90540747194623));
#17212=CARTESIAN_POINT('Origin',(3.6,2.4,5.35459252805377));
#17213=CARTESIAN_POINT('',(3.3942529072965,2.40010656251954,5.04540747194623));
#17214=CARTESIAN_POINT('',(3.39484564919972,2.39994744459104,5.03959252805377));
#17215=CARTESIAN_POINT('',(3.394525,2.40000000000001,5.35459252805377));
#17216=CARTESIAN_POINT('Ctrl Pts',(3.39484564919972,2.39994744459104,5.03959252805377));
#17217=CARTESIAN_POINT('Ctrl Pts',(3.39493157223083,2.43748021568483,5.03756504461887));
#17218=CARTESIAN_POINT('Ctrl Pts',(3.42276238606253,2.54371108636155,5.03183296483171));
#17219=CARTESIAN_POINT('Ctrl Pts',(3.59337897158896,2.64277529828296,5.02239628869227));
#17220=CARTESIAN_POINT('Ctrl Pts',(3.80037832359127,2.53723050760561,5.01128249963547));
#17221=CARTESIAN_POINT('Ctrl Pts',(3.82396912389365,2.30607707315216,5.00016871057866));
#17222=CARTESIAN_POINT('Ctrl Pts',(3.64255844494981,2.16089236073089,4.98905492152186));
#17223=CARTESIAN_POINT('Ctrl Pts',(3.44046962361553,2.22845545212382,4.97886286068023));
#17224=CARTESIAN_POINT('Ctrl Pts',(3.39501853158186,2.34885558191993,4.97237539619086));
#17225=CARTESIAN_POINT('Ctrl Pts',(3.39455384621585,2.40018770306997,4.96959252805377));
#17226=CARTESIAN_POINT('Ctrl Pts',(3.3942529072965,2.40010656251954,5.04540747194623));
#17227=CARTESIAN_POINT('Ctrl Pts',(3.39421422426863,2.40623506914945,5.04507396569907));
#17228=CARTESIAN_POINT('Ctrl Pts',(3.39724233203131,2.4804004332851,5.04103586309963));
#17229=CARTESIAN_POINT('Ctrl Pts',(3.48711398178203,2.61503583311392,5.03329316414794));
#17230=CARTESIAN_POINT('Ctrl Pts',(3.71944062032543,2.61146538882495,5.02217937509113));
#17231=CARTESIAN_POINT('Ctrl Pts',(3.84244192441188,2.41433825182845,5.01106558603433));
#17232=CARTESIAN_POINT('Ctrl Pts',(3.74353337567863,2.20408716238119,4.99995179697753));
#17233=CARTESIAN_POINT('Ctrl Pts',(3.51324710536571,2.17315730898832,4.98883800792072));
#17234=CARTESIAN_POINT('Ctrl Pts',(3.40217617393534,2.30323677769677,4.98065656624362));
#17235=CARTESIAN_POINT('Ctrl Pts',(3.39433909628525,2.38558611032407,4.97617972091879));
#17236=CARTESIAN_POINT('Ctrl Pts',(3.39447042093573,2.39981603086916,4.97540747194623));
#17237=CARTESIAN_POINT('Origin',(3.6,2.4,5.35459252805377));
#17238=CARTESIAN_POINT('',(3.39479089114249,2.40011619889285,5.11540747194623));
#17239=CARTESIAN_POINT('',(3.39436118415265,2.39983962587988,5.10959252805377));
#17240=CARTESIAN_POINT('',(3.394525,2.40000000000001,5.35459252805377));
#17241=CARTESIAN_POINT('Ctrl Pts',(3.39436118415265,2.39983962587988,5.10959252805377));
#17242=CARTESIAN_POINT('Ctrl Pts',(3.39485594839208,2.45749534742618,5.10645928939915));
#17243=CARTESIAN_POINT('Ctrl Pts',(3.45020483086988,2.58415305598872,5.09962145439226));
#17244=CARTESIAN_POINT('Ctrl Pts',(3.66489494817768,2.63403475512075,5.08907902303309));
#17245=CARTESIAN_POINT('Ctrl Pts',(3.83182128848718,2.47240567698227,5.0779652339763));
#17246=CARTESIAN_POINT('Ctrl Pts',(3.78655899556261,2.24450261226871,5.06685144491949));
#17247=CARTESIAN_POINT('Ctrl Pts',(3.57053712771522,2.15892819449186,5.05573765586269));
#17248=CARTESIAN_POINT('Ctrl Pts',(3.41597203014558,2.26936665662614,5.04665135024078));
#17249=CARTESIAN_POINT('Ctrl Pts',(3.39477457457446,2.36890073212835,5.04126964097114));
#17250=CARTESIAN_POINT('Ctrl Pts',(3.39484564919972,2.39994744459104,5.03959252805377));
#17251=CARTESIAN_POINT('Ctrl Pts',(3.39479089114249,2.40011619889285,5.11540747194623));
#17252=CARTESIAN_POINT('Ctrl Pts',(3.39465311263348,2.42674223574529,5.11396821047934));
#17253=CARTESIAN_POINT('Ctrl Pts',(3.4118399484044,2.5217320012959,5.10882435266019));
#17254=CARTESIAN_POINT('Ctrl Pts',(3.55516852834243,2.63869087044012,5.09997589848876));
#17255=CARTESIAN_POINT('Ctrl Pts',(3.77622353148193,2.56711958879047,5.08886210943196));
#17256=CARTESIAN_POINT('Ctrl Pts',(3.8359804180852,2.34258029751366,5.07774832037515));
#17257=CARTESIAN_POINT('Ctrl Pts',(3.6797411123384,2.17059868763558,5.06663453131835));
#17258=CARTESIAN_POINT('Ctrl Pts',(3.45739289886954,2.2074502474941,5.05585424850871));
#17259=CARTESIAN_POINT('Ctrl Pts',(3.39464391638139,2.33815945287815,5.04877856205133));
#17260=CARTESIAN_POINT('Ctrl Pts',(3.3942529072965,2.40010656251954,5.04540747194623));
#17261=CARTESIAN_POINT('Origin',(3.6,2.4,5.35459252805377));
#17262=CARTESIAN_POINT('',(3.39473291096846,2.39977036782444,5.18540747194623));
#17263=CARTESIAN_POINT('',(3.39434265438876,2.4001499379742,5.17959252805377));
#17264=CARTESIAN_POINT('',(3.394525,2.40000000000001,5.35459252805377));
#17265=CARTESIAN_POINT('',(3.54698297828114,2.20148256743283,5.2));
#17266=CARTESIAN_POINT('Ctrl Pts',(3.54698297828114,2.20148256743283,5.2));
#17267=CARTESIAN_POINT('Ctrl Pts',(3.48097120902544,2.21911198848201,5.19629540364773));
#17268=CARTESIAN_POINT('Ctrl Pts',(3.40750559920538,2.28872805295596,5.19143122762981));
#17269=CARTESIAN_POINT('Ctrl Pts',(3.39457126112442,2.3783468402669,5.18656705161189));
#17270=CARTESIAN_POINT('Ctrl Pts',(3.39473291096846,2.39977036782444,5.18540747194623));
#17271=CARTESIAN_POINT('',(3.6531315533849,2.20112677566065,5.2));
#17272=CARTESIAN_POINT('Origin',(3.6,2.4,5.2));
#17273=CARTESIAN_POINT('Ctrl Pts',(3.65313162618093,2.20112654952031,5.2));
#17274=CARTESIAN_POINT('Ctrl Pts',(3.58867175365004,2.1839946978326,5.19636770818145));
#17275=CARTESIAN_POINT('Ctrl Pts',(3.45069166079049,2.21593288928867,5.1895652175327));
#17276=CARTESIAN_POINT('Ctrl Pts',(3.39482801182151,2.34184093155955,5.18276272688396));
#17277=CARTESIAN_POINT('Ctrl Pts',(3.39434265438876,2.4001499379742,5.17959252805377));
#17278=CARTESIAN_POINT('Origin',(-3.6,2.4,4.7));
#17279=CARTESIAN_POINT('',(-3.76675586981256,2.39987855699196,4.38714803633902));
#17280=CARTESIAN_POINT('',(-3.76680083090633,2.40009693666208,4.36785196366098));
#17281=CARTESIAN_POINT('',(-3.7666,2.4,4.7));
#17282=CARTESIAN_POINT('',(-3.76351293272515,2.3680769545372,4.3));
#17283=CARTESIAN_POINT('Ctrl Pts',(-3.76680083090633,2.40009693666208,4.36785196366098));
#17284=CARTESIAN_POINT('Ctrl Pts',(-3.76684158871352,2.40590556800081,4.36746222055426));
#17285=CARTESIAN_POINT('Ctrl Pts',(-3.76656456795221,2.41171030753034,4.36707247744754));
#17286=CARTESIAN_POINT('Ctrl Pts',(-3.76595693377405,2.41748025837345,4.36668273434082));
#17287=CARTESIAN_POINT('Ctrl Pts',(-3.76018123352143,2.47232494575256,4.36297813798855));
#17288=CARTESIAN_POINT('Ctrl Pts',(-3.72453483477909,2.52402649885475,4.35927354163629));
#17289=CARTESIAN_POINT('Ctrl Pts',(-3.67532197505843,2.54891439179576,4.35556894528402));
#17290=CARTESIAN_POINT('Ctrl Pts',(-3.62610911533777,2.57380228473677,4.35186434893175));
#17291=CARTESIAN_POINT('Ctrl Pts',(-3.56332979463879,2.5718765175166,4.34815975257948));
#17292=CARTESIAN_POINT('Ctrl Pts',(-3.51573443689162,2.5440364869014,4.34445515622722));
#17293=CARTESIAN_POINT('Ctrl Pts',(-3.46813907914445,2.5161964562862,4.34075055987495));
#17294=CARTESIAN_POINT('Ctrl Pts',(-3.43572768434908,2.46244216227597,4.33704596352268));
#17295=CARTESIAN_POINT('Ctrl Pts',(-3.43329507915076,2.40733835292718,4.33334136717041));
#17296=CARTESIAN_POINT('Ctrl Pts',(-3.43086247395245,2.35223454357839,4.32963677081815));
#17297=CARTESIAN_POINT('Ctrl Pts',(-3.45840865835118,2.29578121889103,4.32593217446588));
#17298=CARTESIAN_POINT('Ctrl Pts',(-3.50340586780517,2.26388777182752,4.32222757811361));
#17299=CARTESIAN_POINT('Ctrl Pts',(-3.54840307725917,2.23199432476401,4.31852298176134));
#17300=CARTESIAN_POINT('Ctrl Pts',(-3.61085131176843,2.22466075532434,4.31481838540907));
#17301=CARTESIAN_POINT('Ctrl Pts',(-3.66197498261058,2.24508842770105,4.3111137890568));
#17302=CARTESIAN_POINT('Ctrl Pts',(-3.71309865345273,2.26551610007776,4.30740919270453));
#17303=CARTESIAN_POINT('Ctrl Pts',(-3.75289776062778,2.31370501427083,4.30370459635227));
#17304=CARTESIAN_POINT('Ctrl Pts',(-3.76351293272515,2.3680769545372,4.3));
#17305=CARTESIAN_POINT('',(-3.60525668225574,2.5668198662348,4.3));
#17306=CARTESIAN_POINT('Origin',(-3.6,2.4,4.3));
#17307=CARTESIAN_POINT('',(-3.76634548976639,2.39993502697971,4.31714803633902));
#17308=CARTESIAN_POINT('Ctrl Pts',(-3.60525667864057,2.56682005840211,4.3));
#17309=CARTESIAN_POINT('Ctrl Pts',(-3.65930634748376,2.56504681426963,4.30363229181856));
#17310=CARTESIAN_POINT('Ctrl Pts',(-3.71251717627762,2.53457816039784,4.30726458363711));
#17311=CARTESIAN_POINT('Ctrl Pts',(-3.74128611123357,2.48878409483897,4.31089687545566));
#17312=CARTESIAN_POINT('Ctrl Pts',(-3.75778985504382,2.46251362194275,4.31298059575011));
#17313=CARTESIAN_POINT('Ctrl Pts',(-3.76624996614321,2.43119967804664,4.31506431604457));
#17314=CARTESIAN_POINT('Ctrl Pts',(-3.76634548976639,2.39993502697971,4.31714803633902));
#17315=CARTESIAN_POINT('',(-3.7666,2.4,4.2));
#17316=CARTESIAN_POINT('',(-3.7666,2.4,4.7));
#17317=CARTESIAN_POINT('Origin',(-3.6,2.4,4.2));
#17318=CARTESIAN_POINT('Ctrl Pts',(-3.76634548976639,2.39993502697971,4.31714803633902));
#17319=CARTESIAN_POINT('Ctrl Pts',(-3.7664197953026,2.37561500451544,4.31876891239683));
#17320=CARTESIAN_POINT('Ctrl Pts',(-3.76143276332865,2.35132480870382,4.32038978845465));
#17321=CARTESIAN_POINT('Ctrl Pts',(-3.75123332497294,2.32946153149726,4.32201066451247));
#17322=CARTESIAN_POINT('Ctrl Pts',(-3.72792197926853,2.27949187675561,4.32571526086474));
#17323=CARTESIAN_POINT('Ctrl Pts',(-3.67738233884271,2.24219983197054,4.329419857217));
#17324=CARTESIAN_POINT('Ctrl Pts',(-3.62274960712982,2.23467803877973,4.33312445356927));
#17325=CARTESIAN_POINT('Ctrl Pts',(-3.56811687541693,2.22715624558892,4.33682904992154));
#17326=CARTESIAN_POINT('Ctrl Pts',(-3.50939105241698,2.24940470399237,4.34053364627381));
#17327=CARTESIAN_POINT('Ctrl Pts',(-3.473445625673,2.29122843734541,4.34423824262608));
#17328=CARTESIAN_POINT('Ctrl Pts',(-3.43750019892903,2.33305217069845,4.34794283897834));
#17329=CARTESIAN_POINT('Ctrl Pts',(-3.42433516844104,2.39445117900107,4.35164743533061));
#17330=CARTESIAN_POINT('Ctrl Pts',(-3.43997694242044,2.44733227209049,4.35535203168288));
#17331=CARTESIAN_POINT('Ctrl Pts',(-3.45561871639985,2.50021336517992,4.35905662803515));
#17332=CARTESIAN_POINT('Ctrl Pts',(-3.50006729484665,2.54457654305613,4.36276122438742));
#17333=CARTESIAN_POINT('Ctrl Pts',(-3.55297985590111,2.56011554237715,4.36646582073968));
#17334=CARTESIAN_POINT('Ctrl Pts',(-3.60589241695558,2.57565454169817,4.37017041709195));
#17335=CARTESIAN_POINT('Ctrl Pts',(-3.6672689606177,2.562369362464,4.37387501344422));
#17336=CARTESIAN_POINT('Ctrl Pts',(-3.70902050221487,2.52634164219194,4.37757960979649));
#17337=CARTESIAN_POINT('Ctrl Pts',(-3.74496652897209,2.49532354447962,4.38076908531067));
#17338=CARTESIAN_POINT('Ctrl Pts',(-3.76636578927508,2.4474478468568,4.38395856082485));
#17339=CARTESIAN_POINT('Ctrl Pts',(-3.76675586981256,2.39987855699196,4.38714803633902));
#17340=CARTESIAN_POINT('Origin',(-3.6,2.4,4.7));
#17341=CARTESIAN_POINT('',(-3.76672468602162,2.4001324774977,4.45714803633902));
#17342=CARTESIAN_POINT('',(-3.7663710759754,2.40008323252274,4.43785196366098));
#17343=CARTESIAN_POINT('',(-3.7666,2.4,4.7));
#17344=CARTESIAN_POINT('Ctrl Pts',(-3.7663710759754,2.40008323252274,4.43785196366098));
#17345=CARTESIAN_POINT('Ctrl Pts',(-3.76647255964094,2.42251958309795,4.43635646533454));
#17346=CARTESIAN_POINT('Ctrl Pts',(-3.76225162287627,2.44491933914913,4.43486096700809));
#17347=CARTESIAN_POINT('Ctrl Pts',(-3.75352689637225,2.46540054190021,4.43336546868165));
#17348=CARTESIAN_POINT('Ctrl Pts',(-3.73191430783919,2.516135863806,4.42966087232938));
#17349=CARTESIAN_POINT('Ctrl Pts',(-3.6826649015976,2.55509827647583,4.42595627597711));
#17350=CARTESIAN_POINT('Ctrl Pts',(-3.62831779967194,2.56445627090432,4.42225167962485));
#17351=CARTESIAN_POINT('Ctrl Pts',(-3.57397069774627,2.57381426533281,4.41854708327258));
#17352=CARTESIAN_POINT('Ctrl Pts',(-3.51452590013653,2.55356784151996,4.41484248692031));
#17353=CARTESIAN_POINT('Ctrl Pts',(-3.47718895189484,2.51298317028118,4.41113789056804));
#17354=CARTESIAN_POINT('Ctrl Pts',(-3.43985200365314,2.4723984990424,4.40743329421577));
#17355=CARTESIAN_POINT('Ctrl Pts',(-3.42462290477948,2.41147558037768,4.40372869786351));
#17356=CARTESIAN_POINT('Ctrl Pts',(-3.43847074534366,2.35809557252044,4.40002410151124));
#17357=CARTESIAN_POINT('Ctrl Pts',(-3.45231858590785,2.30471556466319,4.39631950515897));
#17358=CARTESIAN_POINT('Ctrl Pts',(-3.49524336590988,2.25887846761341,4.3926149088067));
#17359=CARTESIAN_POINT('Ctrl Pts',(-3.54760150451765,2.24156301194163,4.38891031245443));
#17360=CARTESIAN_POINT('Ctrl Pts',(-3.59995964312543,2.22424755626985,4.38520571610216));
#17361=CARTESIAN_POINT('Ctrl Pts',(-3.66175114033895,2.23545374197608,4.3815011197499));
#17362=CARTESIAN_POINT('Ctrl Pts',(-3.70469438806425,2.2700507456572,4.37779652339763));
#17363=CARTESIAN_POINT('Ctrl Pts',(-3.74311977927038,2.30100796178371,4.37448167015208));
#17364=CARTESIAN_POINT('Ctrl Pts',(-3.76645417654063,2.35069321376496,4.37116681690653));
#17365=CARTESIAN_POINT('Ctrl Pts',(-3.76680083090633,2.40009693666208,4.36785196366098));
#17366=CARTESIAN_POINT('Ctrl Pts',(-3.76675586981256,2.39987855699196,4.38714803633902));
#17367=CARTESIAN_POINT('Ctrl Pts',(-3.76681887033176,2.39219581029783,4.38766315717711));
#17368=CARTESIAN_POINT('Ctrl Pts',(-3.76633386046459,2.38452105604489,4.3881782780152));
#17369=CARTESIAN_POINT('Ctrl Pts',(-3.76527361543791,2.37692660254772,4.38869339885329));
#17370=CARTESIAN_POINT('Ctrl Pts',(-3.75764864753156,2.32230954448549,4.39239799520556));
#17371=CARTESIAN_POINT('Ctrl Pts',(-3.72027217218665,2.27184568967097,4.39610259155783));
#17372=CARTESIAN_POINT('Ctrl Pts',(-3.67024982973388,2.2486305064859,4.3998071879101));
#17373=CARTESIAN_POINT('Ctrl Pts',(-3.62022748728111,2.22541532330082,4.40351178426237));
#17374=CARTESIAN_POINT('Ctrl Pts',(-3.55755927772049,2.22944881174518,4.40721638061463));
#17375=CARTESIAN_POINT('Ctrl Pts',(-3.51092562033288,2.25888482364762,4.4109209769669));
#17376=CARTESIAN_POINT('Ctrl Pts',(-3.46429196294527,2.28832083555005,4.41462557331917));
#17377=CARTESIAN_POINT('Ctrl Pts',(-3.43369285773067,2.34315937091056,4.41833016967144));
#17378=CARTESIAN_POINT('Ctrl Pts',(-3.43313217976425,2.39830336261017,4.42203476602371));
#17379=CARTESIAN_POINT('Ctrl Pts',(-3.43257150179783,2.45344735430978,4.42573936237597));
#17380=CARTESIAN_POINT('Ctrl Pts',(-3.46204925107959,2.5088968023485,4.42944395872824));
#17381=CARTESIAN_POINT('Ctrl Pts',(-3.5080747579799,2.53927490269551,4.43314855508051));
#17382=CARTESIAN_POINT('Ctrl Pts',(-3.55410026488021,2.56965300304252,4.43685315143278));
#17383=CARTESIAN_POINT('Ctrl Pts',(-3.61667352939907,2.57495975569782,4.44055774778505));
#17384=CARTESIAN_POINT('Ctrl Pts',(-3.66715754746926,2.55276652004746,4.44426234413731));
#17385=CARTESIAN_POINT('Ctrl Pts',(-3.71764156553946,2.53057328439709,4.44796694048958));
#17386=CARTESIAN_POINT('Ctrl Pts',(-3.756036337161,2.48088006044104,4.45167153684185));
#17387=CARTESIAN_POINT('Ctrl Pts',(-3.76477027476388,2.4264292215015,4.45537613319412));
#17388=CARTESIAN_POINT('Ctrl Pts',(-3.7661627513915,2.41774796866627,4.45596676757575));
#17389=CARTESIAN_POINT('Ctrl Pts',(-3.76680128414385,2.40894578279607,4.45655740195739));
#17390=CARTESIAN_POINT('Ctrl Pts',(-3.76672468602162,2.4001324774977,4.45714803633902));
#17391=CARTESIAN_POINT('Origin',(-3.6,2.4,4.7));
#17392=CARTESIAN_POINT('',(-3.76633791206845,2.40003802478337,4.52714803633902));
#17393=CARTESIAN_POINT('',(-3.76649857382306,2.39985687062932,4.50785196366098));
#17394=CARTESIAN_POINT('',(-3.7666,2.4,4.7));
#17395=CARTESIAN_POINT('Ctrl Pts',(-3.76649857382306,2.39985687062932,4.50785196366098));
#17396=CARTESIAN_POINT('Ctrl Pts',(-3.76617945752874,2.43880728528579,4.50525071011481));
#17397=CARTESIAN_POINT('Ctrl Pts',(-3.75254366540545,2.47795898788161,4.50264945656864));
#17398=CARTESIAN_POINT('Ctrl Pts',(-3.72758425733276,2.50756395676541,4.50004820302248));
#17399=CARTESIAN_POINT('Ctrl Pts',(-3.6920381137294,2.54972611350612,4.49634360667021));
#17400=CARTESIAN_POINT('Ctrl Pts',(-3.63352511396685,2.57252533344874,4.49263901031794));
#17401=CARTESIAN_POINT('Ctrl Pts',(-3.57882406188105,2.56552742213501,4.48893441396567));
#17402=CARTESIAN_POINT('Ctrl Pts',(-3.52412300979526,2.55852951082128,4.4852298176134));
#17403=CARTESIAN_POINT('Ctrl Pts',(-3.47323390538621,2.52173446825121,4.48152522126114));
#17404=CARTESIAN_POINT('Ctrl Pts',(-3.44944644044618,2.47198175864633,4.47782062490887));
#17405=CARTESIAN_POINT('Ctrl Pts',(-3.42565897550616,2.42222904904145,4.4741160285566));
#17406=CARTESIAN_POINT('Ctrl Pts',(-3.42897315003517,2.35951867240177,4.47041143220433));
#17407=CARTESIAN_POINT('Ctrl Pts',(-3.45787220405951,2.31255037948392,4.46670683585206));
#17408=CARTESIAN_POINT('Ctrl Pts',(-3.48677125808385,2.26558208656607,4.46300223949979));
#17409=CARTESIAN_POINT('Ctrl Pts',(-3.54125519160353,2.23435587737005,4.45929764314752));
#17410=CARTESIAN_POINT('Ctrl Pts',(-3.59638914193523,2.23316262102818,4.45559304679526));
#17411=CARTESIAN_POINT('Ctrl Pts',(-3.65152309226694,2.23196936468632,4.45188845044299));
#17412=CARTESIAN_POINT('Ctrl Pts',(-3.70730705941068,2.26080906119861,4.44818385409072));
#17413=CARTESIAN_POINT('Ctrl Pts',(-3.73821115757027,2.30648302502563,4.44447925773845));
#17414=CARTESIAN_POINT('Ctrl Pts',(-3.75663966522468,2.33371899184293,4.44227015971263));
#17415=CARTESIAN_POINT('Ctrl Pts',(-3.76622116784026,2.36694103711801,4.4400610616868));
#17416=CARTESIAN_POINT('Ctrl Pts',(-3.7663710759754,2.40008323252274,4.43785196366098));
#17417=CARTESIAN_POINT('Ctrl Pts',(-3.76672468602162,2.4001324774977,4.45714803633902));
#17418=CARTESIAN_POINT('Ctrl Pts',(-3.76632084288778,2.35366668006347,4.46026199830966));
#17419=CARTESIAN_POINT('Ctrl Pts',(-3.74603890809821,2.30689180212375,4.46337596028029));
#17420=CARTESIAN_POINT('Ctrl Pts',(-3.71156689963546,2.27590095059859,4.46648992225092));
#17421=CARTESIAN_POINT('Ctrl Pts',(-3.67055648331992,2.23903197255825,4.47019451860319));
#17422=CARTESIAN_POINT('Ctrl Pts',(-3.60946254710462,2.2245024704006,4.47389911495546));
#17423=CARTESIAN_POINT('Ctrl Pts',(-3.55624507667009,2.23896195008268,4.47760371130773));
#17424=CARTESIAN_POINT('Ctrl Pts',(-3.50302760623556,2.25342142976477,4.48130830766));
#17425=CARTESIAN_POINT('Ctrl Pts',(-3.45768660158179,2.29686989128659,4.48501290401227));
#17426=CARTESIAN_POINT('Ctrl Pts',(-3.4409726309165,2.34942290140806,4.48871750036453));
#17427=CARTESIAN_POINT('Ctrl Pts',(-3.4242586602512,2.40197591152952,4.4924220967168));
#17428=CARTESIAN_POINT('Ctrl Pts',(-3.43617172357437,2.46363347025063,4.49612669306907));
#17429=CARTESIAN_POINT('Ctrl Pts',(-3.47125973974121,2.50617764542895,4.49983128942133));
#17430=CARTESIAN_POINT('Ctrl Pts',(-3.50634775590806,2.54872182060726,4.5035358857736));
#17431=CARTESIAN_POINT('Ctrl Pts',(-3.56461072491859,2.57215261224279,4.50724048212587));
#17432=CARTESIAN_POINT('Ctrl Pts',(-3.61938426871317,2.56574678606726,4.51094507847814));
#17433=CARTESIAN_POINT('Ctrl Pts',(-3.67415781250775,2.55934095989172,4.51464967483041));
#17434=CARTESIAN_POINT('Ctrl Pts',(-3.72544193108638,2.52309851590513,4.51835427118267));
#17435=CARTESIAN_POINT('Ctrl Pts',(-3.7497661567401,2.47360601391412,4.52205886753494));
#17436=CARTESIAN_POINT('Ctrl Pts',(-3.7609045803459,2.45094266337894,4.5237552571363));
#17437=CARTESIAN_POINT('Ctrl Pts',(-3.76638989212213,2.42550096131782,4.52545164673766));
#17438=CARTESIAN_POINT('Ctrl Pts',(-3.76633791206845,2.40003802478337,4.52714803633902));
#17439=CARTESIAN_POINT('Origin',(-3.6,2.4,4.7));
#17440=CARTESIAN_POINT('',(-3.76658523827666,2.39984765670423,4.59714803633902));
#17441=CARTESIAN_POINT('',(-3.76687644222506,2.40000067112036,4.57785196366098));
#17442=CARTESIAN_POINT('',(-3.7666,2.4,4.7));
#17443=CARTESIAN_POINT('Ctrl Pts',(-3.76687644086079,2.40000067111705,4.57785196366098));
#17444=CARTESIAN_POINT('Ctrl Pts',(-3.76687973678962,2.45518344204594,4.57414495489509));
#17445=CARTESIAN_POINT('Ctrl Pts',(-3.73679497953693,2.51036312381259,4.57043794612919));
#17446=CARTESIAN_POINT('Ctrl Pts',(-3.69041339694851,2.54026106127768,4.5667309373633));
#17447=CARTESIAN_POINT('Ctrl Pts',(-3.64406199814677,2.57013954203352,4.56302634101103));
#17448=CARTESIAN_POINT('Ctrl Pts',(-3.58143498975323,2.57476917303812,4.55932174465876));
#17449=CARTESIAN_POINT('Ctrl Pts',(-3.53119397724287,2.55203117737673,4.55561714830649));
#17450=CARTESIAN_POINT('Ctrl Pts',(-3.4809529647325,2.52929318171533,4.55191255195423));
#17451=CARTESIAN_POINT('Ctrl Pts',(-3.44309794810529,2.47918755938795,4.54820795560196));
#17452=CARTESIAN_POINT('Ctrl Pts',(-3.43495349044459,2.42464543263837,4.54450335924969));
#17453=CARTESIAN_POINT('Ctrl Pts',(-3.42680903278389,2.37010330588879,4.54079876289742));
#17454=CARTESIAN_POINT('Ctrl Pts',(-3.44837513408969,2.31112467471701,4.53709416654516));
#17455=CARTESIAN_POINT('Ctrl Pts',(-3.48978194566841,2.27470144397531,4.53338957019289));
#17456=CARTESIAN_POINT('Ctrl Pts',(-3.53118875724712,2.23827821323361,4.52968497384062));
#17457=CARTESIAN_POINT('Ctrl Pts',(-3.59243627909875,2.22441038292198,4.52598037748835));
#17458=CARTESIAN_POINT('Ctrl Pts',(-3.64549423583691,2.23944464448895,4.52227578113608));
#17459=CARTESIAN_POINT('Ctrl Pts',(-3.69855219257508,2.25447890605592,4.51857118478381));
#17460=CARTESIAN_POINT('Ctrl Pts',(-3.74342058419978,2.29841525950148,4.51486658843154));
#17461=CARTESIAN_POINT('Ctrl Pts',(-3.75956513629004,2.35114598299368,4.51116199207928));
#17462=CARTESIAN_POINT('Ctrl Pts',(-3.76437348076611,2.36685081528665,4.51005864927318));
#17463=CARTESIAN_POINT('Ctrl Pts',(-3.76663392958958,2.3833357360905,4.50895530646708));
#17464=CARTESIAN_POINT('Ctrl Pts',(-3.76649857382306,2.39985687062932,4.50785196366098));
#17465=CARTESIAN_POINT('Ctrl Pts',(-3.76633791206845,2.40003802478337,4.52714803633902));
#17466=CARTESIAN_POINT('Ctrl Pts',(-3.76627637744537,2.36989468919261,4.52915624308993));
#17467=CARTESIAN_POINT('Ctrl Pts',(-3.758454818996,2.33972159536913,4.53116444984084));
#17468=CARTESIAN_POINT('Ctrl Pts',(-3.74306538301875,2.31409282238037,4.53317265659175));
#17469=CARTESIAN_POINT('Ctrl Pts',(-3.71467605091489,2.26681469283306,4.53687725294402));
#17470=CARTESIAN_POINT('Ctrl Pts',(-3.66053305397837,2.23500099373388,4.54058184929628));
#17471=CARTESIAN_POINT('Ctrl Pts',(-3.6054152417587,2.23321144482349,4.54428644564855));
#17472=CARTESIAN_POINT('Ctrl Pts',(-3.55029742953903,2.23142189591311,4.54799104200082));
#17473=CARTESIAN_POINT('Ctrl Pts',(-3.49420480203621,2.25965649719153,4.55169563835309));
#17474=CARTESIAN_POINT('Ctrl Pts',(-3.46280846829882,2.30499352330658,4.55540023470536));
#17475=CARTESIAN_POINT('Ctrl Pts',(-3.43141213456143,2.35033054942163,4.55910483105762));
#17476=CARTESIAN_POINT('Ctrl Pts',(-3.42471209458945,2.41277000037331,4.56280942740989));
#17477=CARTESIAN_POINT('Ctrl Pts',(-3.44577465966535,2.46373610736585,4.56651402376216));
#17478=CARTESIAN_POINT('Ctrl Pts',(-3.46683722474125,2.51470221435838,4.57021862011443));
#17479=CARTESIAN_POINT('Ctrl Pts',(-3.51566239486502,2.55419497739177,4.5739232164667));
#17480=CARTESIAN_POINT('Ctrl Pts',(-3.56990505407324,2.56414030953056,4.57762781281897));
#17481=CARTESIAN_POINT('Ctrl Pts',(-3.62414771328146,2.57408564166935,4.58133240917123));
#17482=CARTESIAN_POINT('Ctrl Pts',(-3.68380786157412,2.55448354291355,4.5850370055235));
#17483=CARTESIAN_POINT('Ctrl Pts',(-3.72158169378842,2.51430502490722,4.58874160187577));
#17484=CARTESIAN_POINT('Ctrl Pts',(-3.75015369954742,2.4839141225134,4.59154374669685));
#17485=CARTESIAN_POINT('Ctrl Pts',(-3.76620375341029,2.44175070750818,4.59434589151794));
#17486=CARTESIAN_POINT('Ctrl Pts',(-3.76658523827666,2.39984765670423,4.59714803633902));
#17487=CARTESIAN_POINT('Origin',(-3.6,2.4,4.7));
#17488=CARTESIAN_POINT('',(-3.76685426518066,2.40005503529171,4.66714803633902));
#17489=CARTESIAN_POINT('',(-3.76649661588353,2.40014270746765,4.64785196366098));
#17490=CARTESIAN_POINT('',(-3.7666,2.4,4.7));
#17491=CARTESIAN_POINT('Ctrl Pts',(-3.76649661588353,2.40014270746765,4.64785196366098));
#17492=CARTESIAN_POINT('Ctrl Pts',(-3.76663204639349,2.41673658143502,4.64674379602763));
#17493=CARTESIAN_POINT('Ctrl Pts',(-3.76435138934107,2.43329406659146,4.64563562839428));
#17494=CARTESIAN_POINT('Ctrl Pts',(-3.75950152904524,2.44906128711078,4.64452746076093));
#17495=CARTESIAN_POINT('Ctrl Pts',(-3.74328848128947,2.50177099082653,4.64082286440866));
#17496=CARTESIAN_POINT('Ctrl Pts',(-3.69836304459695,2.54564901270383,4.63711826805639));
#17497=CARTESIAN_POINT('Ctrl Pts',(-3.64528559981485,2.5606143272255,4.63341367170412));
#17498=CARTESIAN_POINT('Ctrl Pts',(-3.59220815503275,2.57557964174716,4.62970907535186));
#17499=CARTESIAN_POINT('Ctrl Pts',(-3.53097870216106,2.56163224891319,4.62600447899959));
#17500=CARTESIAN_POINT('Ctrl Pts',(-3.48961924750057,2.52515525214062,4.62229988264732));
#17501=CARTESIAN_POINT('Ctrl Pts',(-3.44825979284008,2.48867825536805,4.61859528629505));
#17502=CARTESIAN_POINT('Ctrl Pts',(-3.4267703363908,2.42967165465689,4.61489068994278));
#17503=CARTESIAN_POINT('Ctrl Pts',(-3.43498564975134,2.37514015541382,4.61118609359051));
#17504=CARTESIAN_POINT('Ctrl Pts',(-3.44320096311188,2.32060865617075,4.60748149723825));
#17505=CARTESIAN_POINT('Ctrl Pts',(-3.48112104628225,2.27055225839578,4.60377690088598));
#17506=CARTESIAN_POINT('Ctrl Pts',(-3.53139155817582,2.2478795563676,4.60007230453371));
#17507=CARTESIAN_POINT('Ctrl Pts',(-3.58166207006939,2.22520685433943,4.59636770818145));
#17508=CARTESIAN_POINT('Ctrl Pts',(-3.64428301068616,2.22991784805805,4.59266311182918));
#17509=CARTESIAN_POINT('Ctrl Pts',(-3.69059555147242,2.25985652453919,4.58895851547691));
#17510=CARTESIAN_POINT('Ctrl Pts',(-3.73687793377613,2.28977570511195,4.58525633153827));
#17511=CARTESIAN_POINT('Ctrl Pts',(-3.76687314922176,2.34488972287695,4.58155414759963));
#17512=CARTESIAN_POINT('Ctrl Pts',(-3.76687644086079,2.40000067111705,4.57785196366098));
#17513=CARTESIAN_POINT('Ctrl Pts',(-3.76658523827666,2.39984765670423,4.59714803633902));
#17514=CARTESIAN_POINT('Ctrl Pts',(-3.76670809830844,2.38635246827757,4.5980504878702));
#17515=CARTESIAN_POINT('Ctrl Pts',(-3.76520579898216,2.37288428508147,4.59895293940139));
#17516=CARTESIAN_POINT('Ctrl Pts',(-3.76197323034856,2.35984505467766,4.59985539093257));
#17517=CARTESIAN_POINT('Ctrl Pts',(-3.74870341855848,2.30631853971129,4.60355998728484));
#17518=CARTESIAN_POINT('Ctrl Pts',(-3.70627627884239,2.26002044703541,4.60726458363711));
#17519=CARTESIAN_POINT('Ctrl Pts',(-3.65410883226945,2.24213936129044,4.61096917998938));
#17520=CARTESIAN_POINT('Ctrl Pts',(-3.60194138569651,2.22425827554546,4.61467377634165));
#17521=CARTESIAN_POINT('Ctrl Pts',(-3.54003363226672,2.23479419673139,4.61837837269391));
#17522=CARTESIAN_POINT('Ctrl Pts',(-3.49671800637814,2.26892530077511,4.62208296904618));
#17523=CARTESIAN_POINT('Ctrl Pts',(-3.45340238048956,2.30305640481884,4.62578756539845));
#17524=CARTESIAN_POINT('Ctrl Pts',(-3.42867888214219,2.36078269172036,4.62949216175072));
#17525=CARTESIAN_POINT('Ctrl Pts',(-3.43386236054643,2.4156853989487,4.63319675810298));
#17526=CARTESIAN_POINT('Ctrl Pts',(-3.43904583895067,2.47058810617705,4.63690135445525));
#17527=CARTESIAN_POINT('Ctrl Pts',(-3.47413629410653,2.52266723373221,4.64060595080752));
#17528=CARTESIAN_POINT('Ctrl Pts',(-3.52307438023553,2.54808847357993,4.64431054715979));
#17529=CARTESIAN_POINT('Ctrl Pts',(-3.57201246636453,2.57350971342765,4.64801514351206));
#17530=CARTESIAN_POINT('Ctrl Pts',(-3.63479818346667,2.57227306556792,4.65171973986433));
#17531=CARTESIAN_POINT('Ctrl Pts',(-3.68269729209092,2.54494448890598,4.65542433621659));
#17532=CARTESIAN_POINT('Ctrl Pts',(-3.73059640071517,2.51761591224403,4.65912893256886));
#17533=CARTESIAN_POINT('Ctrl Pts',(-3.76360890086153,2.46419540677987,4.66283352892113));
#17534=CARTESIAN_POINT('Ctrl Pts',(-3.76662643464441,2.40913116975406,4.6665381252734));
#17535=CARTESIAN_POINT('Ctrl Pts',(-3.76679203318471,2.406109312194,4.66674142896194));
#17536=CARTESIAN_POINT('Ctrl Pts',(-3.76686729650514,2.4030825042416,4.66694473265048));
#17537=CARTESIAN_POINT('Ctrl Pts',(-3.76685426518066,2.40005503529171,4.66714803633902));
#17538=CARTESIAN_POINT('Origin',(-3.6,2.4,4.7));
#17539=CARTESIAN_POINT('',(-3.76642275699063,2.40011764661364,4.73714803633902));
#17540=CARTESIAN_POINT('',(-3.76637219462709,2.39991574862477,4.71785196366098));
#17541=CARTESIAN_POINT('',(-3.7666,2.4,4.7));
#17542=CARTESIAN_POINT('Ctrl Pts',(-3.76637219462709,2.39991574862477,4.71785196366098));
#17543=CARTESIAN_POINT('Ctrl Pts',(-3.76622008929152,2.43312978877493,4.7156380408079));
#17544=CARTESIAN_POINT('Ctrl Pts',(-3.75659374130514,2.46642503349729,4.71342411795483));
#17545=CARTESIAN_POINT('Ctrl Pts',(-3.73808953093009,2.49369647329664,4.71121019510175));
#17546=CARTESIAN_POINT('Ctrl Pts',(-3.70712610771876,2.53933025690454,4.70750559874949));
#17547=CARTESIAN_POINT('Ctrl Pts',(-3.65130473898255,2.56809743365675,4.70380100239722));
#17548=CARTESIAN_POINT('Ctrl Pts',(-3.59617239065227,2.56683254199167,4.70009640604495));
#17549=CARTESIAN_POINT('Ctrl Pts',(-3.541040042322,2.56556765032658,4.69639180969268));
#17550=CARTESIAN_POINT('Ctrl Pts',(-3.48659671439765,2.53427069024418,4.69268721334041));
#17551=CARTESIAN_POINT('Ctrl Pts',(-3.45775870461848,2.48726489299201,4.68898261698815));
#17552=CARTESIAN_POINT('Ctrl Pts',(-3.4289206948393,2.44025909573984,4.68527802063588));
#17553=CARTESIAN_POINT('Ctrl Pts',(-3.4256880032053,2.3775444613179,4.68157342428361));
#17554=CARTESIAN_POINT('Ctrl Pts',(-3.44954008937339,2.32782269778556,4.67786882793134));
#17555=CARTESIAN_POINT('Ctrl Pts',(-3.47339217554148,2.27810093425323,4.67416423157907));
#17556=CARTESIAN_POINT('Ctrl Pts',(-3.52432903951166,2.2413720416105,4.67045963522681));
#17557=CARTESIAN_POINT('Ctrl Pts',(-3.57903913665629,2.23444520584228,4.66675503887454));
#17558=CARTESIAN_POINT('Ctrl Pts',(-3.63374923380092,2.22751837007406,4.66305044252227));
#17559=CARTESIAN_POINT('Ctrl Pts',(-3.69223256411999,2.25039359118035,4.65934584617));
#17560=CARTESIAN_POINT('Ctrl Pts',(-3.72772389987002,2.29260189451059,4.65564124981773));
#17561=CARTESIAN_POINT('Ctrl Pts',(-3.75259860001318,2.32218429445987,4.65304482109882));
#17562=CARTESIAN_POINT('Ctrl Pts',(-3.766179303182,2.36126338124449,4.6504483923799));
#17563=CARTESIAN_POINT('Ctrl Pts',(-3.76649661588353,2.40014270746765,4.64785196366098));
#17564=CARTESIAN_POINT('Ctrl Pts',(-3.76685426518066,2.40005503529171,4.66714803633902));
#17565=CARTESIAN_POINT('Ctrl Pts',(-3.76662983993221,2.34791601656576,4.67064932900275));
#17566=CARTESIAN_POINT('Ctrl Pts',(-3.7402175145738,2.29558094816933,4.67415062166648));
#17567=CARTESIAN_POINT('Ctrl Pts',(-3.69804051189557,2.26495998737175,4.6776519143302));
#17568=CARTESIAN_POINT('Ctrl Pts',(-3.65341448794446,2.23256101060272,4.68135651068247));
#17569=CARTESIAN_POINT('Ctrl Pts',(-3.59113987262282,2.22447102565214,4.68506110703474));
#17570=CARTESIAN_POINT('Ctrl Pts',(-3.53971699675369,2.24439246000598,4.68876570338701));
#17571=CARTESIAN_POINT('Ctrl Pts',(-3.48829412088457,2.26431389435981,4.69247029973927));
#17572=CARTESIAN_POINT('Ctrl Pts',(-3.44772298446796,2.31224674801807,4.69617489609154));
#17573=CARTESIAN_POINT('Ctrl Pts',(-3.43657119813891,2.36625427870627,4.69987949244381));
#17574=CARTESIAN_POINT('Ctrl Pts',(-3.42541941180987,2.42026180939447,4.70358408879608));
#17575=CARTESIAN_POINT('Ctrl Pts',(-3.44368697556839,2.48034401711262,4.70728868514835));
#17576=CARTESIAN_POINT('Ctrl Pts',(-3.48301363527625,2.51900393880922,4.71099328150062));
#17577=CARTESIAN_POINT('Ctrl Pts',(-3.52234029498412,2.55766386050582,4.71469787785288));
#17578=CARTESIAN_POINT('Ctrl Pts',(-3.58272605064134,2.57490149618086,4.71840247420515));
#17579=CARTESIAN_POINT('Ctrl Pts',(-3.63653501876085,2.56282794412363,4.72210707055742));
#17580=CARTESIAN_POINT('Ctrl Pts',(-3.69034398688037,2.5507543920664,4.72581166690969));
#17581=CARTESIAN_POINT('Ctrl Pts',(-3.73757616746218,2.50936965227689,4.72951626326196));
#17582=CARTESIAN_POINT('Ctrl Pts',(-3.75661548523835,2.45761368558721,4.73322085961422));
#17583=CARTESIAN_POINT('Ctrl Pts',(-3.76334323265594,2.43932515890074,4.73452991852249));
#17584=CARTESIAN_POINT('Ctrl Pts',(-3.76655071173719,2.4197416412828,4.73583897743076));
#17585=CARTESIAN_POINT('Ctrl Pts',(-3.76642275699063,2.40011764661364,4.73714803633902));
#17586=CARTESIAN_POINT('Origin',(-3.6,2.4,4.7));
#17587=CARTESIAN_POINT('',(-3.76642910764821,2.39987935508533,4.80714803633902));
#17588=CARTESIAN_POINT('',(-3.76680408556428,2.39990252619421,4.78785196366098));
#17589=CARTESIAN_POINT('',(-3.7666,2.4,4.7));
#17590=CARTESIAN_POINT('Ctrl Pts',(-3.76680408556428,2.39990252619421,4.78785196366098));
#17591=CARTESIAN_POINT('Ctrl Pts',(-3.76646018913848,2.44937641051311,4.78453228558818));
#17592=CARTESIAN_POINT('Ctrl Pts',(-3.74304696564969,2.49913297683607,4.78121260751538));
#17593=CARTESIAN_POINT('Ctrl Pts',(-3.70452480260444,2.53008579208055,4.77789292944258));
#17594=CARTESIAN_POINT('Ctrl Pts',(-3.66153597610701,2.56462760123568,4.77418833309031));
#17595=CARTESIAN_POINT('Ctrl Pts',(-3.59973129998187,2.5757522439241,4.77048373673804));
#17596=CARTESIAN_POINT('Ctrl Pts',(-3.54739603471406,2.55836846433844,4.76677914038578));
#17597=CARTESIAN_POINT('Ctrl Pts',(-3.49506076944624,2.54098468475278,4.76307454403351));
#17598=CARTESIAN_POINT('Ctrl Pts',(-3.45219491503573,2.49509248289304,4.75936994768124));
#17599=CARTESIAN_POINT('Ctrl Pts',(-3.43841627281944,2.44169468516681,4.75566535132897));
#17600=CARTESIAN_POINT('Ctrl Pts',(-3.42463763060315,2.38829688744059,4.7519607549767));
#17601=CARTESIAN_POINT('Ctrl Pts',(-3.43994620058106,2.32739349384788,4.74825615862443));
#17602=CARTESIAN_POINT('Ctrl Pts',(-3.4773359288973,2.28685728781211,4.74455156227217));
#17603=CARTESIAN_POINT('Ctrl Pts',(-3.51472565721353,2.24632108177635,4.7408469659199));
#17604=CARTESIAN_POINT('Ctrl Pts',(-3.57419654386808,2.22615206329753,4.73714236956763));
#17605=CARTESIAN_POINT('Ctrl Pts',(-3.62853140036063,2.23558069804861,4.73343777321536));
#17606=CARTESIAN_POINT('Ctrl Pts',(-3.68286625685319,2.24500933279969,4.7297331768631));
#17607=CARTESIAN_POINT('Ctrl Pts',(-3.73206508318374,2.28403562078066,4.72602858051083));
#17608=CARTESIAN_POINT('Ctrl Pts',(-3.7536117575058,2.33479896000292,4.72232398415856));
#17609=CARTESIAN_POINT('Ctrl Pts',(-3.76228181312143,2.35522535934946,4.72083331065937));
#17610=CARTESIAN_POINT('Ctrl Pts',(-3.76647460984564,2.37755214666628,4.71934263716017));
#17611=CARTESIAN_POINT('Ctrl Pts',(-3.76637219462709,2.39991574862477,4.71785196366098));
#17612=CARTESIAN_POINT('Ctrl Pts',(-3.76642275699063,2.40011764661364,4.73714803633902));
#17613=CARTESIAN_POINT('Ctrl Pts',(-3.76618860374924,2.36420634137441,4.73954357378302));
#17614=CARTESIAN_POINT('Ctrl Pts',(-3.75478479252022,2.32815948710566,4.74193911122702));
#17615=CARTESIAN_POINT('Ctrl Pts',(-3.73334402193678,2.29966496724918,4.74433464867103));
#17616=CARTESIAN_POINT('Ctrl Pts',(-3.70018678588852,2.25559940919069,4.74803924502329));
#17617=CARTESIAN_POINT('Ctrl Pts',(-3.64302585882149,2.22959548666357,4.75174384137557));
#17618=CARTESIAN_POINT('Ctrl Pts',(-3.58802126313241,2.23355404226464,4.75544843772783));
#17619=CARTESIAN_POINT('Ctrl Pts',(-3.53301666744333,2.2375125978657,4.7591530340801));
#17620=CARTESIAN_POINT('Ctrl Pts',(-3.48016840313221,2.27143363159494,4.76285763043237));
#17621=CARTESIAN_POINT('Ctrl Pts',(-3.45366277803107,2.31979299002082,4.76656222678463));
#17622=CARTESIAN_POINT('Ctrl Pts',(-3.42715715292992,2.36815234844671,4.7702668231369));
#17623=CARTESIAN_POINT('Ctrl Pts',(-3.42699416703876,2.43095003156924,4.77397141948917));
#17624=CARTESIAN_POINT('Ctrl Pts',(-3.45324841177486,2.47944632362031,4.77767601584144));
#17625=CARTESIAN_POINT('Ctrl Pts',(-3.47950265651095,2.52794261567138,4.78138061219371));
#17626=CARTESIAN_POINT('Ctrl Pts',(-3.53217413187432,2.56213751665099,4.78508520854598));
#17627=CARTESIAN_POINT('Ctrl Pts',(-3.58715743849732,2.56638153622754,4.78878980489824));
#17628=CARTESIAN_POINT('Ctrl Pts',(-3.64214074512033,2.57062555580409,4.79249440125051));
#17629=CARTESIAN_POINT('Ctrl Pts',(-3.69943588300298,2.54491869397758,4.79619899760278));
#17630=CARTESIAN_POINT('Ctrl Pts',(-3.73282140740775,2.50102584183074,4.79990359395505));
#17631=CARTESIAN_POINT('Ctrl Pts',(-3.754583518131,2.4724146061108,4.80231840808304));
#17632=CARTESIAN_POINT('Ctrl Pts',(-3.76618645992471,2.43607616275589,4.80473322221103));
#17633=CARTESIAN_POINT('Ctrl Pts',(-3.76642910764821,2.39987935508533,4.80714803633902));
#17634=CARTESIAN_POINT('Origin',(-3.6,2.4,4.7));
#17635=CARTESIAN_POINT('',(-3.76685809662611,2.39994994258553,4.87714803633902));
#17636=CARTESIAN_POINT('',(-3.7666675037778,2.40014587506062,4.85785196366098));
#17637=CARTESIAN_POINT('',(-3.7666,2.4,4.7));
#17638=CARTESIAN_POINT('Ctrl Pts',(-3.7666675037778,2.40014587506062,4.85785196366098));
#17639=CARTESIAN_POINT('Ctrl Pts',(-3.76676616841865,2.41091157707528,4.85713112672072));
#17640=CARTESIAN_POINT('Ctrl Pts',(-3.76581236284584,2.4216598706667,4.85641028978047));
#17641=CARTESIAN_POINT('Ctrl Pts',(-3.76374257225157,2.43218878210118,4.85568945284021));
#17642=CARTESIAN_POINT('Ctrl Pts',(-3.7531053001346,2.48630000298229,4.85198485648794));
#17643=CARTESIAN_POINT('Ctrl Pts',(-3.71299219510172,2.53461681652064,4.84828026013567));
#17644=CARTESIAN_POINT('Ctrl Pts',(-3.66176124712798,2.5550267590254,4.8445756637834));
#17645=CARTESIAN_POINT('Ctrl Pts',(-3.61053029915424,2.57543670153016,4.84087106743113));
#17646=CARTESIAN_POINT('Ctrl Pts',(-3.54818150823965,2.56793977300133,4.83716647107887));
#17647=CARTESIAN_POINT('Ctrl Pts',(-3.50324915208796,2.53596698529063,4.8334618747266));
#17648=CARTESIAN_POINT('Ctrl Pts',(-3.45831679593627,2.50399419757992,4.82975727837433));
#17649=CARTESIAN_POINT('Ctrl Pts',(-3.43080087454749,2.44754555068734,4.82605268202206));
#17650=CARTESIAN_POINT('Ctrl Pts',(-3.43329420537107,2.39245508794886,4.8223480856698));
#17651=CARTESIAN_POINT('Ctrl Pts',(-3.43578753619466,2.33736462521039,4.81864348931753));
#17652=CARTESIAN_POINT('Ctrl Pts',(-3.46829011923061,2.28363234662601,4.81493889296526));
#17653=CARTESIAN_POINT('Ctrl Pts',(-3.51592696305034,2.25584913417262,4.81123429661299));
#17654=CARTESIAN_POINT('Ctrl Pts',(-3.56356380687008,2.22806592171924,4.80752970026072));
#17655=CARTESIAN_POINT('Ctrl Pts',(-3.62633491147359,2.22623177539684,4.80382510390846));
#17656=CARTESIAN_POINT('Ctrl Pts',(-3.67551272490272,2.25118610267019,4.80012050755619));
#17657=CARTESIAN_POINT('Ctrl Pts',(-3.72469053833185,2.27614042994354,4.79641591120392));
#17658=CARTESIAN_POINT('Ctrl Pts',(-3.76027506058658,2.32788323081264,4.79271131485165));
#17659=CARTESIAN_POINT('Ctrl Pts',(-3.76598083327909,2.38273411905811,4.78900671849938));
#17660=CARTESIAN_POINT('Ctrl Pts',(-3.76657367957029,2.38843328504628,4.78862180021992));
#17661=CARTESIAN_POINT('Ctrl Pts',(-3.76684396052131,2.39416600535905,4.78823688194045));
#17662=CARTESIAN_POINT('Ctrl Pts',(-3.76680408556428,2.39990252619421,4.78785196366098));
#17663=CARTESIAN_POINT('Ctrl Pts',(-3.76642910764821,2.39987935508533,4.80714803633902));
#17664=CARTESIAN_POINT('Ctrl Pts',(-3.76655870881167,2.38054619044631,4.8084378185633));
#17665=CARTESIAN_POINT('Ctrl Pts',(-3.76344748981416,2.36125343108011,4.80972760078758));
#17666=CARTESIAN_POINT('Ctrl Pts',(-3.75691243582065,2.3432000486953,4.81101738301185));
#17667=CARTESIAN_POINT('Ctrl Pts',(-3.73814202890189,2.29134595017387,4.81472197936412));
#17668=CARTESIAN_POINT('Ctrl Pts',(-3.6911253041375,2.24971659559817,4.81842657571639));
#17669=CARTESIAN_POINT('Ctrl Pts',(-3.63737973221885,2.2373638951443,4.82213117206866));
#17670=CARTESIAN_POINT('Ctrl Pts',(-3.58363416030021,2.22501119469043,4.82583576842093));
#17671=CARTESIAN_POINT('Ctrl Pts',(-3.52315974122731,2.24193514835838,4.82954036477319));
#17672=CARTESIAN_POINT('Ctrl Pts',(-3.48363293580215,2.28039041278662,4.83324496112546));
#17673=CARTESIAN_POINT('Ctrl Pts',(-3.44410613037699,2.31884567721486,4.83694955747773));
#17674=CARTESIAN_POINT('Ctrl Pts',(-3.42552693859956,2.3788322524034,4.84065415383));
#17675=CARTESIAN_POINT('Ctrl Pts',(-3.436398232938,2.43289694207027,4.84435875018227));
#17676=CARTESIAN_POINT('Ctrl Pts',(-3.44726952727644,2.48696163173715,4.84806334653453));
#17677=CARTESIAN_POINT('Ctrl Pts',(-3.48759130773074,2.53510443588236,4.8517679428868));
#17678=CARTESIAN_POINT('Ctrl Pts',(-3.53891008283594,2.5552925272004,4.85547253923907));
#17679=CARTESIAN_POINT('Ctrl Pts',(-3.59022885794113,2.57548061851844,4.85917713559134));
#17680=CARTESIAN_POINT('Ctrl Pts',(-3.65254462769722,2.56771399700931,4.86288173194361));
#17681=CARTESIAN_POINT('Ctrl Pts',(-3.6973382267209,2.53554710104677,4.86658632829587));
#17682=CARTESIAN_POINT('Ctrl Pts',(-3.73990668943618,2.50497810589362,4.87010689764359));
#17683=CARTESIAN_POINT('Ctrl Pts',(-3.76665058188897,2.4523728080809,4.8736274669913));
#17684=CARTESIAN_POINT('Ctrl Pts',(-3.76685809662611,2.39994994258553,4.87714803633902));
#17685=CARTESIAN_POINT('Origin',(-3.6,2.4,4.7));
#17686=CARTESIAN_POINT('',(-3.76657659596252,2.40015219042981,4.94714803633902));
#17687=CARTESIAN_POINT('',(-3.76633013671136,2.4000063325357,4.92785196366098));
#17688=CARTESIAN_POINT('',(-3.7666,2.4,4.7));
#17689=CARTESIAN_POINT('Ctrl Pts',(-3.76633013671136,2.4000063325357,4.92785196366098));
#17690=CARTESIAN_POINT('Ctrl Pts',(-3.76633943338483,2.42742681836579,4.926025371501));
#17691=CARTESIAN_POINT('Ctrl Pts',(-3.75993532163491,2.454843216144,4.92419877934102));
#17692=CARTESIAN_POINT('Ctrl Pts',(-3.74709395519472,2.478810633836,4.92237218718103));
#17693=CARTESIAN_POINT('Ctrl Pts',(-3.72104978380566,2.52742006625356,4.91866759082877));
#17694=CARTESIAN_POINT('Ctrl Pts',(-3.66852675119931,2.56184254018683,4.9149629944765));
#17695=CARTESIAN_POINT('Ctrl Pts',(-3.61356232107187,2.56632441524918,4.91125839812423));
#17696=CARTESIAN_POINT('Ctrl Pts',(-3.55859789094443,2.57080629031153,4.90755380177196));
#17697=CARTESIAN_POINT('Ctrl Pts',(-3.5011920632959,2.54534756650297,4.90384920541969));
#17698=CARTESIAN_POINT('Ctrl Pts',(-3.46761694066379,2.50159957313644,4.90014460906742));
#17699=CARTESIAN_POINT('Ctrl Pts',(-3.43404181803167,2.45785157976992,4.89644001271516));
#17700=CARTESIAN_POINT('Ctrl Pts',(-3.42429740041597,2.39581431684543,4.89273541636289));
#17701=CARTESIAN_POINT('Ctrl Pts',(-3.44284327579263,2.34387948951498,4.88903082001062));
#17702=CARTESIAN_POINT('Ctrl Pts',(-3.46138915116929,2.29194466218454,4.88532622365835));
#17703=CARTESIAN_POINT('Ctrl Pts',(-3.50822531953831,2.25011227044814,4.88162162730609));
#17704=CARTESIAN_POINT('Ctrl Pts',(-3.56191694286671,2.23752714559004,4.87791703095382));
#17705=CARTESIAN_POINT('Ctrl Pts',(-3.61560856619511,2.22494202073194,4.87421243460155));
#17706=CARTESIAN_POINT('Ctrl Pts',(-3.6761556444829,2.24160416275214,4.87050783824928));
#17707=CARTESIAN_POINT('Ctrl Pts',(-3.71584846402625,2.27988804787417,4.86680324189701));
#17708=CARTESIAN_POINT('Ctrl Pts',(-3.7478178913646,2.31072268995097,4.863819482485));
#17709=CARTESIAN_POINT('Ctrl Pts',(-3.76625910135787,2.35558341867251,4.86083572307299));
#17710=CARTESIAN_POINT('Ctrl Pts',(-3.7666675037778,2.40014587506062,4.85785196366098));
#17711=CARTESIAN_POINT('Ctrl Pts',(-3.76685809662611,2.39994994258553,4.87714803633902));
#17712=CARTESIAN_POINT('Ctrl Pts',(-3.76686894382487,2.39720969748472,4.87733206334357));
#17713=CARTESIAN_POINT('Ctrl Pts',(-3.76680728418873,2.39446995085397,4.87751609034812));
#17714=CARTESIAN_POINT('Ctrl Pts',(-3.76667158779769,2.39173387609673,4.87770011735268));
#17715=CARTESIAN_POINT('Ctrl Pts',(-3.76393992155949,2.33665471752516,4.88140471370494));
#17716=CARTESIAN_POINT('Ctrl Pts',(-3.73120516079181,2.28306357079796,4.88510931005722));
#17717=CARTESIAN_POINT('Ctrl Pts',(-3.68344855437882,2.25548672809881,4.88881390640948));
#17718=CARTESIAN_POINT('Ctrl Pts',(-3.63569194796583,2.22790988539967,4.89251850276175));
#17719=CARTESIAN_POINT('Ctrl Pts',(-3.57291349590753,2.22634734672859,4.89622309911402));
#17720=CARTESIAN_POINT('Ctrl Pts',(-3.52384411276617,2.25151421676554,4.89992769546629));
#17721=CARTESIAN_POINT('Ctrl Pts',(-3.47477472962482,2.27668108680249,4.90363229181855));
#17722=CARTESIAN_POINT('Ctrl Pts',(-3.43941441540042,2.32857736554749,4.90733688817082));
#17723=CARTESIAN_POINT('Ctrl Pts',(-3.43394601840489,2.38345242676704,4.91104148452309));
#17724=CARTESIAN_POINT('Ctrl Pts',(-3.42847762140937,2.4383274879866,4.91474608087536));
#17725=CARTESIAN_POINT('Ctrl Pts',(-3.45290114164273,2.49618133168073,4.91845067722763));
#17726=CARTESIAN_POINT('Ctrl Pts',(-3.49603901657836,2.530536818217,4.9221552735799));
#17727=CARTESIAN_POINT('Ctrl Pts',(-3.539176891514,2.56489230475327,4.92585986993216));
#17728=CARTESIAN_POINT('Ctrl Pts',(-3.60102912115191,2.5757494341317,4.92956446628443));
#17729=CARTESIAN_POINT('Ctrl Pts',(-3.65328868187437,2.55813937955255,4.9332690626367));
#17730=CARTESIAN_POINT('Ctrl Pts',(-3.70554824259683,2.54052932497339,4.93697365898897));
#17731=CARTESIAN_POINT('Ctrl Pts',(-3.74821513440384,2.49445208643666,4.94067825534123));
#17732=CARTESIAN_POINT('Ctrl Pts',(-3.76176261231807,2.4409951733855,4.9443828516935));
#17733=CARTESIAN_POINT('Ctrl Pts',(-3.76513331494005,2.42769473782655,4.94530457990868));
#17734=CARTESIAN_POINT('Ctrl Pts',(-3.7667013875235,2.41393746536136,4.94622630812385));
#17735=CARTESIAN_POINT('Ctrl Pts',(-3.76657659596252,2.40015219042981,4.94714803633902));
#17736=CARTESIAN_POINT('Origin',(-3.6,2.4,4.7));
#17737=CARTESIAN_POINT('',(-3.76634000089015,2.39995738785102,5.01714803633902));
#17738=CARTESIAN_POINT('',(-3.76664425875303,2.39985083704439,4.99785196366098));
#17739=CARTESIAN_POINT('',(-3.7666,2.4,4.7));
#17740=CARTESIAN_POINT('Ctrl Pts',(-3.76664425875303,2.39985083704439,4.99785196366098));
#17741=CARTESIAN_POINT('Ctrl Pts',(-3.76623994328637,2.44366117230771,4.99491961628127));
#17742=CARTESIAN_POINT('Ctrl Pts',(-3.74849621432459,2.48776127465667,4.99198726890157));
#17743=CARTESIAN_POINT('Ctrl Pts',(-3.71750016303509,2.5184966637895,4.98905492152186));
#17744=CARTESIAN_POINT('Ctrl Pts',(-3.67834114001603,2.55732637791376,4.98535032516959));
#17745=CARTESIAN_POINT('Ctrl Pts',(-3.61803053064114,2.57482512236184,4.98164572881732));
#17746=CARTESIAN_POINT('Ctrl Pts',(-3.56416982715023,2.56298449736068,4.97794113246505));
#17747=CARTESIAN_POINT('Ctrl Pts',(-3.51030912365932,2.55114387235952,4.97423653611279));
#17748=CARTESIAN_POINT('Ctrl Pts',(-3.46289832605237,2.50996387790913,4.97053193976052));
#17749=CARTESIAN_POINT('Ctrl Pts',(-3.44363525475417,2.45829077205198,4.96682734340825));
#17750=CARTESIAN_POINT('Ctrl Pts',(-3.42437218345597,2.40661766619482,4.96312274705598));
#17751=CARTESIAN_POINT('Ctrl Pts',(-3.4332568384665,2.34445144893089,4.95941815070372));
#17752=CARTESIAN_POINT('Ctrl Pts',(-3.4662231070096,2.30024284205961,4.95571355435145));
#17753=CARTESIAN_POINT('Ctrl Pts',(-3.4991893755527,2.25603423518832,4.95200895799918));
#17754=CARTESIAN_POINT('Ctrl Pts',(-3.55623725762836,2.22978323870968,4.94830436164691));
#17755=CARTESIAN_POINT('Ctrl Pts',(-3.61125846653673,2.23350377003431,4.94459976529464));
#17756=CARTESIAN_POINT('Ctrl Pts',(-3.66627967544511,2.23722430135893,4.94089516894237));
#17757=CARTESIAN_POINT('Ctrl Pts',(-3.71927421118621,2.27091636048683,4.9371905725901));
#17758=CARTESIAN_POINT('Ctrl Pts',(-3.74598882397087,2.31916058550171,4.93348597623784));
#17759=CARTESIAN_POINT('Ctrl Pts',(-3.75953150177818,2.3436174623693,4.93160797204555));
#17760=CARTESIAN_POINT('Ctrl Pts',(-3.76632057836981,2.37181405816179,4.92972996785327));
#17761=CARTESIAN_POINT('Ctrl Pts',(-3.76633013671136,2.4000063325357,4.92785196366098));
#17762=CARTESIAN_POINT('Ctrl Pts',(-3.76657659596252,2.40015219042981,4.94714803633902));
#17763=CARTESIAN_POINT('Ctrl Pts',(-3.76619982713509,2.35853189310505,4.94993090447612));
#17764=CARTESIAN_POINT('Ctrl Pts',(-3.7503917908276,2.31665633988757,4.95271377261321));
#17765=CARTESIAN_POINT('Ctrl Pts',(-3.72217338919013,2.28632762005297,4.95549664075031));
#17766=CARTESIAN_POINT('Ctrl Pts',(-3.68460862412651,2.24595356733716,4.95920123710258));
#17767=CARTESIAN_POINT('Ctrl Pts',(-3.62505102997782,2.22604204947114,4.96290583345484));
#17768=CARTESIAN_POINT('Ctrl Pts',(-3.57075747740423,2.23570568531624,4.96661042980711));
#17769=CARTESIAN_POINT('Ctrl Pts',(-3.51646392483064,2.24536932116134,4.97031502615938));
#17770=CARTESIAN_POINT('Ctrl Pts',(-3.46743441383215,2.28460811071757,4.97401962251165));
#17771=CARTESIAN_POINT('Ctrl Pts',(-3.44610757816651,2.33546419983794,4.97772421886392));
#17772=CARTESIAN_POINT('Ctrl Pts',(-3.42478074250087,2.38632028895831,4.98142881521618));
#17773=CARTESIAN_POINT('Ctrl Pts',(-3.43115658216808,2.44879367764282,4.98513341156845));
#17774=CARTESIAN_POINT('Ctrl Pts',(-3.46231715792478,2.49429306452592,4.98883800792072));
#17775=CARTESIAN_POINT('Ctrl Pts',(-3.49347773368148,2.53979245140902,4.99254260427299));
#17776=CARTESIAN_POINT('Ctrl Pts',(-3.54942304552767,2.56831783649071,4.99624720062526));
#17777=CARTESIAN_POINT('Ctrl Pts',(-3.60454940439799,2.56681441711196,4.99995179697753));
#17778=CARTESIAN_POINT('Ctrl Pts',(-3.6596757632683,2.5653109977332,5.00365639332979));
#17779=CARTESIAN_POINT('Ctrl Pts',(-3.71398316916273,2.533778773894,5.00736098968206));
#17780=CARTESIAN_POINT('Ctrl Pts',(-3.7426175295644,2.48664864348361,5.01106558603433));
#17781=CARTESIAN_POINT('Ctrl Pts',(-3.75828878922747,2.46085485932866,5.01309306946923));
#17782=CARTESIAN_POINT('Ctrl Pts',(-3.76627033413891,2.43038911475947,5.01512055290412));
#17783=CARTESIAN_POINT('Ctrl Pts',(-3.76634000089015,2.39995738785102,5.01714803633902));
#17784=CARTESIAN_POINT('Origin',(-3.6,2.4,4.7));
#17785=CARTESIAN_POINT('',(-3.76673280722786,2.39986996770474,5.08714803633902));
#17786=CARTESIAN_POINT('',(-3.76682061973634,2.40008640134019,5.06785196366098));
#17787=CARTESIAN_POINT('',(-3.7666,2.4,4.7));
#17788=CARTESIAN_POINT('Ctrl Pts',(-3.76682061973634,2.40008640134019,5.06785196366098));
#17789=CARTESIAN_POINT('Ctrl Pts',(-3.76685198409984,2.40505542063702,5.06751845741382));
#17790=CARTESIAN_POINT('Ctrl Pts',(-3.76664920930319,2.41002184448446,5.06718495116665));
#17791=CARTESIAN_POINT('Ctrl Pts',(-3.76620395659798,2.41496643342036,5.06685144491949));
#17792=CARTESIAN_POINT('Ctrl Pts',(-3.76125807758801,2.46989106014367,5.06314684856722));
#17793=CARTESIAN_POINT('Ctrl Pts',(-3.7263932711654,2.5221215151067,5.05944225221495));
#17794=CARTESIAN_POINT('Ctrl Pts',(-3.67756562981921,2.54775425401002,5.05573765586269));
#17795=CARTESIAN_POINT('Ctrl Pts',(-3.62873798847301,2.57338699291335,5.05203305951042));
#17796=CARTESIAN_POINT('Ctrl Pts',(-3.56594751220322,2.57242201575698,5.04832846315815));
#17797=CARTESIAN_POINT('Ctrl Pts',(-3.51793061046379,2.54530094002895,5.04462386680588));
#17798=CARTESIAN_POINT('Ctrl Pts',(-3.46991370872435,2.51817986430092,5.04091927045361));
#17799=CARTESIAN_POINT('Ctrl Pts',(-3.43667038151527,2.46490269000124,5.03721467410135));
#17800=CARTESIAN_POINT('Ctrl Pts',(-3.4334146300602,2.40985202293434,5.03351007774908));
#17801=CARTESIAN_POINT('Ctrl Pts',(-3.43015887860513,2.35480135586744,5.02980548139681));
#17802=CARTESIAN_POINT('Ctrl Pts',(-3.45689070290407,2.29797719603331,5.02610088504454));
#17803=CARTESIAN_POINT('Ctrl Pts',(-3.50137612997721,2.26538543995573,5.02239628869227));
#17804=CARTESIAN_POINT('Ctrl Pts',(-3.54586155705034,2.23279368387816,5.01869169234));
#17805=CARTESIAN_POINT('Ctrl Pts',(-3.60810058689768,2.22443433155712,5.01498709598773));
#17806=CARTESIAN_POINT('Ctrl Pts',(-3.65960917559394,2.24413308920132,5.01128249963547));
#17807=CARTESIAN_POINT('Ctrl Pts',(-3.7111177642902,2.26383184684551,5.0075779032832));
#17808=CARTESIAN_POINT('Ctrl Pts',(-3.75189591183539,2.31158871445493,5.00387330693093));
#17809=CARTESIAN_POINT('Ctrl Pts',(-3.76328126727638,2.36554749015986,5.00016871057866));
#17810=CARTESIAN_POINT('Ctrl Pts',(-3.76565462410273,2.37679557365843,4.9993964616061));
#17811=CARTESIAN_POINT('Ctrl Pts',(-3.76675073733939,2.38831315681292,4.99862421263354));
#17812=CARTESIAN_POINT('Ctrl Pts',(-3.76664425875303,2.39985083704439,4.99785196366098));
#17813=CARTESIAN_POINT('Ctrl Pts',(-3.76634000089015,2.39995738785102,5.01714803633902));
#17814=CARTESIAN_POINT('Ctrl Pts',(-3.76639762849214,2.37478458425737,5.01882514925639));
#17815=CARTESIAN_POINT('Ctrl Pts',(-3.76104161363815,2.34963505698934,5.02050226217376));
#17816=CARTESIAN_POINT('Ctrl Pts',(-3.75014621226255,2.32717238066401,5.02217937509113));
#17817=CARTESIAN_POINT('Ctrl Pts',(-3.72607921965016,2.27755428523638,5.0258839714434));
#17818=CARTESIAN_POINT('Ctrl Pts',(-3.67498391951647,2.2410461313627,5.02958856779567));
#17819=CARTESIAN_POINT('Ctrl Pts',(-3.62024436463387,2.23435607004762,5.03329316414794));
#17820=CARTESIAN_POINT('Ctrl Pts',(-3.56550480975127,2.22766600873255,5.03699776050021));
#17821=CARTESIAN_POINT('Ctrl Pts',(-3.50712100011975,2.25079403997609,5.04070235685247));
#17822=CARTESIAN_POINT('Ctrl Pts',(-3.47181261940603,2.29315551442515,5.04440695320474));
#17823=CARTESIAN_POINT('Ctrl Pts',(-3.43650423869231,2.33551698887421,5.04811154955701));
#17824=CARTESIAN_POINT('Ctrl Pts',(-3.42427128689639,2.39711190652879,5.05181614590928));
#17825=CARTESIAN_POINT('Ctrl Pts',(-3.44071223950815,2.44975095341954,5.05552074226154));
#17826=CARTESIAN_POINT('Ctrl Pts',(-3.45715319211991,2.50239000031029,5.05922533861381));
#17827=CARTESIAN_POINT('Ctrl Pts',(-3.50226804913935,2.54607317643722,5.06292993496608));
#17828=CARTESIAN_POINT('Ctrl Pts',(-3.55540974897266,2.56080872993518,5.06663453131835));
#17829=CARTESIAN_POINT('Ctrl Pts',(-3.60855144880598,2.57554428343315,5.07033912767062));
#17830=CARTESIAN_POINT('Ctrl Pts',(-3.66971999145316,2.56133221430215,5.07404372402289));
#17831=CARTESIAN_POINT('Ctrl Pts',(-3.71092122942369,2.52467655355957,5.07774832037516));
#17832=CARTESIAN_POINT('Ctrl Pts',(-3.74576802490479,2.49367427362722,5.08088155902978));
#17833=CARTESIAN_POINT('Ctrl Pts',(-3.76633165033452,2.44661746651941,5.0840147976844));
#17834=CARTESIAN_POINT('Ctrl Pts',(-3.76673280722786,2.39986996770474,5.08714803633902));
#17835=CARTESIAN_POINT('Origin',(-3.6,2.4,4.7));
#17836=CARTESIAN_POINT('',(-3.76674783252531,2.40012156540224,5.15714803633902));
#17837=CARTESIAN_POINT('',(-3.76638442018051,2.4000942147675,5.13785196366098));
#17838=CARTESIAN_POINT('',(-3.7666,2.4,4.7));
#17839=CARTESIAN_POINT('',(-3.47309291201476,2.50793586530485,5.2));
#17840=CARTESIAN_POINT('Ctrl Pts',(-3.76674783252531,2.40012156540224,5.15714803633902));
#17841=CARTESIAN_POINT('Ctrl Pts',(-3.76635429688688,2.35284438834095,5.16031823516921));
#17842=CARTESIAN_POINT('Ctrl Pts',(-3.74524547308137,2.30526839815283,5.1634884339994));
#17843=CARTESIAN_POINT('Ctrl Pts',(-3.70967617106781,2.27424023606977,5.16665863282959));
#17844=CARTESIAN_POINT('Ctrl Pts',(-3.66811098429235,2.23798168503636,5.17036322918186));
#17845=CARTESIAN_POINT('Ctrl Pts',(-3.60679923783928,2.22432008207827,5.17406782553412));
#17846=CARTESIAN_POINT('Ctrl Pts',(-3.55380863333633,2.23961508023379,5.17777242188639));
#17847=CARTESIAN_POINT('Ctrl Pts',(-3.50081802883339,2.2549100783893,5.18147701823866));
#17848=CARTESIAN_POINT('Ctrl Pts',(-3.45614856628056,2.29916167765842,5.18518161459093));
#17849=CARTESIAN_POINT('Ctrl Pts',(-3.44024447629705,2.35186821788708,5.1888862109432));
#17850=CARTESIAN_POINT('Ctrl Pts',(-3.42434038631354,2.40457475811575,5.19259080729547));
#17851=CARTESIAN_POINT('Ctrl Pts',(-3.43720166889934,2.46573623930395,5.19629540364773));
#17852=CARTESIAN_POINT('Ctrl Pts',(-3.47309291201476,2.50793586530485,5.2));
#17853=CARTESIAN_POINT('',(-3.72714753727462,2.50812032359617,5.2));
#17854=CARTESIAN_POINT('Origin',(-3.6,2.4,5.2));
#17855=CARTESIAN_POINT('Ctrl Pts',(-3.72714768981588,2.50812044061668,5.2));
#17856=CARTESIAN_POINT('Ctrl Pts',(-3.69206189497277,2.54927257104909,5.19636770818145));
#17857=CARTESIAN_POINT('Ctrl Pts',(-3.63506413165932,2.57187758396405,5.19273541636289));
#17858=CARTESIAN_POINT('Ctrl Pts',(-3.58132375091077,2.56581791151438,5.18910312454434));
#17859=CARTESIAN_POINT('Ctrl Pts',(-3.52651361217864,2.55963761500343,5.18539852819207));
#17860=CARTESIAN_POINT('Ctrl Pts',(-3.475091829903,2.5236400741886,5.1816939318398));
#17861=CARTESIAN_POINT('Ctrl Pts',(-3.45055836676857,2.47425895866487,5.17798933548753));
#17862=CARTESIAN_POINT('Ctrl Pts',(-3.42602490363414,2.42487784314114,5.17428473913526));
#17863=CARTESIAN_POINT('Ctrl Pts',(-3.42837975964092,2.3621131529085,5.17058014278299));
#17864=CARTESIAN_POINT('Ctrl Pts',(-3.4565619363393,2.31470980183002,5.16687554643073));
#17865=CARTESIAN_POINT('Ctrl Pts',(-3.48474411303769,2.26730645075154,5.16317095007846));
#17866=CARTESIAN_POINT('Ctrl Pts',(-3.53875361042767,2.23526443882722,5.15946635372619));
#17867=CARTESIAN_POINT('Ctrl Pts',(-3.59386432951576,2.23323784347702,5.15576175737392));
#17868=CARTESIAN_POINT('Ctrl Pts',(-3.64897504860385,2.23121124812682,5.15205716102166));
#17869=CARTESIAN_POINT('Ctrl Pts',(-3.70518698939006,2.25920006935074,5.14835256466939));
#17870=CARTESIAN_POINT('Ctrl Pts',(-3.73677860664843,2.30440012364175,5.14464796831712));
#17871=CARTESIAN_POINT('Ctrl Pts',(-3.75609666072391,2.3320396422478,5.14238263343174));
#17872=CARTESIAN_POINT('Ctrl Pts',(-3.76620859139621,2.36611484945711,5.14011729854636));
#17873=CARTESIAN_POINT('Ctrl Pts',(-3.76638442018051,2.4000942147675,5.13785196366098));
#17874=CARTESIAN_POINT('Origin',(-3.6,2.4,5.35459252805377));
#17875=CARTESIAN_POINT('',(-3.80572269346025,2.40011955618633,4.34540747194623));
#17876=CARTESIAN_POINT('',(-3.8051611014991,2.39991986595833,4.33959252805377));
#17877=CARTESIAN_POINT('',(-3.805475,2.40000000000001,5.35459252805377));
#17878=CARTESIAN_POINT('',(-3.41173724903364,2.31767678198965,4.3));
#17879=CARTESIAN_POINT('Ctrl Pts',(-3.8051611014991,2.39991986595833,4.33959252805377));
#17880=CARTESIAN_POINT('Ctrl Pts',(-3.80504328807488,2.43847991504582,4.33750880775932));
#17881=CARTESIAN_POINT('Ctrl Pts',(-3.77605831390311,2.54576383181508,4.33172049111259));
#17882=CARTESIAN_POINT('Ctrl Pts',(-3.60297477126067,2.64299057240655,4.32222757811361));
#17883=CARTESIAN_POINT('Ctrl Pts',(-3.39749753058122,2.53388381093044,4.3111137890568));
#17884=CARTESIAN_POINT('Ctrl Pts',(-3.38436282049399,2.380278625644,4.30370459635227));
#17885=CARTESIAN_POINT('Ctrl Pts',(-3.41173724903364,2.31767678198965,4.3));
#17886=CARTESIAN_POINT('',(-3.47764162137361,2.23446466486417,4.3));
#17887=CARTESIAN_POINT('Origin',(-3.6,2.4,4.3));
#17888=CARTESIAN_POINT('Ctrl Pts',(-3.80572269346025,2.40011955618633,4.34540747194623));
#17889=CARTESIAN_POINT('Ctrl Pts',(-3.80577296183019,2.40728359294699,4.34501772883951));
#17890=CARTESIAN_POINT('Ctrl Pts',(-3.80218372831243,2.48249299452007,4.34092338938053));
#17891=CARTESIAN_POINT('Ctrl Pts',(-3.70962996035205,2.61673302206395,4.33312445356927));
#17892=CARTESIAN_POINT('Ctrl Pts',(-3.47734458963256,2.60960762555316,4.32201066451247));
#17893=CARTESIAN_POINT('Ctrl Pts',(-3.35820165688085,2.41200908723629,4.31096917998938));
#17894=CARTESIAN_POINT('Ctrl Pts',(-3.42405717417692,2.27417969332383,4.30363229181855));
#17895=CARTESIAN_POINT('Ctrl Pts',(-3.477641490197,2.23446446733471,4.3));
#17896=CARTESIAN_POINT('Origin',(-3.6,2.4,5.35459252805377));
#17897=CARTESIAN_POINT('',(-3.8051926580795,2.40010265427736,4.41540747194623));
#17898=CARTESIAN_POINT('',(-3.80566724099481,2.39985021907517,4.40959252805377));
#17899=CARTESIAN_POINT('',(-3.805475,2.40000000000001,5.35459252805377));
#17900=CARTESIAN_POINT('Ctrl Pts',(-3.80566724099481,2.39985021907517,4.40959252805377));
#17901=CARTESIAN_POINT('Ctrl Pts',(-3.80518613776288,2.45851948579172,4.40640305253959));
#17902=CARTESIAN_POINT('Ctrl Pts',(-3.74813828696622,2.58615032985374,4.39950898067314));
#17903=CARTESIAN_POINT('Ctrl Pts',(-3.53156902199863,2.63302754596983,4.38891031245443));
#17904=CARTESIAN_POINT('Ctrl Pts',(-3.36710794775451,2.46888245639993,4.37779652339763));
#17905=CARTESIAN_POINT('Ctrl Pts',(-3.41581895566904,2.24170428297288,4.36668273434082));
#17906=CARTESIAN_POINT('Ctrl Pts',(-3.63310626324856,2.15938431915927,4.35556894528402));
#17907=CARTESIAN_POINT('Ctrl Pts',(-3.78504422722635,2.27149586782626,4.34653887652167));
#17908=CARTESIAN_POINT('Ctrl Pts',(-3.80525274573711,2.36992492828818,4.34121340411158));
#17909=CARTESIAN_POINT('Ctrl Pts',(-3.8051611014991,2.39991986595833,4.33959252805377));
#17910=CARTESIAN_POINT('Ctrl Pts',(-3.8051926580795,2.40010265427736,4.41540747194623));
#17911=CARTESIAN_POINT('Ctrl Pts',(-3.80531782228225,2.42777437777342,4.41391197361979));
#17912=CARTESIAN_POINT('Ctrl Pts',(-3.78721617252902,2.52383659362796,4.40871187894108));
#17913=CARTESIAN_POINT('Ctrl Pts',(-3.64121277856108,2.63934345799643,4.3998071879101));
#17914=CARTESIAN_POINT('Ctrl Pts',(-3.4212652433475,2.56443108225311,4.38869339885329));
#17915=CARTESIAN_POINT('Ctrl Pts',(-3.36491712045917,2.33901445477475,4.3775796097965));
#17916=CARTESIAN_POINT('Ctrl Pts',(-3.52374009472539,2.16941582002738,4.36646582073968));
#17917=CARTESIAN_POINT('Ctrl Pts',(-3.7443527804805,2.20942499341216,4.3557417747896));
#17918=CARTESIAN_POINT('Ctrl Pts',(-3.80529514960796,2.33918780371163,4.34872232519178));
#17919=CARTESIAN_POINT('Ctrl Pts',(-3.80572269346025,2.40011955618633,4.34540747194623));
#17920=CARTESIAN_POINT('Origin',(-3.6,2.4,5.35459252805377));
#17921=CARTESIAN_POINT('',(-3.80534990670044,2.39982347234431,4.48540747194623));
#17922=CARTESIAN_POINT('',(-3.80562878067403,2.40016339023914,4.47959252805377));
#17923=CARTESIAN_POINT('',(-3.805475,2.40000000000001,5.35459252805377));
#17924=CARTESIAN_POINT('Ctrl Pts',(-3.80562878067403,2.40016339023914,4.47959252805377));
#17925=CARTESIAN_POINT('Ctrl Pts',(-3.80572325245773,2.41103322160878,4.47900189367213));
#17926=CARTESIAN_POINT('Ctrl Pts',(-3.79999615010417,2.4899814340984,4.47470666293823));
#17927=CARTESIAN_POINT('Ctrl Pts',(-3.69773850528383,2.62233049702197,4.46670683585206));
#17928=CARTESIAN_POINT('Ctrl Pts',(-3.46621554861493,2.60269535293104,4.45559304679526));
#17929=CARTESIAN_POINT('Ctrl Pts',(-3.35714699158608,2.39753073103871,4.44447925773845));
#17930=CARTESIAN_POINT('Ctrl Pts',(-3.47036459922058,2.19462650439043,4.43336546868165));
#17931=CARTESIAN_POINT('Ctrl Pts',(-3.70223885539349,2.17970247609322,4.42225167962484));
#17932=CARTESIAN_POINT('Ctrl Pts',(-3.80084479883202,2.31283530811152,4.41432736608222));
#17933=CARTESIAN_POINT('Ctrl Pts',(-3.80574494226542,2.39037475462753,4.41010764889186));
#17934=CARTESIAN_POINT('Ctrl Pts',(-3.80566724099481,2.39985021907517,4.40959252805377));
#17935=CARTESIAN_POINT('Ctrl Pts',(-3.80534990670044,2.39982347234431,4.48540747194623));
#17936=CARTESIAN_POINT('Ctrl Pts',(-3.804956326745,2.4478627067473,4.48280621840006));
#17937=CARTESIAN_POINT('Ctrl Pts',(-3.76418777279803,2.56491922132028,4.47650036850163));
#17938=CARTESIAN_POINT('Ctrl Pts',(-3.56918135753979,2.64090223654315,4.46648992225092));
#17939=CARTESIAN_POINT('Ctrl Pts',(-3.38089014394226,2.50475947474088,4.45537613319412));
#17940=CARTESIAN_POINT('Ctrl Pts',(-3.3931526891646,2.27272919910994,4.44426234413731));
#17941=CARTESIAN_POINT('Ctrl Pts',(-3.59474487835949,2.15719128792351,4.43314855508051));
#17942=CARTESIAN_POINT('Ctrl Pts',(-3.77337323137102,2.2495401787091,4.42353026435015));
#17943=CARTESIAN_POINT('Ctrl Pts',(-3.80500776987982,2.35922694839029,4.41761656997206));
#17944=CARTESIAN_POINT('Ctrl Pts',(-3.8051926580795,2.40010265427736,4.41540747194623));
#17945=CARTESIAN_POINT('Origin',(-3.6,2.4,5.35459252805377));
#17946=CARTESIAN_POINT('',(-3.80581594817644,2.40000082772184,4.55540747194624));
#17947=CARTESIAN_POINT('',(-3.80515175559583,2.40004689761323,4.54959252805377));
#17948=CARTESIAN_POINT('',(-3.805475,2.40000000000001,5.35459252805377));
#17949=CARTESIAN_POINT('Ctrl Pts',(-3.80515175559583,2.40004689761323,4.54959252805377));
#17950=CARTESIAN_POINT('Ctrl Pts',(-3.80521586484871,2.43145144073697,4.54789613845241));
#17951=CARTESIAN_POINT('Ctrl Pts',(-3.78367650680796,2.53135422698056,4.54249515249878));
#17952=CARTESIAN_POINT('Ctrl Pts',(-3.62821111800771,2.64122148806661,4.53338957019289));
#17953=CARTESIAN_POINT('Ctrl Pts',(-3.41263638408026,2.55452685581013,4.52227578113608));
#17954=CARTESIAN_POINT('Ctrl Pts',(-3.36855769224962,2.32639203807509,4.51116199207928));
#17955=CARTESIAN_POINT('Ctrl Pts',(-3.536320770243,2.1656314264689,4.50004820302247));
#17956=CARTESIAN_POINT('Ctrl Pts',(-3.75035693400944,2.21653400528296,4.48952504834731));
#17957=CARTESIAN_POINT('Ctrl Pts',(-3.80513070343558,2.34285510855967,4.4827064900244));
#17958=CARTESIAN_POINT('Ctrl Pts',(-3.80562878067403,2.40016339023914,4.47959252805377));
#17959=CARTESIAN_POINT('Ctrl Pts',(-3.80581594649383,2.40000082771776,4.55540747194623));
#17960=CARTESIAN_POINT('Ctrl Pts',(-3.80581594913922,2.4000451187351,4.55540505953261));
#17961=CARTESIAN_POINT('Ctrl Pts',(-3.80579587912807,2.46810441912583,4.55169805076672));
#17962=CARTESIAN_POINT('Ctrl Pts',(-3.73158417538336,2.60413054603043,4.54428644564855));
#17963=CARTESIAN_POINT('Ctrl Pts',(-3.49986236476522,2.62126031969194,4.53317265659175));
#17964=CARTESIAN_POINT('Ctrl Pts',(-3.35979766713961,2.43586801331045,4.52205886753494));
#17965=CARTESIAN_POINT('Ctrl Pts',(-3.43959288921302,2.2176453079079,4.51094507847814));
#17966=CARTESIAN_POINT('Ctrl Pts',(-3.66621055822496,2.16633391955349,4.49983128942134));
#17967=CARTESIAN_POINT('Ctrl Pts',(-3.79336822071197,2.29085017253336,4.4913187539107));
#17968=CARTESIAN_POINT('Ctrl Pts',(-3.80551684683325,2.37944724113564,4.48651081475233));
#17969=CARTESIAN_POINT('Ctrl Pts',(-3.80534990670044,2.39982347234431,4.48540747194623));
#17970=CARTESIAN_POINT('Origin',(-3.6,2.4,5.35459252805377));
#17971=CARTESIAN_POINT('',(-3.80534749188876,2.40017600730441,4.62540747194623));
#17972=CARTESIAN_POINT('',(-3.80545679372687,2.39981210841117,4.61959252805377));
#17973=CARTESIAN_POINT('',(-3.805475,2.40000000000001,5.35459252805377));
#17974=CARTESIAN_POINT('Ctrl Pts',(-3.80545679372687,2.39981210841117,4.61959252805377));
#17975=CARTESIAN_POINT('Ctrl Pts',(-3.80498629190864,2.45149295693423,4.61679038323268));
#17976=CARTESIAN_POINT('Ctrl Pts',(-3.75902063818539,2.5722445101987,4.61028364205933));
#17977=CARTESIAN_POINT('Ctrl Pts',(-3.55620097488638,2.63888348417682,4.60007230453371));
#17978=CARTESIAN_POINT('Ctrl Pts',(-3.3755463800872,2.4927590756963,4.58895851547691));
#17979=CARTESIAN_POINT('Ctrl Pts',(-3.40033672906513,2.26173123324197,4.5778447264201));
#17980=CARTESIAN_POINT('Ctrl Pts',(-3.60788113427776,2.15726236113484,4.5667309373633));
#17981=CARTESIAN_POINT('Ctrl Pts',(-3.77763371313004,2.25700670057819,4.55731353790785));
#17982=CARTESIAN_POINT('Ctrl Pts',(-3.80507586227844,2.36286981549731,4.55160073480468));
#17983=CARTESIAN_POINT('Ctrl Pts',(-3.80515175559583,2.40004689761323,4.54959252805377));
#17984=CARTESIAN_POINT('Ctrl Pts',(-3.80534749188876,2.40017600730441,4.62540747194623));
#17985=CARTESIAN_POINT('Ctrl Pts',(-3.80551452420589,2.42064195120264,4.62429930431288));
#17986=CARTESIAN_POINT('Ctrl Pts',(-3.79329841012664,2.50933048388748,4.61948654032726));
#17987=CARTESIAN_POINT('Ctrl Pts',(-3.66590691767206,2.63375190534549,4.61096917998937));
#17988=CARTESIAN_POINT('Ctrl Pts',(-3.43935610442817,2.58214613327058,4.59985539093257));
#17989=CARTESIAN_POINT('Ctrl Pts',(-3.35984447062414,2.36381993973287,4.58874160187577));
#17990=CARTESIAN_POINT('Ctrl Pts',(-3.50014991641224,2.17860976567263,4.57762781281897));
#17991=CARTESIAN_POINT('Ctrl Pts',(-3.73179898227351,2.19603680019893,4.56651643617579));
#17992=CARTESIAN_POINT('Ctrl Pts',(-3.80581188677276,2.33203010689162,4.55910965588488));
#17993=CARTESIAN_POINT('Ctrl Pts',(-3.80581594649383,2.40000082771776,4.55540747194623));
#17994=CARTESIAN_POINT('Origin',(-3.6,2.4,5.35459252805377));
#17995=CARTESIAN_POINT('',(-3.80519403776112,2.3998960891277,4.69540747194623));
#17996=CARTESIAN_POINT('',(-3.80578859626649,2.40006787741036,4.68959252805377));
#17997=CARTESIAN_POINT('',(-3.805475,2.40000000000001,5.35459252805377));
#17998=CARTESIAN_POINT('Ctrl Pts',(-3.80578859626649,2.40006787741036,4.68959252805377));
#17999=CARTESIAN_POINT('Ctrl Pts',(-3.80580466836371,2.40380178606869,4.68938922436523));
#18000=CARTESIAN_POINT('Ctrl Pts',(-3.8040203778982,2.4755592442775,4.68548132432442));
#18001=CARTESIAN_POINT('Ctrl Pts',(-3.7203544535977,2.61094662622203,4.67786882793133));
#18002=CARTESIAN_POINT('Ctrl Pts',(-3.48804541599454,2.61552226041731,4.66675503887454));
#18003=CARTESIAN_POINT('Ctrl Pts',(-3.35820967878295,2.42282792546417,4.65564124981773));
#18004=CARTESIAN_POINT('Ctrl Pts',(-3.44968736466998,2.20923893144694,4.64452746076093));
#18005=CARTESIAN_POINT('Ctrl Pts',(-3.67874791033599,2.17025570685489,4.63341367170413));
#18006=CARTESIAN_POINT('Ctrl Pts',(-3.79614945128685,2.2983686897146,4.62510202746841));
#18007=CARTESIAN_POINT('Ctrl Pts',(-3.80560832232849,2.38316790767908,4.62049497958495));
#18008=CARTESIAN_POINT('Ctrl Pts',(-3.80545679372687,2.39981210841117,4.61959252805377));
#18009=CARTESIAN_POINT('Ctrl Pts',(-3.80519403776112,2.3998960891277,4.69540747194623));
#18010=CARTESIAN_POINT('Ctrl Pts',(-3.80500643965891,2.44086040425288,4.69319354909316));
#18011=CARTESIAN_POINT('Ctrl Pts',(-3.77326722861529,2.55063877508332,4.68727502988781));
#18012=CARTESIAN_POINT('Ctrl Pts',(-3.59442944478611,2.64280165560495,4.6776519143302));
#18013=CARTESIAN_POINT('Ctrl Pts',(-3.39298749751263,2.52700196401557,4.6665381252734));
#18014=CARTESIAN_POINT('Ctrl Pts',(-3.38102644144724,2.29495593446246,4.65542433621659));
#18015=CARTESIAN_POINT('Ctrl Pts',(-3.56949436685434,2.15905792937668,4.64431054715979));
#18016=CARTESIAN_POINT('Ctrl Pts',(-3.76430796130134,2.23525748954489,4.63430492573634));
#18017=CARTESIAN_POINT('Ctrl Pts',(-3.80495613638248,2.352224449347,4.62800390066515));
#18018=CARTESIAN_POINT('Ctrl Pts',(-3.80534749188876,2.40017600730441,4.62540747194623));
#18019=CARTESIAN_POINT('Origin',(-3.6,2.4,5.35459252805377));
#18020=CARTESIAN_POINT('',(-3.80572670757095,2.39987978133106,4.76540747194623));
#18021=CARTESIAN_POINT('',(-3.8052563985153,2.4001450986671,4.75959252805377));
#18022=CARTESIAN_POINT('',(-3.805475,2.40000000000001,5.35459252805377));
#18023=CARTESIAN_POINT('Ctrl Pts',(-3.8052563985153,2.4001450986671,4.75959252805377));
#18024=CARTESIAN_POINT('Ctrl Pts',(-3.80541421064946,2.4243482217442,4.7582834691455));
#18025=CARTESIAN_POINT('Ctrl Pts',(-3.79026314769432,2.51685423684082,4.75326981388497));
#18026=CARTESIAN_POINT('Ctrl Pts',(-3.65317165905879,2.6369735181158,4.74455156227217));
#18027=CARTESIAN_POINT('Ctrl Pts',(-3.42974255082951,2.57319374878213,4.73343777321536));
#18028=CARTESIAN_POINT('Ctrl Pts',(-3.36215201667677,2.35088777703746,4.72232398415856));
#18029=CARTESIAN_POINT('Ctrl Pts',(-3.51226643903938,2.1735347799409,4.71121019510176));
#18030=CARTESIAN_POINT('Ctrl Pts',(-3.73846936695489,2.20292040156477,4.70029970973349));
#18031=CARTESIAN_POINT('Ctrl Pts',(-3.80551180288158,2.33576256604952,4.6930938207175));
#18032=CARTESIAN_POINT('Ctrl Pts',(-3.80578859626649,2.40006787741036,4.68959252805377));
#18033=CARTESIAN_POINT('Ctrl Pts',(-3.80572670757095,2.39987978133106,4.76540747194623));
#18034=CARTESIAN_POINT('Ctrl Pts',(-3.80530256520545,2.46089806692785,4.76208779387343));
#18035=CARTESIAN_POINT('Ctrl Pts',(-3.74420122965308,2.59074745124221,4.75506351944836));
#18036=CARTESIAN_POINT('Ctrl Pts',(-3.52344221510783,2.63048336300545,4.74433464867103));
#18037=CARTESIAN_POINT('Ctrl Pts',(-3.36483726729874,2.46068083880743,4.73322085961422));
#18038=CARTESIAN_POINT('Ctrl Pts',(-3.42147943565789,2.23533645468145,4.72210707055742));
#18039=CARTESIAN_POINT('Ctrl Pts',(-3.64152350112028,2.16071048099716,4.71099328150062));
#18040=CARTESIAN_POINT('Ctrl Pts',(-3.7872979195691,2.27634402063526,4.70209341529689));
#18041=CARTESIAN_POINT('Ctrl Pts',(-3.80532035088855,2.37231408965339,4.69689814544543));
#18042=CARTESIAN_POINT('Ctrl Pts',(-3.80519403776112,2.3998960891277,4.69540747194623));
#18043=CARTESIAN_POINT('Origin',(-3.6,2.4,5.35459252805377));
#18044=CARTESIAN_POINT('',(-3.80555825533459,2.40017991403412,4.83540747194623));
#18045=CARTESIAN_POINT('',(-3.80526423105652,2.39985120339831,4.82959252805377));
#18046=CARTESIAN_POINT('',(-3.805475,2.40000000000001,5.35459252805377));
#18047=CARTESIAN_POINT('Ctrl Pts',(-3.80526423105652,2.39985120339831,4.82959252805377));
#18048=CARTESIAN_POINT('Ctrl Pts',(-3.80496496310342,2.44449429497159,4.82717771392578));
#18049=CARTESIAN_POINT('Ctrl Pts',(-3.76870077292898,2.55806758042747,4.82105830344552));
#18050=CARTESIAN_POINT('Ctrl Pts',(-3.58130943065524,2.64214527918755,4.81123429661299));
#18051=CARTESIAN_POINT('Ctrl Pts',(-3.38642339103422,2.51562311930547,4.80012050755619));
#18052=CARTESIAN_POINT('Ctrl Pts',(-3.38702644372307,2.28326980706774,4.78900671849939));
#18053=CARTESIAN_POINT('Ctrl Pts',(-3.58256660775658,2.15776096423133,4.77789292944257));
#18054=CARTESIAN_POINT('Ctrl Pts',(-3.76915215745557,2.24264335554317,4.76808819929404));
#18055=CARTESIAN_POINT('Ctrl Pts',(-3.80496760717513,2.35585412961529,4.76198806549777));
#18056=CARTESIAN_POINT('Ctrl Pts',(-3.8052563985153,2.4001450986671,4.75959252805377));
#18057=CARTESIAN_POINT('Ctrl Pts',(-3.80555825533459,2.40017991403412,4.83540747194623));
#18058=CARTESIAN_POINT('Ctrl Pts',(-3.80567994271202,2.41345772088563,4.83468663500598));
#18059=CARTESIAN_POINT('Ctrl Pts',(-3.79845785744155,2.49484232907173,4.83026120171345));
#18060=CARTESIAN_POINT('Ctrl Pts',(-3.68988494016744,2.62561997380774,4.82213117206865));
#18061=CARTESIAN_POINT('Ctrl Pts',(-3.45919254257122,2.59788111325323,4.81101738301186));
#18062=CARTESIAN_POINT('Ctrl Pts',(-3.35738280762477,2.38901942561361,4.79990359395505));
#18063=CARTESIAN_POINT('Ctrl Pts',(-3.47764334032546,2.19020838223802,4.78878980489825));
#18064=CARTESIAN_POINT('Ctrl Pts',(-3.70989831124516,2.18342198579874,4.77767601584144));
#18065=CARTESIAN_POINT('Ctrl Pts',(-3.8022342613798,2.31768599661427,4.76988190485744));
#18066=CARTESIAN_POINT('Ctrl Pts',(-3.80577588708354,2.39280468157954,4.7657923902257));
#18067=CARTESIAN_POINT('Ctrl Pts',(-3.80572670757095,2.39987978133106,4.76540747194623));
#18068=CARTESIAN_POINT('Origin',(-3.6,2.4,5.35459252805377));
#18069=CARTESIAN_POINT('',(-3.80514216591097,2.40000781019071,4.90540747194623));
#18070=CARTESIAN_POINT('',(-3.8057933217542,2.39993826202139,4.89959252805377));
#18071=CARTESIAN_POINT('',(-3.805475,2.40000000000001,5.35459252805377));
#18072=CARTESIAN_POINT('Ctrl Pts',(-3.8057933217542,2.39993826202139,4.89959252805377));
#18073=CARTESIAN_POINT('Ctrl Pts',(-3.80553738483576,2.46459365390411,4.89607195870605));
#18074=CARTESIAN_POINT('Ctrl Pts',(-3.73784442289473,2.59774586534896,4.88884679300607));
#18075=CARTESIAN_POINT('Ctrl Pts',(-3.51109208760397,2.62600676257303,4.87791703095382));
#18076=CARTESIAN_POINT('Ctrl Pts',(-3.36190028978558,2.44787694237367,4.86680324189701));
#18077=CARTESIAN_POINT('Ctrl Pts',(-3.43064385696086,2.2259248138587,4.85568945284022));
#18078=CARTESIAN_POINT('Ctrl Pts',(-3.65440102248913,2.16330567736551,4.8445756637834));
#18079=CARTESIAN_POINT('Ctrl Pts',(-3.7905654137645,2.28386779123864,4.83587668885459));
#18080=CARTESIAN_POINT('Ctrl Pts',(-3.80542407378798,2.37600677360117,4.83088231027805));
#18081=CARTESIAN_POINT('Ctrl Pts',(-3.80526423105652,2.39985120339831,4.82959252805377));
#18082=CARTESIAN_POINT('Ctrl Pts',(-3.80514216591096,2.40000781019071,4.90540747194623));
#18083=CARTESIAN_POINT('Ctrl Pts',(-3.80515363190124,2.43382668369574,4.90358087978625));
#18084=CARTESIAN_POINT('Ctrl Pts',(-3.78123591260341,2.53621991664107,4.898049691274));
#18085=CARTESIAN_POINT('Ctrl Pts',(-3.6197380796992,2.64206214751696,4.88881390640948));
#18086=CARTESIAN_POINT('Ctrl Pts',(-3.40733479453568,2.54786410535795,4.87770011735268));
#18087=CARTESIAN_POINT('Ctrl Pts',(-3.37128015690807,2.3183243706747,4.86658632829587));
#18088=CARTESIAN_POINT('Ctrl Pts',(-3.54457538552076,2.16354326577609,4.85547253923908));
#18089=CARTESIAN_POINT('Ctrl Pts',(-3.75407113442107,2.22119506367479,4.84507958712252));
#18090=CARTESIAN_POINT('Ctrl Pts',(-3.80505455493103,2.34521910535256,4.83839123135824));
#18091=CARTESIAN_POINT('Ctrl Pts',(-3.80555825533459,2.40017991403412,4.83540747194623));
#18092=CARTESIAN_POINT('Origin',(-3.6,2.4,5.35459252805377));
#18093=CARTESIAN_POINT('',(-3.80552958623817,2.39981603086253,4.97540747194623));
#18094=CARTESIAN_POINT('',(-3.8054461347863,2.4001877030526,4.96959252805377));
#18095=CARTESIAN_POINT('',(-3.805475,2.40000000000001,5.35459252805377));
#18096=CARTESIAN_POINT('Ctrl Pts',(-3.80544613478631,2.4001877030526,4.96959252805377));
#18097=CARTESIAN_POINT('Ctrl Pts',(-3.8056000456266,2.41718968004276,4.9686707998386));
#18098=CARTESIAN_POINT('Ctrl Pts',(-3.79589308272504,2.50235240455911,4.96404447527116));
#18099=CARTESIAN_POINT('Ctrl Pts',(-3.67755429503925,2.63014996180817,4.95571355435145));
#18100=CARTESIAN_POINT('Ctrl Pts',(-3.44869918906956,2.58997825726379,4.94459976529464));
#18101=CARTESIAN_POINT('Ctrl Pts',(-3.35833143120733,2.37591729928569,4.93348597623784));
#18102=CARTESIAN_POINT('Ctrl Pts',(-3.48916565507154,2.18389951041786,4.92237218718103));
#18103=CARTESIAN_POINT('Ctrl Pts',(-3.72144781179447,2.18968095039579,4.91125839812423));
#18104=CARTESIAN_POINT('Ctrl Pts',(-3.80419976151153,2.32515687187029,4.90366517841514));
#18105=CARTESIAN_POINT('Ctrl Pts',(-3.80580670007452,2.39655859898363,4.89977655505832));
#18106=CARTESIAN_POINT('Ctrl Pts',(-3.8057933217542,2.39993826202139,4.89959252805377));
#18107=CARTESIAN_POINT('Ctrl Pts',(-3.80552958623817,2.39981603086253,4.97540747194623));
#18108=CARTESIAN_POINT('Ctrl Pts',(-3.80503092645118,2.45384921596595,4.97247512456653));
#18109=CARTESIAN_POINT('Ctrl Pts',(-3.75549941221135,2.57695439031686,4.96583818083456));
#18110=CARTESIAN_POINT('Ctrl Pts',(-3.54785414659174,2.63720135974049,4.9554966407503));
#18111=CARTESIAN_POINT('Ctrl Pts',(-3.37243277255298,2.48483414437987,4.94438285169351));
#18112=CARTESIAN_POINT('Ctrl Pts',(-3.40530626273826,2.25481727477052,4.9332690626367));
#18113=CARTESIAN_POINT('Ctrl Pts',(-3.61638513853951,2.15768779995451,4.9221552735799));
#18114=CARTESIAN_POINT('Ctrl Pts',(-3.78023981554385,2.2618608319249,4.91286807668307));
#18115=CARTESIAN_POINT('Ctrl Pts',(-3.80513037719409,2.36523705642733,4.90728547613852));
#18116=CARTESIAN_POINT('Ctrl Pts',(-3.80514216591096,2.40000781019071,4.90540747194623));
#18117=CARTESIAN_POINT('Origin',(-3.6,2.4,5.35459252805377));
#18118=CARTESIAN_POINT('',(-3.8057470998819,2.40010656251728,5.04540747194623));
#18119=CARTESIAN_POINT('',(-3.80515433183015,2.39994744458997,5.03959252805377));
#18120=CARTESIAN_POINT('',(-3.805475,2.40000000000001,5.35459252805377));
#18121=CARTESIAN_POINT('Ctrl Pts',(-3.80515433183015,2.39994744458997,5.03959252805377));
#18122=CARTESIAN_POINT('Ctrl Pts',(-3.80506840880667,2.4374802122161,5.03756504461887));
#18123=CARTESIAN_POINT('Ctrl Pts',(-3.77723759754696,2.54371107308321,5.03183296483171));
#18124=CARTESIAN_POINT('Ctrl Pts',(-3.60662102779949,2.64277527582587,5.02239628869227));
#18125=CARTESIAN_POINT('Ctrl Pts',(-3.39962169493761,2.53723049491962,5.01128249963547));
#18126=CARTESIAN_POINT('Ctrl Pts',(-3.3760308968172,2.30607708183528,5.00016871057867));
#18127=CARTESIAN_POINT('Ctrl Pts',(-3.55744155898554,2.16089238284251,4.98905492152186));
#18128=CARTESIAN_POINT('Ctrl Pts',(-3.75953036163254,2.22845546798632,4.97886286068023));
#18129=CARTESIAN_POINT('Ctrl Pts',(-3.80498144946327,2.34885558664921,4.97237539619086));
#18130=CARTESIAN_POINT('Ctrl Pts',(-3.80544613478631,2.4001877030526,4.96959252805377));
#18131=CARTESIAN_POINT('Ctrl Pts',(-3.8057470998819,2.40010656251728,5.04540747194623));
#18132=CARTESIAN_POINT('Ctrl Pts',(-3.80578578291066,2.40623506936011,5.04507396569907));
#18133=CARTESIAN_POINT('Ctrl Pts',(-3.80275767503742,2.48040043607423,5.04103586309964));
#18134=CARTESIAN_POINT('Ctrl Pts',(-3.71288602216703,2.61503584063672,5.03329316414794));
#18135=CARTESIAN_POINT('Ctrl Pts',(-3.48055937550073,2.61146539619723,5.02217937509113));
#18136=CARTESIAN_POINT('Ctrl Pts',(-3.35755806712823,2.4143382523336,5.01106558603433));
#18137=CARTESIAN_POINT('Ctrl Pts',(-3.45646661930996,2.20408715554039,4.99995179697752));
#18138=CARTESIAN_POINT('Ctrl Pts',(-3.68675289766315,2.17315730107164,4.98883800792072));
#18139=CARTESIAN_POINT('Ctrl Pts',(-3.79782383296962,2.3032367743191,4.98065656624362));
#18140=CARTESIAN_POINT('Ctrl Pts',(-3.80566091089323,2.38558610982074,4.97617972091879));
#18141=CARTESIAN_POINT('Ctrl Pts',(-3.80552958623817,2.39981603086253,4.97540747194623));
#18142=CARTESIAN_POINT('Origin',(-3.6,2.4,5.35459252805377));
#18143=CARTESIAN_POINT('',(-3.80520911606596,2.40011619915578,5.11540747194623));
#18144=CARTESIAN_POINT('',(-3.80563879690963,2.399839625535,5.10959252805377));
#18145=CARTESIAN_POINT('',(-3.805475,2.40000000000001,5.35459252805377));
#18146=CARTESIAN_POINT('Ctrl Pts',(-3.80563879690963,2.399839625535,5.10959252805377));
#18147=CARTESIAN_POINT('Ctrl Pts',(-3.805144032728,2.45749534173516,5.10645928939914));
#18148=CARTESIAN_POINT('Ctrl Pts',(-3.74979515516761,2.58415303951777,5.09962145439226));
#18149=CARTESIAN_POINT('Ctrl Pts',(-3.53510505788101,2.63403473315196,5.0890790230331));
#18150=CARTESIAN_POINT('Ctrl Pts',(-3.36817873292179,2.47240567046266,5.07796523397629));
#18151=CARTESIAN_POINT('Ctrl Pts',(-3.41344102170209,2.24450262655374,5.06685144491949));
#18152=CARTESIAN_POINT('Ctrl Pts',(-3.6294628695539,2.15892821683407,5.05573765586269));
#18153=CARTESIAN_POINT('Ctrl Pts',(-3.78402795283848,2.2693666686934,5.04665135024078));
#18154=CARTESIAN_POINT('Ctrl Pts',(-3.80522540644911,2.36890073499569,5.04126964097114));
#18155=CARTESIAN_POINT('Ctrl Pts',(-3.80515433183015,2.39994744458997,5.03959252805377));
#18156=CARTESIAN_POINT('Ctrl Pts',(-3.80520911606596,2.40011619915578,5.11540747194623));
#18157=CARTESIAN_POINT('Ctrl Pts',(-3.80534689450199,2.42674223668704,5.11396821047934));
#18158=CARTESIAN_POINT('Ctrl Pts',(-3.7881600578547,2.52173200460476,5.10882435266019));
#18159=CARTESIAN_POINT('Ctrl Pts',(-3.64483147349944,2.63869087951471,5.09997589848877));
#18160=CARTESIAN_POINT('Ctrl Pts',(-3.42377646220466,2.56711959422357,5.08886210943196));
#18161=CARTESIAN_POINT('Ctrl Pts',(-3.36401957377094,2.34258029572384,5.07774832037515));
#18162=CARTESIAN_POINT('Ctrl Pts',(-3.52025888482579,2.17059867951396,5.06663453131835));
#18163=CARTESIAN_POINT('Ctrl Pts',(-3.7426071061349,2.20745024082863,5.05585424850871));
#18164=CARTESIAN_POINT('Ctrl Pts',(-3.80535609078813,2.33815945072363,5.04877856205134));
#18165=CARTESIAN_POINT('Ctrl Pts',(-3.8057470998819,2.40010656251728,5.04540747194623));
#18166=CARTESIAN_POINT('Origin',(-3.6,2.4,5.35459252805377));
#18167=CARTESIAN_POINT('',(-3.80526708520764,2.39977040928181,5.18540747194623));
#18168=CARTESIAN_POINT('',(-3.80565732826014,2.40014993187889,5.17959252805377));
#18169=CARTESIAN_POINT('',(-3.805475,2.40000000000001,5.35459252805377));
#18170=CARTESIAN_POINT('',(-3.65301702171886,2.20148256743283,5.2));
#18171=CARTESIAN_POINT('Ctrl Pts',(-3.65301702171886,2.20148256743283,5.2));
#18172=CARTESIAN_POINT('Ctrl Pts',(-3.71902879097456,2.21911198848201,5.19629540364773));
#18173=CARTESIAN_POINT('Ctrl Pts',(-3.79249439061758,2.28872811842027,5.19143122762981));
#18174=CARTESIAN_POINT('Ctrl Pts',(-3.80542873353734,2.378346888084,5.18656705161189));
#18175=CARTESIAN_POINT('Ctrl Pts',(-3.80526708520764,2.39977040928181,5.18540747194623));
#18176=CARTESIAN_POINT('',(-3.54686846753247,2.20112677390461,5.2));
#18177=CARTESIAN_POINT('Origin',(-3.6,2.4,5.2));
#18178=CARTESIAN_POINT('Ctrl Pts',(-3.54686839490754,2.2011265482535,5.2));
#18179=CARTESIAN_POINT('Ctrl Pts',(-3.61132828593009,2.18399467910883,5.19636770818144));
#18180=CARTESIAN_POINT('Ctrl Pts',(-3.74930829171963,2.21593295369214,5.1895652175327));
#18181=CARTESIAN_POINT('Ctrl Pts',(-3.80517196370246,2.34184094054235,5.18276272688396));
#18182=CARTESIAN_POINT('Ctrl Pts',(-3.80565732826014,2.40014993187889,5.17959252805377));
#18183=CARTESIAN_POINT('Origin',(0.,-2.4,2.2));
#18184=CARTESIAN_POINT('',(7.34788079488412E-17,-2.8,2.8));
#18185=CARTESIAN_POINT('Origin',(0.,-2.8,2.2));
#18186=CARTESIAN_POINT('',(7.34788079488412E-17,-2.,2.8));
#18187=CARTESIAN_POINT('',(7.34788079488412E-17,-2.4,2.8));
#18188=CARTESIAN_POINT('Origin',(0.,-2.,2.2));
#18189=CARTESIAN_POINT('Origin',(-2.4,1.,0.4));
#18190=CARTESIAN_POINT('',(-2.,1.,0.4));
#18191=CARTESIAN_POINT('Origin',(-2.4,1.,0.4));
#18192=CARTESIAN_POINT('',(-2.15,1.,0.4));
#18193=CARTESIAN_POINT('Origin',(-2.4,1.,0.4));
#18194=CARTESIAN_POINT('Origin',(-2.4,1.,0.2));
#18195=CARTESIAN_POINT('',(-2.,1.,0.));
#18196=CARTESIAN_POINT('Origin',(-2.4,1.,0.));
#18197=CARTESIAN_POINT('',(-2.,1.,0.2));
#18198=CARTESIAN_POINT('Origin',(-2.4,1.,0.4));
#18199=CARTESIAN_POINT('',(-2.15,1.,0.8));
#18200=CARTESIAN_POINT('',(-2.15,1.,0.4));
#18201=CARTESIAN_POINT('Origin',(-2.4,1.,0.8));
#18202=CARTESIAN_POINT('Origin',(2.4,1.,0.4));
#18203=CARTESIAN_POINT('',(2.8,1.,0.4));
#18204=CARTESIAN_POINT('Origin',(2.4,1.,0.4));
#18205=CARTESIAN_POINT('',(2.65,1.,0.4));
#18206=CARTESIAN_POINT('Origin',(2.4,1.,0.4));
#18207=CARTESIAN_POINT('Origin',(2.4,1.,0.2));
#18208=CARTESIAN_POINT('',(2.8,1.,0.));
#18209=CARTESIAN_POINT('Origin',(2.4,1.,0.));
#18210=CARTESIAN_POINT('',(2.8,1.,0.2));
#18211=CARTESIAN_POINT('Origin',(2.4,1.,0.4));
#18212=CARTESIAN_POINT('',(2.65,1.,0.8));
#18213=CARTESIAN_POINT('',(2.65,1.,0.4));
#18214=CARTESIAN_POINT('Origin',(2.4,1.,0.8));
#18215=CARTESIAN_POINT('Origin',(-3.6,2.4,4.3));
#18216=CARTESIAN_POINT('Ctrl Pts',(-3.76351293272515,2.3680769545372,4.3));
#18217=CARTESIAN_POINT('Ctrl Pts',(-3.76286871316717,2.35978063266222,4.3));
#18218=CARTESIAN_POINT('Ctrl Pts',(-3.76155560899202,2.35157023575845,4.3));
#18219=CARTESIAN_POINT('Ctrl Pts',(-3.75963220387653,2.34349709858594,4.3));
#18220=CARTESIAN_POINT('Ctrl Pts',(-3.75857027766629,2.33903985975814,4.3));
#18221=CARTESIAN_POINT('Ctrl Pts',(-3.75732203034493,2.33462439532847,4.3));
#18222=CARTESIAN_POINT('Ctrl Pts',(-3.75589532649161,2.33025917511629,4.3));
#18223=CARTESIAN_POINT('Ctrl Pts',(-3.75435560971578,2.32554817445892,4.3));
#18224=CARTESIAN_POINT('Ctrl Pts',(-3.75261043848503,2.32090359735875,4.3));
#18225=CARTESIAN_POINT('Ctrl Pts',(-3.75067344213558,2.31634215529567,4.3));
#18226=CARTESIAN_POINT('Ctrl Pts',(-3.74745267041618,2.30875754441053,4.3));
#18227=CARTESIAN_POINT('Ctrl Pts',(-3.74370039609997,2.30139711771457,4.3));
#18228=CARTESIAN_POINT('Ctrl Pts',(-3.73945961576596,2.29430909563144,4.3));
#18229=CARTESIAN_POINT('Ctrl Pts',(-3.73760645031824,2.29121172284092,4.3));
#18230=CARTESIAN_POINT('Ctrl Pts',(-3.73566013813008,2.28816728583911,4.3));
#18231=CARTESIAN_POINT('Ctrl Pts',(-3.73363014813367,2.28518827452246,4.3));
#18232=CARTESIAN_POINT('Ctrl Pts',(-3.72675415090804,2.27509774521709,4.3));
#18233=CARTESIAN_POINT('Ctrl Pts',(-3.71890632139719,2.26572975853371,4.3));
#18234=CARTESIAN_POINT('Ctrl Pts',(-3.71022045861654,2.25723279915054,4.3));
#18235=CARTESIAN_POINT('Ctrl Pts',(-3.7059906475113,2.25309497956169,4.3));
#18236=CARTESIAN_POINT('Ctrl Pts',(-3.70156132140551,2.2491639079058,4.3));
#18237=CARTESIAN_POINT('Ctrl Pts',(-3.6969439956845,2.24545878490313,4.3));
#18238=CARTESIAN_POINT('Ctrl Pts',(-3.69303802929494,2.24232448448942,4.3));
#18239=CARTESIAN_POINT('Ctrl Pts',(-3.68899297342194,2.23934940616711,4.3));
#18240=CARTESIAN_POINT('Ctrl Pts',(-3.68484121061819,2.23656266363051,4.3));
#18241=CARTESIAN_POINT('Ctrl Pts',(-3.67976592507208,2.23315603498015,4.3));
#18242=CARTESIAN_POINT('Ctrl Pts',(-3.6745257104219,2.23002554470273,4.3));
#18243=CARTESIAN_POINT('Ctrl Pts',(-3.66913582629221,2.22718930926681,4.3));
#18244=CARTESIAN_POINT('Ctrl Pts',(-3.6615627323528,2.22320423706977,4.3));
#18245=CARTESIAN_POINT('Ctrl Pts',(-3.65369447955584,2.21979946771843,4.3));
#18246=CARTESIAN_POINT('Ctrl Pts',(-3.64559786041243,2.21695927257373,4.3));
#18247=CARTESIAN_POINT('Ctrl Pts',(-3.6396877011334,2.21488606085518,4.3));
#18248=CARTESIAN_POINT('Ctrl Pts',(-3.63365563048822,2.21311388420288,4.3));
#18249=CARTESIAN_POINT('Ctrl Pts',(-3.62752539225901,2.21164027047228,4.3));
#18250=CARTESIAN_POINT('Ctrl Pts',(-3.62399744472375,2.21079220686783,4.3));
#18251=CARTESIAN_POINT('Ctrl Pts',(-3.62044147481098,2.2100443281221,4.3));
#18252=CARTESIAN_POINT('Ctrl Pts',(-3.61687028704666,2.20939689951074,4.3));
#18253=CARTESIAN_POINT('Ctrl Pts',(-3.605353381675,2.20730897399576,4.3));
#18254=CARTESIAN_POINT('Ctrl Pts',(-3.59365536798806,2.20625732317521,4.3));
#18255=CARTESIAN_POINT('Ctrl Pts',(-3.58193303067035,2.20620865478203,4.3));
#18256=CARTESIAN_POINT('Ctrl Pts',(-3.57526869322992,2.20618098601718,4.3));
#18257=CARTESIAN_POINT('Ctrl Pts',(-3.56859610554753,2.20647808326505,4.3));
#18258=CARTESIAN_POINT('Ctrl Pts',(-3.5619424077193,2.20709864598645,4.3));
#18259=CARTESIAN_POINT('Ctrl Pts',(-3.55784552037318,2.20748074562885,4.3));
#18260=CARTESIAN_POINT('Ctrl Pts',(-3.55375372321261,2.20798587206127,4.3));
#18261=CARTESIAN_POINT('Ctrl Pts',(-3.54967985340644,2.20861337807665,4.3));
#18262=CARTESIAN_POINT('Ctrl Pts',(-3.53642392777045,2.21065521384261,4.3));
#18263=CARTESIAN_POINT('Ctrl Pts',(-3.52344437883893,2.21397442298982,4.3));
#18264=CARTESIAN_POINT('Ctrl Pts',(-3.51095539964347,2.2185383760968,4.3));
#18265=CARTESIAN_POINT('Ctrl Pts',(-3.50062245090115,2.22231443279277,4.3));
#18266=CARTESIAN_POINT('Ctrl Pts',(-3.49062431451358,2.22694342333832,4.3));
#18267=CARTESIAN_POINT('Ctrl Pts',(-3.48108410337466,2.23243384161104,4.3));
#18268=CARTESIAN_POINT('Ctrl Pts',(-3.47992982403391,2.23309813260964,4.3));
#18269=CARTESIAN_POINT('Ctrl Pts',(-3.47878225959784,2.23377506397182,4.3));
#18270=CARTESIAN_POINT('Ctrl Pts',(-3.47764149019701,2.2344644673347,4.3));
#18271=CARTESIAN_POINT('Ctrl Pts',(-3.41173724903364,2.31767678198965,4.3));
#18272=CARTESIAN_POINT('Ctrl Pts',(-3.40908132667977,2.32572936887695,4.3));
#18273=CARTESIAN_POINT('Ctrl Pts',(-3.40697195743913,2.3339396046188,4.3));
#18274=CARTESIAN_POINT('Ctrl Pts',(-3.40539675516275,2.34225613248928,4.3));
#18275=CARTESIAN_POINT('Ctrl Pts',(-3.40421042715,2.34851953759571,4.3));
#18276=CARTESIAN_POINT('Ctrl Pts',(-3.40332726918042,2.35484328996956,4.3));
#18277=CARTESIAN_POINT('Ctrl Pts',(-3.40274510142185,2.36120518228067,4.3));
#18278=CARTESIAN_POINT('Ctrl Pts',(-3.40230911384944,2.36596962679656,4.3));
#18279=CARTESIAN_POINT('Ctrl Pts',(-3.40204239822336,2.37075409356134,4.3));
#18280=CARTESIAN_POINT('Ctrl Pts',(-3.40194406709946,2.37553699140669,4.3));
#18281=CARTESIAN_POINT('Ctrl Pts',(-3.40173837831389,2.38554184450123,4.3));
#18282=CARTESIAN_POINT('Ctrl Pts',(-3.40226689742789,2.39555478383888,4.3));
#18283=CARTESIAN_POINT('Ctrl Pts',(-3.40352192589958,2.40548747856692,4.3));
#18284=CARTESIAN_POINT('Ctrl Pts',(-3.40417748512669,2.41067578291694,4.3));
#18285=CARTESIAN_POINT('Ctrl Pts',(-3.40503255607762,2.41584510393915,4.3));
#18286=CARTESIAN_POINT('Ctrl Pts',(-3.40608151604784,2.42095776789691,4.3));
#18287=CARTESIAN_POINT('Ctrl Pts',(-3.40864845689543,2.4334691184973,4.3));
#18288=CARTESIAN_POINT('Ctrl Pts',(-3.41237570095201,2.44567367466126,4.3));
#18289=CARTESIAN_POINT('Ctrl Pts',(-3.41724958122609,2.45738288213971,4.3));
#18290=CARTESIAN_POINT('Ctrl Pts',(-3.41948715125122,2.46275851104282,4.3));
#18291=CARTESIAN_POINT('Ctrl Pts',(-3.42196701213329,2.46802938689262,4.3));
#18292=CARTESIAN_POINT('Ctrl Pts',(-3.4246907645117,2.47317480637784,4.3));
#18293=CARTESIAN_POINT('Ctrl Pts',(-3.42647139059006,2.47653857328711,4.3));
#18294=CARTESIAN_POINT('Ctrl Pts',(-3.42835735887431,2.47985042338477,4.3));
#18295=CARTESIAN_POINT('Ctrl Pts',(-3.43034607421528,2.48309853180527,4.3));
#18296=CARTESIAN_POINT('Ctrl Pts',(-3.4346184872232,2.49007653432835,4.3));
#18297=CARTESIAN_POINT('Ctrl Pts',(-3.43934735204432,2.49673388406761,4.3));
#18298=CARTESIAN_POINT('Ctrl Pts',(-3.44453054699271,2.50301823813816,4.3));
#18299=CARTESIAN_POINT('Ctrl Pts',(-3.45023589251222,2.50993567259632,4.3));
#18300=CARTESIAN_POINT('Ctrl Pts',(-3.45649190823175,2.51640147868906,4.3));
#18301=CARTESIAN_POINT('Ctrl Pts',(-3.46322632730094,2.52238265672963,4.3));
#18302=CARTESIAN_POINT('Ctrl Pts',(-3.46747028515846,2.52615193026038,4.3));
#18303=CARTESIAN_POINT('Ctrl Pts',(-3.47190440586361,2.52972849539073,4.3));
#18304=CARTESIAN_POINT('Ctrl Pts',(-3.4765114687556,2.53310132051434,4.3));
#18305=CARTESIAN_POINT('Ctrl Pts',(-3.47932494356125,2.53516106198772,4.3));
#18306=CARTESIAN_POINT('Ctrl Pts',(-3.48219950761294,2.53714209816472,4.3));
#18307=CARTESIAN_POINT('Ctrl Pts',(-3.48512412807744,2.53903826687632,4.3));
#18308=CARTESIAN_POINT('Ctrl Pts',(-3.49373597317477,2.5446217302422,4.3));
#18309=CARTESIAN_POINT('Ctrl Pts',(-3.50279826970664,2.54948377957132,4.3));
#18310=CARTESIAN_POINT('Ctrl Pts',(-3.51220207894208,2.55357333967367,4.3));
#18311=CARTESIAN_POINT('Ctrl Pts',(-3.5210279439966,2.5574115614721,4.3));
#18312=CARTESIAN_POINT('Ctrl Pts',(-3.53015530415702,2.56056927246177,4.3));
#18313=CARTESIAN_POINT('Ctrl Pts',(-3.53949459164804,2.56298239916129,4.3));
#18314=CARTESIAN_POINT('Ctrl Pts',(-3.54298202528158,2.5638834977967,4.3));
#18315=CARTESIAN_POINT('Ctrl Pts',(-3.54649047145145,2.5646782882288,4.3));
#18316=CARTESIAN_POINT('Ctrl Pts',(-3.55001192980026,2.5653638227639,4.3));
#18317=CARTESIAN_POINT('Ctrl Pts',(-3.56109314401874,2.567521041247,4.3));
#18318=CARTESIAN_POINT('Ctrl Pts',(-3.57231422450356,2.56860269457927,4.3));
#18319=CARTESIAN_POINT('Ctrl Pts',(-3.58352456323646,2.56851224856759,4.3));
#18320=CARTESIAN_POINT('Ctrl Pts',(-3.58970650036672,2.56846237214805,4.3));
#18321=CARTESIAN_POINT('Ctrl Pts',(-3.59588506606642,2.56805522595141,4.3));
#18322=CARTESIAN_POINT('Ctrl Pts',(-3.60203269728429,2.56726809931874,4.3));
#18323=CARTESIAN_POINT('Ctrl Pts',(-3.60310836212971,2.56713037400346,4.3));
#18324=CARTESIAN_POINT('Ctrl Pts',(-3.60418307356748,2.56698100334876,4.3));
#18325=CARTESIAN_POINT('Ctrl Pts',(-3.60525667864057,2.56682005840211,4.3));
#18326=CARTESIAN_POINT('Origin',(-3.6,2.4,5.35459252805377));
#18327=CARTESIAN_POINT('Ctrl Pts',(-3.80565732826014,2.40014993187889,5.17959252805377));
#18328=CARTESIAN_POINT('Ctrl Pts',(-3.80573914572043,2.40997902530624,5.17905813053169));
#18329=CARTESIAN_POINT('Ctrl Pts',(-3.80062938236564,2.48786313470717,5.17481913665734));
#18330=CARTESIAN_POINT('Ctrl Pts',(-3.70109553522054,2.62084298334156,5.16687554643073));
#18331=CARTESIAN_POINT('Ctrl Pts',(-3.46929950811782,2.60468896536386,5.15576175737392));
#18332=CARTESIAN_POINT('Ctrl Pts',(-3.35713783891219,2.401213058351,5.14464796831712));
#18333=CARTESIAN_POINT('Ctrl Pts',(-3.46726930372222,2.19661072251331,5.13353417926031));
#18334=CARTESIAN_POINT('Ctrl Pts',(-3.69889135748228,2.17818094124235,5.12242039020352));
#18335=CARTESIAN_POINT('Ctrl Pts',(-3.80021577778504,2.31073764355723,5.11443983980133));
#18336=CARTESIAN_POINT('Ctrl Pts',(-3.80572901899447,2.38932589169745,5.11016388575141));
#18337=CARTESIAN_POINT('Ctrl Pts',(-3.80563879690963,2.399839625535,5.10959252805377));
#18338=CARTESIAN_POINT('Ctrl Pts',(-3.80526708520764,2.39977040928181,5.18540747194623));
#18339=CARTESIAN_POINT('Ctrl Pts',(-3.80491230346332,2.4467902221928,5.18286245525962));
#18340=CARTESIAN_POINT('Ctrl Pts',(-3.76565540874154,2.56295294620881,5.17661284222074));
#18341=CARTESIAN_POINT('Ctrl Pts',(-3.57278676575927,2.64128531597693,5.16665863282959));
#18342=CARTESIAN_POINT('Ctrl Pts',(-3.38252462806861,2.5080933346037,5.15554484377278));
#18343=CARTESIAN_POINT('Ctrl Pts',(-3.39123766596766,2.27586209704876,5.14443105471597));
#18344=CARTESIAN_POINT('Ctrl Pts',(-3.59107442724388,2.15730569128375,5.13331726565918));
#18345=CARTESIAN_POINT('Ctrl Pts',(-3.77212564275939,2.247453977085,5.12364273806926));
#18346=CARTESIAN_POINT('Ctrl Pts',(-3.80499225880634,2.35820797534334,5.11767280683161));
#18347=CARTESIAN_POINT('Ctrl Pts',(-3.80520911606596,2.40011619915578,5.11540747194623));
#18348=CARTESIAN_POINT('Ctrl Pts',(-3.47309291201476,2.50793586530485,5.2));
#18349=CARTESIAN_POINT('Ctrl Pts',(-3.43720166889934,2.46573623930395,5.19629540364773));
#18350=CARTESIAN_POINT('Ctrl Pts',(-3.41147910372774,2.34341327692754,5.1888862109432));
#18351=CARTESIAN_POINT('Ctrl Pts',(-3.54548749138621,2.21065847912018,5.17777242188639));
#18352=CARTESIAN_POINT('Ctrl Pts',(-3.72942273074541,2.25164328799446,5.16665863282959));
#18353=CARTESIAN_POINT('Ctrl Pts',(-3.79487861203899,2.42820978532064,5.15554484377278));
#18354=CARTESIAN_POINT('Ctrl Pts',(-3.68196868800459,2.57906042596279,5.14443105471598));
#18355=CARTESIAN_POINT('Ctrl Pts',(-3.49402748778406,2.56596267978888,5.13331726565918));
#18356=CARTESIAN_POINT('Ctrl Pts',(-3.40308633148933,2.40098355284719,5.12220347660236));
#18357=CARTESIAN_POINT('Ctrl Pts',(-3.49238138946403,2.23509111264493,5.11108968754557));
#18358=CARTESIAN_POINT('Ctrl Pts',(-3.68018153136171,2.22014816795705,5.09997589848877));
#18359=CARTESIAN_POINT('Ctrl Pts',(-3.79459033398193,2.36982238810866,5.08886210943195));
#18360=CARTESIAN_POINT('Ctrl Pts',(-3.73088853410035,2.54712014517116,5.07774832037516));
#18361=CARTESIAN_POINT('Ctrl Pts',(-3.54738290615879,2.58975635256414,5.06663453131835));
#18362=CARTESIAN_POINT('Ctrl Pts',(-3.41203833510047,2.45870682418337,5.05552074226154));
#18363=CARTESIAN_POINT('Ctrl Pts',(-3.44873719048823,2.27392207121964,5.04440695320474));
#18364=CARTESIAN_POINT('Ctrl Pts',(-3.62388861938279,2.20453797748901,5.03329316414794));
#18365=CARTESIAN_POINT('Ctrl Pts',(-3.77717451978384,2.31406243911007,5.02217937509113));
#18366=CARTESIAN_POINT('Ctrl Pts',(-3.76829057505717,2.5022465500548,5.01106558603433));
#18367=CARTESIAN_POINT('Ctrl Pts',(-3.60536835737386,2.5968432215724,4.99995179697752));
#18368=CARTESIAN_POINT('Ctrl Pts',(-3.43753242183529,2.51126706632734,4.98883800792072));
#18369=CARTESIAN_POINT('Ctrl Pts',(-3.41840490283366,2.32384690027379,4.97772421886392));
#18370=CARTESIAN_POINT('Ctrl Pts',(-3.56549343582914,2.20613053160512,4.96661042980711));
#18371=CARTESIAN_POINT('Ctrl Pts',(-3.74416621827519,2.26586508520319,4.95549664075031));
#18372=CARTESIAN_POINT('Ctrl Pts',(-3.79088202621085,2.44837484789993,4.9443828516935));
#18373=CARTESIAN_POINT('Ctrl Pts',(-3.66288135078982,2.58660656351012,4.9332690626367));
#18374=CARTESIAN_POINT('Ctrl Pts',(-3.47732466187608,2.55403517537485,4.9221552735799));
#18375=CARTESIAN_POINT('Ctrl Pts',(-3.40405410117601,2.38047364429248,4.91104148452309));
#18376=CARTESIAN_POINT('Ctrl Pts',(-3.51013504384922,2.2247848080575,4.89992769546628));
#18377=CARTESIAN_POINT('Ctrl Pts',(-3.69847040002413,2.22947242407076,4.88881390640949));
#18378=CARTESIAN_POINT('Ctrl Pts',(-3.79667468232717,2.39024586425236,4.87770011735267));
#18379=CARTESIAN_POINT('Ctrl Pts',(-3.7148603974533,2.55994737550017,4.86658632829588));
#18380=CARTESIAN_POINT('Ctrl Pts',(-3.52791308818505,2.58324724002758,4.85547253923907));
#18381=CARTESIAN_POINT('Ctrl Pts',(-3.40694774682213,2.43881882759193,4.84435875018226));
#18382=CARTESIAN_POINT('Ctrl Pts',(-3.46268532215442,2.25885910202633,4.83324496112546));
#18383=CARTESIAN_POINT('Ctrl Pts',(-3.64410857937311,2.20808724102248,4.82213117206866));
#18384=CARTESIAN_POINT('Ctrl Pts',(-3.78515875366629,2.33297530474957,4.81101738301185));
#18385=CARTESIAN_POINT('Ctrl Pts',(-3.75673102088563,2.51921183215107,4.79990359395505));
#18386=CARTESIAN_POINT('Ctrl Pts',(-3.58484560723768,2.59633241763059,4.78878980489824));
#18387=CARTESIAN_POINT('Ctrl Pts',(-3.42683118114759,2.49374771469177,4.77767601584145));
#18388=CARTESIAN_POINT('Ctrl Pts',(-3.42732013882109,2.30535466532418,4.76656222678463));
#18389=CARTESIAN_POINT('Ctrl Pts',(-3.58586493175446,2.20359156413646,4.75544843772784));
#18390=CARTESIAN_POINT('Ctrl Pts',(-3.75734771295555,2.28160333171781,4.74433464867102));
#18391=CARTESIAN_POINT('Ctrl Pts',(-3.784808348044,2.46798491248738,4.73322085961423));
#18392=CARTESIAN_POINT('Ctrl Pts',(-3.64311180629855,2.59213913185591,4.72210707055742));
#18393=CARTESIAN_POINT('Ctrl Pts',(-3.46195453932691,2.54042622483077,4.71099328150062));
#18394=CARTESIAN_POINT('Ctrl Pts',(-3.40715184805135,2.36017960167632,4.69987949244381));
#18395=CARTESIAN_POINT('Ctrl Pts',(-3.52886525730118,2.21638104070156,4.688765703387));
#18396=CARTESIAN_POINT('Ctrl Pts',(-3.7156891032661,2.24065099555331,4.67765191433021));
#18397=CARTESIAN_POINT('Ctrl Pts',(-3.79662140100789,2.41077490131571,4.6665381252734));
#18398=CARTESIAN_POINT('Ctrl Pts',(-3.69758390056881,2.57103641770819,4.65542433621659));
#18399=CARTESIAN_POINT('Ctrl Pts',(-3.50922674926239,2.57474636128738,4.64431054715979));
#18400=CARTESIAN_POINT('Ctrl Pts',(-3.40395538379481,2.41850897862188,4.63319675810298));
#18401=CARTESIAN_POINT('Ctrl Pts',(-3.47812587883694,2.24533011791732,4.62208296904618));
#18402=CARTESIAN_POINT('Ctrl Pts',(-3.6638491391263,2.21372235435953,4.61096917998938));
#18403=CARTESIAN_POINT('Ctrl Pts',(-3.79113055827457,2.35261663238717,4.59985539093257));
#18404=CARTESIAN_POINT('Ctrl Pts',(-3.74346800986679,2.53488144415775,4.58874160187577));
#18405=CARTESIAN_POINT('Ctrl Pts',(-3.56448756498879,2.59368774042515,4.57762781281897));
#18406=CARTESIAN_POINT('Ctrl Pts',(-3.41801205461748,2.475209451325,4.56651402376216));
#18407=CARTESIAN_POINT('Ctrl Pts',(-3.4381121745334,2.28789109846994,4.55540023470536));
#18408=CARTESIAN_POINT('Ctrl Pts',(-3.60639005704185,2.20318729463469,4.54428644564855));
#18409=CARTESIAN_POINT('Ctrl Pts',(-3.76881904785141,2.29862839193225,4.53317265659175));
#18410=CARTESIAN_POINT('Ctrl Pts',(-3.77672604966501,2.48685607191854,4.52205886753494));
#18411=CARTESIAN_POINT('Ctrl Pts',(-3.62287369392911,2.59558340387831,4.51094507847814));
#18412=CARTESIAN_POINT('Ctrl Pts',(-3.44808478689753,2.52529102897173,4.49983128942133));
#18413=CARTESIAN_POINT('Ctrl Pts',(-3.41234559692803,2.34031835280842,4.48871750036453));
#18414=CARTESIAN_POINT('Ctrl Pts',(-3.54836861088932,2.20997296824294,4.47760371130773));
#18415=CARTESIAN_POINT('Ctrl Pts',(-3.73165041953522,2.2535614747159,4.46648992225092));
#18416=CARTESIAN_POINT('Ctrl Pts',(-3.79443110878254,2.431186836485,4.45537613319412));
#18417=CARTESIAN_POINT('Ctrl Pts',(-3.67924679391792,2.58026650835313,4.44426234413731));
#18418=CARTESIAN_POINT('Ctrl Pts',(-3.49152700036135,2.56434625038721,4.43314855508051));
#18419=CARTESIAN_POINT('Ctrl Pts',(-3.40309375251607,2.39799790627107,4.4220347660237));
#18420=CARTESIAN_POINT('Ctrl Pts',(-3.49489106815987,2.23348230018954,4.4109209769669));
#18421=CARTESIAN_POINT('Ctrl Pts',(-3.68289569684173,2.22138183485646,4.3998071879101));
#18422=CARTESIAN_POINT('Ctrl Pts',(-3.79502512287648,2.37277339930001,4.38869339885329));
#18423=CARTESIAN_POINT('Ctrl Pts',(-3.72864550427982,2.54908418322982,4.37757960979649));
#18424=CARTESIAN_POINT('Ctrl Pts',(-3.54451587329345,2.58893972093235,4.36646582073968));
#18425=CARTESIAN_POINT('Ctrl Pts',(-3.41117013795305,2.4558501873037,4.35535203168288));
#18426=CARTESIAN_POINT('Ctrl Pts',(-3.45066522941702,2.27165316239582,4.34423824262608));
#18427=CARTESIAN_POINT('Ctrl Pts',(-3.62684269841689,2.20490778718547,4.33312445356927));
#18428=CARTESIAN_POINT('Ctrl Pts',(-3.77846161969435,2.31678392154068,4.32201066451247));
#18429=CARTESIAN_POINT('Ctrl Pts',(-3.76671077264337,2.50472571563538,4.31089687545566));
#18430=CARTESIAN_POINT('Ctrl Pts',(-3.6024119571336,2.59701778495161,4.29978308639886));
#18431=CARTESIAN_POINT('Ctrl Pts',(-3.43581014038123,2.50855356077874,4.28866929734205));
#18432=CARTESIAN_POINT('Ctrl Pts',(-3.42516046182893,2.38400982617005,4.28126010463752));
#18433=CARTESIAN_POINT('Ctrl Pts',(-3.44735576439472,2.33325198627315,4.27755550828525));
#18434=CARTESIAN_POINT('Ctrl Pts',(-3.46322193753412,2.51633123698097,5.20748149723825));
#18435=CARTESIAN_POINT('Ctrl Pts',(-3.42453903360215,2.47084927712496,5.20377690088598));
#18436=CARTESIAN_POINT('Ctrl Pts',(-3.39681573869656,2.33901189865735,5.19636770818145));
#18437=CARTESIAN_POINT('Ctrl Pts',(-3.54124744782407,2.19593128499412,5.18525391912464));
#18438=CARTESIAN_POINT('Ctrl Pts',(-3.73948937471845,2.24010393789599,5.17414013006784));
#18439=CARTESIAN_POINT('Ctrl Pts',(-3.81003648727512,2.43040397380471,5.16302634101103));
#18440=CARTESIAN_POINT('Ctrl Pts',(-3.68834430374324,2.59298794508905,5.15191255195423));
#18441=CARTESIAN_POINT('Ctrl Pts',(-3.48578482789531,2.57887144164721,5.14079876289743));
#18442=CARTESIAN_POINT('Ctrl Pts',(-3.38777016729695,2.40106005468179,5.12968497384062));
#18443=CARTESIAN_POINT('Ctrl Pts',(-3.48401069421676,2.22226431593439,5.11857118478382));
#18444=CARTESIAN_POINT('Ctrl Pts',(-3.68641814006856,2.20615909238548,5.10745739572702));
#18445=CARTESIAN_POINT('Ctrl Pts',(-3.80972578663008,2.36747513988482,5.0963436066702));
#18446=CARTESIAN_POINT('Ctrl Pts',(-3.74106918988897,2.55856331372564,5.0852298176134));
#18447=CARTESIAN_POINT('Ctrl Pts',(-3.5432902900662,2.60451581276008,5.0741160285566));
#18448=CARTESIAN_POINT('Ctrl Pts',(-3.39741846770758,2.46327310627647,5.06300223949979));
#18449=CARTESIAN_POINT('Ctrl Pts',(-3.43697180089285,2.26411558966434,5.05188845044299));
#18450=CARTESIAN_POINT('Ctrl Pts',(-3.62574670277316,2.18933472393736,5.04077466138618));
#18451=CARTESIAN_POINT('Ctrl Pts',(-3.79095535102953,2.30737812002324,5.02966087232938));
#18452=CARTESIAN_POINT('Ctrl Pts',(-3.78138040319912,2.51019940046172,5.01854708327258));
#18453=CARTESIAN_POINT('Ctrl Pts',(-3.60578591418241,2.61215390632356,5.00743329421578));
#18454=CARTESIAN_POINT('Ctrl Pts',(-3.42489551286939,2.51992154252476,4.99631950515897));
#18455=CARTESIAN_POINT('Ctrl Pts',(-3.40428023416151,2.31792362746096,4.98520571610217));
#18456=CARTESIAN_POINT('Ctrl Pts',(-3.56280947688127,2.19105114868425,4.97409192704536));
#18457=CARTESIAN_POINT('Ctrl Pts',(-3.75537962710962,2.25543192231258,4.96297813798856));
#18458=CARTESIAN_POINT('Ctrl Pts',(-3.80572904255528,2.45213749738394,4.95186434893175));
#18459=CARTESIAN_POINT('Ctrl Pts',(-3.6677723322063,2.60112102960948,4.94075055987495));
#18460=CARTESIAN_POINT('Ctrl Pts',(-3.46778283760724,2.56601620267116,4.92963677081815));
#18461=CARTESIAN_POINT('Ctrl Pts',(-3.38881321118645,2.37895486262355,4.91852298176134));
#18462=CARTESIAN_POINT('Ctrl Pts',(-3.50314524759,2.21115637551095,4.90740919270453));
#18463=CARTESIAN_POINT('Ctrl Pts',(-3.70612953728091,2.21620859951243,4.89629540364773));
#18464=CARTESIAN_POINT('Ctrl Pts',(-3.81197225790835,2.38948717672297,4.88518161459093));
#18465=CARTESIAN_POINT('Ctrl Pts',(-3.72379436694309,2.57238826029923,4.87406782553412));
#18466=CARTESIAN_POINT('Ctrl Pts',(-3.52230608799136,2.5975004142094,4.86295403647732));
#18467=CARTESIAN_POINT('Ctrl Pts',(-3.39193192780995,2.44183819918584,4.85184024742051));
#18468=CARTESIAN_POINT('Ctrl Pts',(-3.45200483375657,2.24788100597045,4.84072645836371));
#18469=CARTESIAN_POINT('Ctrl Pts',(-3.64753939374511,2.19316005313682,4.8296126693069));
#18470=CARTESIAN_POINT('Ctrl Pts',(-3.79956060750538,2.3277620493917,4.81849888025011));
#18471=CARTESIAN_POINT('Ctrl Pts',(-3.76892173404475,2.52848426107239,4.80738509119329));
#18472=CARTESIAN_POINT('Ctrl Pts',(-3.5836668817102,2.61160337148291,4.7962713021365));
#18473=CARTESIAN_POINT('Ctrl Pts',(-3.41336191777647,2.50103951622967,4.78515751307969));
#18474=CARTESIAN_POINT('Ctrl Pts',(-3.41388890712174,2.29799304590536,4.77404372402289));
#18475=CARTESIAN_POINT('Ctrl Pts',(-3.58476549042184,2.18831469750142,4.76292993496608));
#18476=CARTESIAN_POINT('Ctrl Pts',(-3.76958639310991,2.27239430714904,4.75181614590928));
#18477=CARTESIAN_POINT('Ctrl Pts',(-3.79918294694398,2.47327285461012,4.74070235685247));
#18478=CARTESIAN_POINT('Ctrl Pts',(-3.64646509055197,2.60708392727588,4.72958856779567));
#18479=CARTESIAN_POINT('Ctrl Pts',(-3.45121720982778,2.55134873281456,4.71847477873886));
#18480=CARTESIAN_POINT('Ctrl Pts',(-3.39215190425982,2.3570823267967,4.70736098968206));
#18481=CARTESIAN_POINT('Ctrl Pts',(-3.52333231788058,2.20209895378134,4.69624720062526));
#18482=CARTESIAN_POINT('Ctrl Pts',(-3.7246875304159,2.22825665272044,4.68513341156845));
#18483=CARTESIAN_POINT('Ctrl Pts',(-3.81191483230877,2.41161298512653,4.67401962251165));
#18484=CARTESIAN_POINT('Ctrl Pts',(-3.70517408491178,2.58433982054614,4.66290583345484));
#18485=CARTESIAN_POINT('Ctrl Pts',(-3.50216630483977,2.58833832766402,4.65179204439804));
#18486=CARTESIAN_POINT('Ctrl Pts',(-3.38870681545753,2.41994862756931,4.64067825534123));
#18487=CARTESIAN_POINT('Ctrl Pts',(-3.46864637411461,2.23329972242719,4.62956446628443));
#18488=CARTESIAN_POINT('Ctrl Pts',(-3.6688153961962,2.19923347185799,4.61845067722763));
#18489=CARTESIAN_POINT('Ctrl Pts',(-3.80599690571939,2.34893110134286,4.60733688817082));
#18490=CARTESIAN_POINT('Ctrl Pts',(-3.7546271112745,2.54537267293252,4.59622309911402));
#18491=CARTESIAN_POINT('Ctrl Pts',(-3.56172536828799,2.60875298834237,4.58510931005721));
#18492=CARTESIAN_POINT('Ctrl Pts',(-3.40385682977405,2.48105932611543,4.57399552100042));
#18493=CARTESIAN_POINT('Ctrl Pts',(-3.42552035937731,2.27917114339395,4.5628817319436));
#18494=CARTESIAN_POINT('Ctrl Pts',(-3.60688708278715,2.18787898346807,4.5517679428868));
#18495=CARTESIAN_POINT('Ctrl Pts',(-3.7819499811952,2.2907435954864,4.54065415383));
#18496=CARTESIAN_POINT('Ctrl Pts',(-3.79047199840596,2.49361183381496,4.52954036477319));
#18497=CARTESIAN_POINT('Ctrl Pts',(-3.62465283528865,2.61079609860775,4.51842657571639));
#18498=CARTESIAN_POINT('Ctrl Pts',(-3.43626865262511,2.53503630458453,4.50731278665958));
#18499=CARTESIAN_POINT('Ctrl Pts',(-3.39774962870189,2.33567624789731,4.49619899760278));
#18500=CARTESIAN_POINT('Ctrl Pts',(-3.54435266400721,2.19519245431826,4.48508520854598));
#18501=CARTESIAN_POINT('Ctrl Pts',(-3.74189033562052,2.24217132331451,4.47397141948917));
#18502=CARTESIAN_POINT('Ctrl Pts',(-3.80955417671754,2.43361258332043,4.46285763043237));
#18503=CARTESIAN_POINT('Ctrl Pts',(-3.68541069770656,2.59428783790942,4.45174384137556));
#18504=CARTESIAN_POINT('Ctrl Pts',(-3.48308984977921,2.57712928456848,4.44063005231877));
#18505=CARTESIAN_POINT('Ctrl Pts',(-3.38777816553941,2.39784218119362,4.42951626326195));
#18506=CARTESIAN_POINT('Ctrl Pts',(-3.48671557851344,2.22053036825651,4.41840247420515));
#18507=CARTESIAN_POINT('Ctrl Pts',(-3.68934341635898,2.20748871526871,4.40728868514834));
#18508=CARTESIAN_POINT('Ctrl Pts',(-3.81019439388853,2.37065568400947,4.39617489609154));
#18509=CARTESIAN_POINT('Ctrl Pts',(-3.73865169471375,2.56068011684939,4.38506110703474));
#18510=CARTESIAN_POINT('Ctrl Pts',(-3.54020025619518,2.60363566261151,4.37394731797793));
#18511=CARTESIAN_POINT('Ctrl Pts',(-3.3964827412202,2.46019427700244,4.36283352892113));
#18512=CARTESIAN_POINT('Ctrl Pts',(-3.43904980483436,2.26167020258818,4.35171973986432));
#18513=CARTESIAN_POINT('Ctrl Pts',(-3.62893055336078,2.18973329784341,4.34060595080752));
#18514=CARTESIAN_POINT('Ctrl Pts',(-3.79234256300291,2.3103112823848,4.32949216175072));
#18515=CARTESIAN_POINT('Ctrl Pts',(-3.77967772199614,2.5128713982991,4.31837837269391));
#18516=CARTESIAN_POINT('Ctrl Pts',(-3.60259956184262,2.61234204743659,4.30726458363711));
#18517=CARTESIAN_POINT('Ctrl Pts',(-3.42303927044789,2.51699697749597,4.2961507945803));
#18518=CARTESIAN_POINT('Ctrl Pts',(-3.41156124805062,2.38276609266137,4.28874160187577));
#18519=CARTESIAN_POINT('Ctrl Pts',(-3.43548292594103,2.32806025151199,4.2850370055235));
#18520=CARTESIAN_POINT('Ctrl Pts',(-3.45335096305347,2.52472660865709,5.2149629944765));
#18521=CARTESIAN_POINT('Ctrl Pts',(-3.41187639830495,2.47596231494597,5.21125839812423));
#18522=CARTESIAN_POINT('Ctrl Pts',(-3.38215237366538,2.33461052038716,5.20384920541969));
#18523=CARTESIAN_POINT('Ctrl Pts',(-3.53700740426192,2.18120409086806,5.19273541636289));
#18524=CARTESIAN_POINT('Ctrl Pts',(-3.7495560186915,2.22856458779753,5.18162162730609));
#18525=CARTESIAN_POINT('Ctrl Pts',(-3.82519436251124,2.43259816228878,5.17050783824928));
#18526=CARTESIAN_POINT('Ctrl Pts',(-3.69471991948189,2.60691546421531,5.15939404919248));
#18527=CARTESIAN_POINT('Ctrl Pts',(-3.47754216800657,2.59178020350553,5.14828026013568));
#18528=CARTESIAN_POINT('Ctrl Pts',(-3.37245400310457,2.4011365565164,5.13716647107886));
#18529=CARTESIAN_POINT('Ctrl Pts',(-3.47563999896949,2.20943751922385,5.12605268202207));
#18530=CARTESIAN_POINT('Ctrl Pts',(-3.69265474877542,2.19217001681392,5.11493889296526));
#18531=CARTESIAN_POINT('Ctrl Pts',(-3.82486123927823,2.36512789166097,5.10382510390846));
#18532=CARTESIAN_POINT('Ctrl Pts',(-3.75124984567759,2.57000648228012,5.09271131485165));
#18533=CARTESIAN_POINT('Ctrl Pts',(-3.53919767397361,2.61927527295602,5.08159752579485));
#18534=CARTESIAN_POINT('Ctrl Pts',(-3.38279860031468,2.46783938836956,5.07048373673804));
#18535=CARTESIAN_POINT('Ctrl Pts',(-3.42520641129747,2.25430910810904,5.05936994768124));
#18536=CARTESIAN_POINT('Ctrl Pts',(-3.62760478616353,2.17413147038572,5.04825615862444));
#18537=CARTESIAN_POINT('Ctrl Pts',(-3.80473618227523,2.30069380093641,5.03714236956763));
#18538=CARTESIAN_POINT('Ctrl Pts',(-3.79447023134107,2.51815225086865,5.02602858051083));
#18539=CARTESIAN_POINT('Ctrl Pts',(-3.60620347099095,2.62746459107471,5.01491479145402));
#18540=CARTESIAN_POINT('Ctrl Pts',(-3.4122586039035,2.52857601872219,5.00380100239722));
#18541=CARTESIAN_POINT('Ctrl Pts',(-3.39015556548935,2.31200035464812,4.99268721334042));
#18542=CARTESIAN_POINT('Ctrl Pts',(-3.56012551793341,2.17597176576338,4.98157342428361));
#18543=CARTESIAN_POINT('Ctrl Pts',(-3.76659303594405,2.24499875942197,4.9704596352268));
#18544=CARTESIAN_POINT('Ctrl Pts',(-3.82057605889971,2.45590014686796,4.95934584617));
#18545=CARTESIAN_POINT('Ctrl Pts',(-3.67266331362277,2.61563549570883,4.94823205711319));
#18546=CARTESIAN_POINT('Ctrl Pts',(-3.4582410133384,2.57799722996748,4.93711826805639));
#18547=CARTESIAN_POINT('Ctrl Pts',(-3.37357232119689,2.37743608095462,4.92600447899959));
#18548=CARTESIAN_POINT('Ctrl Pts',(-3.49615545133077,2.19752794296441,4.91489068994278));
#18549=CARTESIAN_POINT('Ctrl Pts',(-3.71378867453769,2.20294477495411,4.90377690088598));
#18550=CARTESIAN_POINT('Ctrl Pts',(-3.82726983348952,2.38872848919359,4.89266311182918));
#18551=CARTESIAN_POINT('Ctrl Pts',(-3.73272833643288,2.58482914509829,4.88154932277237));
#18552=CARTESIAN_POINT('Ctrl Pts',(-3.51669908779767,2.61175358839122,4.87043553371557));
#18553=CARTESIAN_POINT('Ctrl Pts',(-3.37691610879776,2.44485757077975,4.85932174465876));
#18554=CARTESIAN_POINT('Ctrl Pts',(-3.44132434535872,2.23690290991458,4.84820795560196));
#18555=CARTESIAN_POINT('Ctrl Pts',(-3.65097020811712,2.17823286525116,4.83709416654515));
#18556=CARTESIAN_POINT('Ctrl Pts',(-3.81396246134447,2.32254879403384,4.82598037748835));
#18557=CARTESIAN_POINT('Ctrl Pts',(-3.78111244720387,2.5377566899937,4.81486658843155));
#18558=CARTESIAN_POINT('Ctrl Pts',(-3.58248815618272,2.62687432533523,4.80375279937474));
#18559=CARTESIAN_POINT('Ctrl Pts',(-3.39989265440535,2.50833131776757,4.79263901031794));
#18560=CARTESIAN_POINT('Ctrl Pts',(-3.4004576754224,2.29063142648655,4.78152522126113));
#18561=CARTESIAN_POINT('Ctrl Pts',(-3.58366604908921,2.17303783086637,4.77041143220433));
#18562=CARTESIAN_POINT('Ctrl Pts',(-3.78182507326426,2.26318528258027,4.75929764314753));
#18563=CARTESIAN_POINT('Ctrl Pts',(-3.81355754584396,2.47856079673287,4.74818385409072));
#18564=CARTESIAN_POINT('Ctrl Pts',(-3.64981837480538,2.62202872269584,4.73707006503392));
#18565=CARTESIAN_POINT('Ctrl Pts',(-3.44047988032865,2.56227124079834,4.72595627597711));
#18566=CARTESIAN_POINT('Ctrl Pts',(-3.3771519604683,2.35398505191708,4.71484248692031));
#18567=CARTESIAN_POINT('Ctrl Pts',(-3.51779937845998,2.18781686686112,4.7037286978635));
#18568=CARTESIAN_POINT('Ctrl Pts',(-3.73368595756569,2.21586230988758,4.6926149088067));
#18569=CARTESIAN_POINT('Ctrl Pts',(-3.82720826360965,2.41245106893735,4.6815011197499));
#18570=CARTESIAN_POINT('Ctrl Pts',(-3.71276426925474,2.59764322338409,4.67038733069309));
#18571=CARTESIAN_POINT('Ctrl Pts',(-3.49510586041716,2.60193029404067,4.65927354163629));
#18572=CARTESIAN_POINT('Ctrl Pts',(-3.37345824712023,2.42138827651674,4.64815975257948));
#18573=CARTESIAN_POINT('Ctrl Pts',(-3.4591668693923,2.22126932693707,4.63704596352268));
#18574=CARTESIAN_POINT('Ctrl Pts',(-3.67378165326609,2.18474458935644,4.62593217446588));
#18575=CARTESIAN_POINT('Ctrl Pts',(-3.82086325316422,2.34524557029854,4.61481838540907));
#18576=CARTESIAN_POINT('Ctrl Pts',(-3.7657862126822,2.55586390170729,4.60370459635227));
#18577=CARTESIAN_POINT('Ctrl Pts',(-3.55896317158719,2.6238182362596,4.59259080729546));
#18578=CARTESIAN_POINT('Ctrl Pts',(-3.38970160493063,2.48690920090586,4.58147701823866));
#18579=CARTESIAN_POINT('Ctrl Pts',(-3.41292854422122,2.27045118831796,4.57036322918185));
#18580=CARTESIAN_POINT('Ctrl Pts',(-3.60738410853246,2.17257067230145,4.55924944012505));
#18581=CARTESIAN_POINT('Ctrl Pts',(-3.79508091453898,2.28285879904056,4.54813565106825));
#18582=CARTESIAN_POINT('Ctrl Pts',(-3.80421794714692,2.50036759571139,4.53702186201144));
#18583=CARTESIAN_POINT('Ctrl Pts',(-3.62643197664818,2.62600879333718,4.52590807295464));
#18584=CARTESIAN_POINT('Ctrl Pts',(-3.42445251835268,2.54478158019733,4.51479428389783));
#18585=CARTESIAN_POINT('Ctrl Pts',(-3.38315366047576,2.3310341429862,4.50368049484103));
#18586=CARTESIAN_POINT('Ctrl Pts',(-3.54033671712511,2.18041194039358,4.49256670578422));
#18587=CARTESIAN_POINT('Ctrl Pts',(-3.75213025170582,2.23078117191311,4.48145291672742));
#18588=CARTESIAN_POINT('Ctrl Pts',(-3.82467724465257,2.43603833015588,4.47033912767062));
#18589=CARTESIAN_POINT('Ctrl Pts',(-3.69157460149519,2.60830916746569,4.45922533861381));
#18590=CARTESIAN_POINT('Ctrl Pts',(-3.47465269919707,2.58991231874976,4.44811154955701));
#18591=CARTESIAN_POINT('Ctrl Pts',(-3.37246257856274,2.39768645611616,4.4369977605002));
#18592=CARTESIAN_POINT('Ctrl Pts',(-3.47854008886701,2.20757843632347,4.4258839714434));
#18593=CARTESIAN_POINT('Ctrl Pts',(-3.69579113587624,2.19359559568096,4.41477018238659));
#18594=CARTESIAN_POINT('Ctrl Pts',(-3.82536366490058,2.36853796871893,4.4036563933298));
#18595=CARTESIAN_POINT('Ctrl Pts',(-3.74865788514769,2.57227605046896,4.39254260427298));
#18596=CARTESIAN_POINT('Ctrl Pts',(-3.5358846390969,2.61833160429067,4.38142881521619));
#18597=CARTESIAN_POINT('Ctrl Pts',(-3.38179534448736,2.46453836670119,4.37031502615938));
#18598=CARTESIAN_POINT('Ctrl Pts',(-3.4274343802517,2.25168724278053,4.35920123710257));
#18599=CARTESIAN_POINT('Ctrl Pts',(-3.63101840830467,2.17455880850134,4.34808744804577));
#18600=CARTESIAN_POINT('Ctrl Pts',(-3.80622350631146,2.30383864322893,4.33697365898897));
#18601=CARTESIAN_POINT('Ctrl Pts',(-3.79264467134891,2.52101708096281,4.32585986993216));
#18602=CARTESIAN_POINT('Ctrl Pts',(-3.60278716655164,2.62766630992157,4.31474608087536));
#18603=CARTESIAN_POINT('Ctrl Pts',(-3.41026840051456,2.5254403942132,4.30363229181855));
#18604=CARTESIAN_POINT('Ctrl Pts',(-3.3979620342723,2.38152235915268,4.29622309911402));
#18605=CARTESIAN_POINT('Ctrl Pts',(-3.42361008748734,2.32286851675082,4.29251850276175));
#18606=CARTESIAN_POINT('Ctrl Pts',(-3.44347998857283,2.53312198033322,5.22244449171475));
#18607=CARTESIAN_POINT('Ctrl Pts',(-3.39921376300775,2.48107535276698,5.21873989536248));
#18608=CARTESIAN_POINT('Ctrl Pts',(-3.36748900863419,2.33020914211697,5.21133070265795));
#18609=CARTESIAN_POINT('Ctrl Pts',(-3.53276736069978,2.16647689674201,5.20021691360114));
#18610=CARTESIAN_POINT('Ctrl Pts',(-3.75962266266454,2.21702523769905,5.18910312454434));
#18611=CARTESIAN_POINT('Ctrl Pts',(-3.84035223774737,2.43479235077285,5.17798933548753));
#18612=CARTESIAN_POINT('Ctrl Pts',(-3.70109553522054,2.62084298334156,5.16687554643073));
#18613=CARTESIAN_POINT('Ctrl Pts',(-3.46929950811782,2.60468896536386,5.15576175737392));
#18614=CARTESIAN_POINT('Ctrl Pts',(-3.35713783891219,2.401213058351,5.14464796831712));
#18615=CARTESIAN_POINT('Ctrl Pts',(-3.46726930372222,2.19661072251331,5.13353417926031));
#18616=CARTESIAN_POINT('Ctrl Pts',(-3.69889135748228,2.17818094124235,5.12242039020352));
#18617=CARTESIAN_POINT('Ctrl Pts',(-3.83999669192638,2.36278064343714,5.1113066011467));
#18618=CARTESIAN_POINT('Ctrl Pts',(-3.76143050146621,2.5814496508346,5.1001928120899));
#18619=CARTESIAN_POINT('Ctrl Pts',(-3.53510505788101,2.63403473315196,5.0890790230331));
#18620=CARTESIAN_POINT('Ctrl Pts',(-3.36817873292179,2.47240567046266,5.07796523397629));
#18621=CARTESIAN_POINT('Ctrl Pts',(-3.41344102170209,2.24450262655374,5.06685144491949));
#18622=CARTESIAN_POINT('Ctrl Pts',(-3.6294628695539,2.15892821683407,5.05573765586269));
#18623=CARTESIAN_POINT('Ctrl Pts',(-3.81851701352091,2.29400948184958,5.04462386680588));
#18624=CARTESIAN_POINT('Ctrl Pts',(-3.80756005948302,2.52610510127557,5.03351007774908));
#18625=CARTESIAN_POINT('Ctrl Pts',(-3.60662102779949,2.64277527582587,5.02239628869227));
#18626=CARTESIAN_POINT('Ctrl Pts',(-3.39962169493761,2.53723049491962,5.01128249963547));
#18627=CARTESIAN_POINT('Ctrl Pts',(-3.3760308968172,2.30607708183528,5.00016871057867));
#18628=CARTESIAN_POINT('Ctrl Pts',(-3.55744155898554,2.16089238284251,4.98905492152186));
#18629=CARTESIAN_POINT('Ctrl Pts',(-3.77780644477848,2.23456559653136,4.97794113246506));
#18630=CARTESIAN_POINT('Ctrl Pts',(-3.83542307524414,2.45966279635197,4.96682734340825));
#18631=CARTESIAN_POINT('Ctrl Pts',(-3.67755429503925,2.63014996180817,4.95571355435145));
#18632=CARTESIAN_POINT('Ctrl Pts',(-3.44869918906956,2.58997825726379,4.94459976529464));
#18633=CARTESIAN_POINT('Ctrl Pts',(-3.35833143120733,2.37591729928569,4.93348597623784));
#18634=CARTESIAN_POINT('Ctrl Pts',(-3.48916565507154,2.18389951041786,4.92237218718103));
#18635=CARTESIAN_POINT('Ctrl Pts',(-3.72144781179447,2.18968095039579,4.91125839812423));
#18636=CARTESIAN_POINT('Ctrl Pts',(-3.84256740907069,2.38796980166419,4.90014460906742));
#18637=CARTESIAN_POINT('Ctrl Pts',(-3.74166230592267,2.59727002989735,4.88903082001062));
#18638=CARTESIAN_POINT('Ctrl Pts',(-3.51109208760397,2.62600676257303,4.87791703095382));
#18639=CARTESIAN_POINT('Ctrl Pts',(-3.36190028978558,2.44787694237367,4.86680324189701));
#18640=CARTESIAN_POINT('Ctrl Pts',(-3.43064385696086,2.2259248138587,4.85568945284022));
#18641=CARTESIAN_POINT('Ctrl Pts',(-3.65440102248913,2.16330567736551,4.8445756637834));
#18642=CARTESIAN_POINT('Ctrl Pts',(-3.82836431518356,2.31733553867597,4.8334618747266));
#18643=CARTESIAN_POINT('Ctrl Pts',(-3.79330316036299,2.54702911891502,4.8223480856698));
#18644=CARTESIAN_POINT('Ctrl Pts',(-3.58130943065524,2.64214527918755,4.81123429661299));
#18645=CARTESIAN_POINT('Ctrl Pts',(-3.38642339103422,2.51562311930547,4.80012050755619));
#18646=CARTESIAN_POINT('Ctrl Pts',(-3.38702644372307,2.28326980706774,4.78900671849939));
#18647=CARTESIAN_POINT('Ctrl Pts',(-3.58256660775658,2.15776096423133,4.77789292944257));
#18648=CARTESIAN_POINT('Ctrl Pts',(-3.79406375341862,2.2539762580115,4.76677914038578));
#18649=CARTESIAN_POINT('Ctrl Pts',(-3.82793214474394,2.48384873885561,4.75566535132897));
#18650=CARTESIAN_POINT('Ctrl Pts',(-3.65317165905879,2.6369735181158,4.74455156227217));
#18651=CARTESIAN_POINT('Ctrl Pts',(-3.42974255082951,2.57319374878213,4.73343777321536));
#18652=CARTESIAN_POINT('Ctrl Pts',(-3.36215201667677,2.35088777703746,4.72232398415856));
#18653=CARTESIAN_POINT('Ctrl Pts',(-3.51226643903938,2.1735347799409,4.71121019510176));
#18654=CARTESIAN_POINT('Ctrl Pts',(-3.74268438471549,2.20346796705471,4.70009640604495));
#18655=CARTESIAN_POINT('Ctrl Pts',(-3.84250169491054,2.41328915274817,4.68898261698815));
#18656=CARTESIAN_POINT('Ctrl Pts',(-3.7203544535977,2.61094662622203,4.67786882793133));
#18657=CARTESIAN_POINT('Ctrl Pts',(-3.48804541599454,2.61552226041731,4.66675503887454));
#18658=CARTESIAN_POINT('Ctrl Pts',(-3.35820967878295,2.42282792546417,4.65564124981773));
#18659=CARTESIAN_POINT('Ctrl Pts',(-3.44968736466998,2.20923893144694,4.64452746076093));
#18660=CARTESIAN_POINT('Ctrl Pts',(-3.67874791033599,2.17025570685489,4.63341367170413));
#18661=CARTESIAN_POINT('Ctrl Pts',(-3.83572960060904,2.34156003925422,4.62229988264732));
#18662=CARTESIAN_POINT('Ctrl Pts',(-3.77694531408991,2.56635513048207,4.61118609359051));
#18663=CARTESIAN_POINT('Ctrl Pts',(-3.55620097488638,2.63888348417682,4.60007230453371));
#18664=CARTESIAN_POINT('Ctrl Pts',(-3.3755463800872,2.4927590756963,4.58895851547691));
#18665=CARTESIAN_POINT('Ctrl Pts',(-3.40033672906513,2.26173123324197,4.5778447264201));
#18666=CARTESIAN_POINT('Ctrl Pts',(-3.60788113427776,2.15726236113484,4.5667309373633));
#18667=CARTESIAN_POINT('Ctrl Pts',(-3.80821184788277,2.27497400259471,4.55561714830649));
#18668=CARTESIAN_POINT('Ctrl Pts',(-3.81796389588787,2.50712335760782,4.54450335924969));
#18669=CARTESIAN_POINT('Ctrl Pts',(-3.62821111800771,2.64122148806661,4.53338957019289));
#18670=CARTESIAN_POINT('Ctrl Pts',(-3.41263638408026,2.55452685581013,4.52227578113608));
#18671=CARTESIAN_POINT('Ctrl Pts',(-3.36855769224962,2.32639203807509,4.51116199207928));
#18672=CARTESIAN_POINT('Ctrl Pts',(-3.536320770243,2.1656314264689,4.50004820302247));
#18673=CARTESIAN_POINT('Ctrl Pts',(-3.76237016779111,2.21939102051171,4.48893441396567));
#18674=CARTESIAN_POINT('Ctrl Pts',(-3.83980031258758,2.43846407699132,4.47782062490887));
#18675=CARTESIAN_POINT('Ctrl Pts',(-3.69773850528383,2.62233049702197,4.46670683585206));
#18676=CARTESIAN_POINT('Ctrl Pts',(-3.46621554861493,2.60269535293104,4.45559304679526));
#18677=CARTESIAN_POINT('Ctrl Pts',(-3.35714699158608,2.39753073103871,4.44447925773845));
#18678=CARTESIAN_POINT('Ctrl Pts',(-3.47036459922058,2.19462650439043,4.43336546868165));
#18679=CARTESIAN_POINT('Ctrl Pts',(-3.70223885539349,2.17970247609322,4.42225167962484));
#18680=CARTESIAN_POINT('Ctrl Pts',(-3.84053293591263,2.36642025342839,4.41113789056805));
#18681=CARTESIAN_POINT('Ctrl Pts',(-3.75866407558161,2.58387198408852,4.40002410151123));
#18682=CARTESIAN_POINT('Ctrl Pts',(-3.53156902199863,2.63302754596983,4.38891031245443));
#18683=CARTESIAN_POINT('Ctrl Pts',(-3.36710794775451,2.46888245639993,4.37779652339763));
#18684=CARTESIAN_POINT('Ctrl Pts',(-3.41581895566904,2.24170428297288,4.36668273434082));
#18685=CARTESIAN_POINT('Ctrl Pts',(-3.63310626324856,2.15938431915927,4.35556894528402));
#18686=CARTESIAN_POINT('Ctrl Pts',(-3.82010444962002,2.29736600407305,4.34445515622722));
#18687=CARTESIAN_POINT('Ctrl Pts',(-3.80561162070166,2.52916276362653,4.33334136717041));
#18688=CARTESIAN_POINT('Ctrl Pts',(-3.60297477126067,2.64299057240655,4.32222757811361));
#18689=CARTESIAN_POINT('Ctrl Pts',(-3.39749753058122,2.53388381093044,4.3111137890568));
#18690=CARTESIAN_POINT('Ctrl Pts',(-3.38436282049399,2.380278625644,4.30370459635227));
#18691=CARTESIAN_POINT('Ctrl Pts',(-3.41173724903364,2.31767678198965,4.3));
#18692=CARTESIAN_POINT('Ctrl Pts',(-3.47309291201476,2.50793586530485,5.2));
#18693=CARTESIAN_POINT('Ctrl Pts',(-3.46488109712516,2.50027511355887,5.2));
#18694=CARTESIAN_POINT('Ctrl Pts',(-3.45756392397337,2.49177395403935,5.2));
#18695=CARTESIAN_POINT('Ctrl Pts',(-3.45114582175476,2.48262659215394,5.2));
#18696=CARTESIAN_POINT('Ctrl Pts',(-3.44637505636198,2.47582708724863,5.2));
#18697=CARTESIAN_POINT('Ctrl Pts',(-3.44210140258396,2.46866923691254,5.2));
#18698=CARTESIAN_POINT('Ctrl Pts',(-3.4383368615674,2.46121837901648,5.2));
#18699=CARTESIAN_POINT('Ctrl Pts',(-3.43611956164057,2.45682985287343,5.2));
#18700=CARTESIAN_POINT('Ctrl Pts',(-3.43407749071882,2.45233446363919,5.2));
#18701=CARTESIAN_POINT('Ctrl Pts',(-3.4322255599542,2.44777399682775,5.2));
#18702=CARTESIAN_POINT('Ctrl Pts',(-3.42766722424942,2.43654888026604,5.2));
#18703=CARTESIAN_POINT('Ctrl Pts',(-3.42424189960471,2.42490562017205,5.2));
#18704=CARTESIAN_POINT('Ctrl Pts',(-3.42197767565222,2.41304271238881,5.2));
#18705=CARTESIAN_POINT('Ctrl Pts',(-3.42053879301361,2.40550400048974,5.2));
#18706=CARTESIAN_POINT('Ctrl Pts',(-3.41956954249672,2.39787570455109,5.2));
#18707=CARTESIAN_POINT('Ctrl Pts',(-3.41908669765048,2.39020364672881,5.2));
#18708=CARTESIAN_POINT('Ctrl Pts',(-3.4188613702662,2.3866233564252,5.2));
#18709=CARTESIAN_POINT('Ctrl Pts',(-3.4187425132976,2.38303698501937,5.2));
#18710=CARTESIAN_POINT('Ctrl Pts',(-3.4187312729093,2.37945933257344,5.2));
#18711=CARTESIAN_POINT('Ctrl Pts',(-3.41869622423253,2.36830384747272,5.2));
#18712=CARTESIAN_POINT('Ctrl Pts',(-3.4197031160267,2.35720597826242,5.2));
#18713=CARTESIAN_POINT('Ctrl Pts',(-3.42178566785009,2.34630687436894,5.2));
#18714=CARTESIAN_POINT('Ctrl Pts',(-3.42294604955552,2.3402339783087,5.2));
#18715=CARTESIAN_POINT('Ctrl Pts',(-3.42444092603953,2.33422255306027,5.2));
#18716=CARTESIAN_POINT('Ctrl Pts',(-3.42625156753842,2.32828873958556,5.2));
#18717=CARTESIAN_POINT('Ctrl Pts',(-3.42738421175614,2.32457685099508,5.2));
#18718=CARTESIAN_POINT('Ctrl Pts',(-3.42864107094821,2.32089381471682,5.2));
#18719=CARTESIAN_POINT('Ctrl Pts',(-3.4300164442918,2.31724844575858,5.2));
#18720=CARTESIAN_POINT('Ctrl Pts',(-3.43439823178552,2.30563470307137,5.2));
#18721=CARTESIAN_POINT('Ctrl Pts',(-3.43994733372525,2.29448387749046,5.2));
#18722=CARTESIAN_POINT('Ctrl Pts',(-3.44649833143843,2.28391851131164,5.2));
#18723=CARTESIAN_POINT('Ctrl Pts',(-3.45083930540137,2.27691744345919,5.2));
#18724=CARTESIAN_POINT('Ctrl Pts',(-3.45562139981211,2.27017330264703,5.2));
#18725=CARTESIAN_POINT('Ctrl Pts',(-3.46080803162185,2.26372396193311,5.2));
#18726=CARTESIAN_POINT('Ctrl Pts',(-3.46351816065219,2.2603540397685,5.2));
#18727=CARTESIAN_POINT('Ctrl Pts',(-3.46634013864158,2.25706328802701,5.2));
#18728=CARTESIAN_POINT('Ctrl Pts',(-3.46926558695491,2.25386191331523,5.2));
#18729=CARTESIAN_POINT('Ctrl Pts',(-3.47553201369268,2.24700444124844,5.2));
#18730=CARTESIAN_POINT('Ctrl Pts',(-3.48224798017073,2.24058272300471,5.2));
#18731=CARTESIAN_POINT('Ctrl Pts',(-3.48935940275436,2.23464751188384,5.2));
#18732=CARTESIAN_POINT('Ctrl Pts',(-3.49388585721574,2.23086972163985,5.2));
#18733=CARTESIAN_POINT('Ctrl Pts',(-3.49857277644925,2.2272891074735,5.2));
#18734=CARTESIAN_POINT('Ctrl Pts',(-3.50340840926684,2.2239201748241,5.2));
#18735=CARTESIAN_POINT('Ctrl Pts',(-3.50748096973522,2.22108286635877,5.2));
#18736=CARTESIAN_POINT('Ctrl Pts',(-3.51165201299164,2.21840074277452,5.2));
#18737=CARTESIAN_POINT('Ctrl Pts',(-3.51591072169151,2.21588342574414,5.2));
#18738=CARTESIAN_POINT('Ctrl Pts',(-3.52463381704441,2.21072721571968,5.2));
#18739=CARTESIAN_POINT('Ctrl Pts',(-3.53372795060187,2.20625881994954,5.2));
#18740=CARTESIAN_POINT('Ctrl Pts',(-3.54313435341931,2.20255201733462,5.2));
#18741=CARTESIAN_POINT('Ctrl Pts',(-3.5443736619696,2.20206364018726,5.2));
#18742=CARTESIAN_POINT('Ctrl Pts',(-3.54561840623672,2.20158850319392,5.2));
#18743=CARTESIAN_POINT('Ctrl Pts',(-3.54686839490754,2.2011265482535,5.2));
#18744=CARTESIAN_POINT('Ctrl Pts',(-3.76673280722786,2.39986996770474,5.08714803633902));
#18745=CARTESIAN_POINT('Ctrl Pts',(-3.76680595967625,2.39134538779314,5.08771939403666));
#18746=CARTESIAN_POINT('Ctrl Pts',(-3.76620865205667,2.38283109327188,5.08829075173431));
#18747=CARTESIAN_POINT('Ctrl Pts',(-3.76490523356496,2.37442631092714,5.08886210943196));
#18748=CARTESIAN_POINT('Ctrl Pts',(-3.75645406644185,2.31993098139145,5.09256670578422));
#18749=CARTESIAN_POINT('Ctrl Pts',(-3.71831779890178,2.27003957467425,5.0962713021365));
#18750=CARTESIAN_POINT('Ctrl Pts',(-3.66794964148213,2.24758436209697,5.09997589848877));
#18751=CARTESIAN_POINT('Ctrl Pts',(-3.61758148406248,2.22512914951968,5.10368049484103));
#18752=CARTESIAN_POINT('Ctrl Pts',(-3.55498143676326,2.2301101310823,5.1073850911933));
#18753=CARTESIAN_POINT('Ctrl Pts',(-3.50879890345119,2.26024936189732,5.11108968754557));
#18754=CARTESIAN_POINT('Ctrl Pts',(-3.46261637013913,2.29038859271235,5.11479428389783));
#18755=CARTESIAN_POINT('Ctrl Pts',(-3.43285135081423,2.34568607277977,5.1184988802501));
#18756=CARTESIAN_POINT('Ctrl Pts',(-3.43312570053424,2.40083133397043,5.12220347660237));
#18757=CARTESIAN_POINT('Ctrl Pts',(-3.43340005025424,2.45597659516109,5.12590807295464));
#18758=CARTESIAN_POINT('Ctrl Pts',(-3.46371376901915,2.51096963747498,5.12961266930691));
#18759=CARTESIAN_POINT('Ctrl Pts',(-3.51019416177169,2.54064911632758,5.13331726565918));
#18760=CARTESIAN_POINT('Ctrl Pts',(-3.55667455452423,2.57032859518018,5.13702186201145));
#18761=CARTESIAN_POINT('Ctrl Pts',(-3.61932162126441,2.57469451057149,5.14072645836371));
#18762=CARTESIAN_POINT('Ctrl Pts',(-3.6694634753069,2.55173569482678,5.14443105471598));
#18763=CARTESIAN_POINT('Ctrl Pts',(-3.71960532934939,2.52877687908207,5.14813565106825));
#18764=CARTESIAN_POINT('Ctrl Pts',(-3.75724197069419,2.47849333220135,5.15184024742052));
#18765=CARTESIAN_POINT('Ctrl Pts',(-3.76515097781766,2.42392380920663,5.15554484377278));
#18766=CARTESIAN_POINT('Ctrl Pts',(-3.76629187237323,2.41605201560311,5.15607924129486));
#18767=CARTESIAN_POINT('Ctrl Pts',(-3.76681417046854,2.40809103597041,5.15661363881694));
#18768=CARTESIAN_POINT('Ctrl Pts',(-3.76674783252531,2.40012156540224,5.15714803633902));
#18769=CARTESIAN_POINT('Ctrl Pts',(-3.65301702171886,2.20148256743283,5.2));
#18770=CARTESIAN_POINT('Ctrl Pts',(-3.71902879097456,2.21911198848201,5.19629540364773));
#18771=CARTESIAN_POINT('Ctrl Pts',(-3.83093279751213,2.32515241961692,5.1888862109432));
#18772=CARTESIAN_POINT('Ctrl Pts',(-3.78812294461068,2.55382789975093,5.17777242188639));
#18773=CARTESIAN_POINT('Ctrl Pts',(-3.57278676575927,2.64128531597693,5.16665863282959));
#18774=CARTESIAN_POINT('Ctrl Pts',(-3.38252462806861,2.5080933346037,5.15554484377278));
#18775=CARTESIAN_POINT('Ctrl Pts',(-3.39123766596766,2.27586209704876,5.14443105471597));
#18776=CARTESIAN_POINT('Ctrl Pts',(-3.59107442724388,2.15730569128375,5.13331726565918));
#18777=CARTESIAN_POINT('Ctrl Pts',(-3.79906029518588,2.2608651698129,5.12220347660237));
#18778=CARTESIAN_POINT('Ctrl Pts',(-3.82485429121136,2.49178880612566,5.11108968754556));
#18779=CARTESIAN_POINT('Ctrl Pts',(-3.64483147349944,2.63869087951471,5.09997589848877));
#18780=CARTESIAN_POINT('Ctrl Pts',(-3.42377646220466,2.56711959422357,5.08886210943196));
#18781=CARTESIAN_POINT('Ctrl Pts',(-3.36401957377094,2.34258029572384,5.07774832037515));
#18782=CARTESIAN_POINT('Ctrl Pts',(-3.52025888482579,2.17059867951396,5.06663453131835));
#18783=CARTESIAN_POINT('Ctrl Pts',(-3.74948582371233,2.20859030608788,5.05552074226155));
#18784=CARTESIAN_POINT('Ctrl Pts',(-3.8418868522934,2.42178158973285,5.04440695320474));
#18785=CARTESIAN_POINT('Ctrl Pts',(-3.71288602216703,2.61503584063672,5.03329316414794));
#18786=CARTESIAN_POINT('Ctrl Pts',(-3.48055937550073,2.61146539619723,5.02217937509113));
#18787=CARTESIAN_POINT('Ctrl Pts',(-3.35755806712823,2.4143382523336,5.01106558603433));
#18788=CARTESIAN_POINT('Ctrl Pts',(-3.45646661930996,2.20408715554039,4.99995179697752));
#18789=CARTESIAN_POINT('Ctrl Pts',(-3.68675289766315,2.17315730107164,4.98883800792072));
#18790=CARTESIAN_POINT('Ctrl Pts',(-3.83763326741432,2.34985914450584,4.97772421886391));
#18791=CARTESIAN_POINT('Ctrl Pts',(-3.77100521132112,2.57245548011022,4.96661042980712));
#18792=CARTESIAN_POINT('Ctrl Pts',(-3.54785414659174,2.63720135974049,4.9554966407503));
#18793=CARTESIAN_POINT('Ctrl Pts',(-3.37243277255298,2.48483414437987,4.94438285169351));
#18794=CARTESIAN_POINT('Ctrl Pts',(-3.40530626273826,2.25481727477052,4.9332690626367));
#18795=CARTESIAN_POINT('Ctrl Pts',(-3.61638513853951,2.15768779995451,4.9221552735799));
#18796=CARTESIAN_POINT('Ctrl Pts',(-3.81246651125382,2.28234942989398,4.91104148452309));
#18797=CARTESIAN_POINT('Ctrl Pts',(-3.81407487666422,2.51469796087643,4.89992769546629));
#18798=CARTESIAN_POINT('Ctrl Pts',(-3.6197380796992,2.64206214751696,4.88881390640948));
#18799=CARTESIAN_POINT('Ctrl Pts',(-3.40733479453568,2.54786410535795,4.87770011735268));
#18800=CARTESIAN_POINT('Ctrl Pts',(-3.37128015690807,2.3183243706747,4.86658632829587));
#18801=CARTESIAN_POINT('Ctrl Pts',(-3.54457538552076,2.16354326577609,4.85547253923908));
#18802=CARTESIAN_POINT('Ctrl Pts',(-3.76860139232476,2.2251936913151,4.84435875018226));
#18803=CARTESIAN_POINT('Ctrl Pts',(-3.83830463266378,2.44684631363142,4.83324496112547));
#18804=CARTESIAN_POINT('Ctrl Pts',(-3.68988494016744,2.62561997380774,4.82213117206865));
#18805=CARTESIAN_POINT('Ctrl Pts',(-3.45919254257122,2.59788111325323,4.81101738301186));
#18806=CARTESIAN_POINT('Ctrl Pts',(-3.35738280762477,2.38901942561361,4.79990359395505));
#18807=CARTESIAN_POINT('Ctrl Pts',(-3.47764334032546,2.19020838223802,4.78878980489825));
#18808=CARTESIAN_POINT('Ctrl Pts',(-3.70989831124516,2.18342198579874,4.77767601584144));
#18809=CARTESIAN_POINT('Ctrl Pts',(-3.84156211155055,2.3748719019196,4.76656222678464));
#18810=CARTESIAN_POINT('Ctrl Pts',(-3.75212137165305,2.58932185118547,4.75544843772783));
#18811=CARTESIAN_POINT('Ctrl Pts',(-3.52344221510783,2.63048336300545,4.74433464867103));
#18812=CARTESIAN_POINT('Ctrl Pts',(-3.36483726729874,2.46068083880743,4.73322085961422));
#18813=CARTESIAN_POINT('Ctrl Pts',(-3.42147943565789,2.23533645468145,4.72210707055742));
#18814=CARTESIAN_POINT('Ctrl Pts',(-3.64152350112028,2.16071048099716,4.71099328150062));
#18815=CARTESIAN_POINT('Ctrl Pts',(-3.82356063509873,2.30510891778388,4.69987949244381));
#18816=CARTESIAN_POINT('Ctrl Pts',(-3.80097018442129,2.53636223826109,4.68876570338701));
#18817=CARTESIAN_POINT('Ctrl Pts',(-3.59442944478611,2.64280165560495,4.6776519143302));
#18818=CARTESIAN_POINT('Ctrl Pts',(-3.39298749751263,2.52700196401557,4.6665381252734));
#18819=CARTESIAN_POINT('Ctrl Pts',(-3.38102644144724,2.29495593446246,4.65542433621659));
#18820=CARTESIAN_POINT('Ctrl Pts',(-3.56949436685434,2.15905792937668,4.64431054715979));
#18821=CARTESIAN_POINT('Ctrl Pts',(-3.7858844442369,2.24369693400118,4.63319675810299));
#18822=CARTESIAN_POINT('Ctrl Pts',(-3.83213238173679,2.47140190753206,4.62208296904618));
#18823=CARTESIAN_POINT('Ctrl Pts',(-3.66590691767206,2.63375190534549,4.61096917998937));
#18824=CARTESIAN_POINT('Ctrl Pts',(-3.43935610442817,2.58214613327058,4.59985539093257));
#18825=CARTESIAN_POINT('Ctrl Pts',(-3.35984447062414,2.36381993973287,4.58874160187577));
#18826=CARTESIAN_POINT('Ctrl Pts',(-3.50014991641224,2.17860976567263,4.57762781281897));
#18827=CARTESIAN_POINT('Ctrl Pts',(-3.73184927607424,2.1960405838179,4.56651402376216));
#18828=CARTESIAN_POINT('Ctrl Pts',(-3.84286549809491,2.40015776867247,4.55540023470536));
#18829=CARTESIAN_POINT('Ctrl Pts',(-3.73158417538336,2.60413054603043,4.54428644564855));
#18830=CARTESIAN_POINT('Ctrl Pts',(-3.49986236476522,2.62126031969194,4.53317265659175));
#18831=CARTESIAN_POINT('Ctrl Pts',(-3.35979766713961,2.43586801331045,4.52205886753494));
#18832=CARTESIAN_POINT('Ctrl Pts',(-3.43959288921302,2.2176453079079,4.51094507847814));
#18833=CARTESIAN_POINT('Ctrl Pts',(-3.66621055822496,2.16633391955349,4.49983128942134));
#18834=CARTESIAN_POINT('Ctrl Pts',(-3.83222495382674,2.32889974592014,4.48871750036453));
#18835=CARTESIAN_POINT('Ctrl Pts',(-3.78568121275365,2.55654443850517,4.47760371130773));
#18836=CARTESIAN_POINT('Ctrl Pts',(-3.56918135753979,2.64090223654315,4.46648992225092));
#18837=CARTESIAN_POINT('Ctrl Pts',(-3.38089014394226,2.50475947474088,4.45537613319412));
#18838=CARTESIAN_POINT('Ctrl Pts',(-3.3931526891646,2.27272919910994,4.44426234413731));
#18839=CARTESIAN_POINT('Ctrl Pts',(-3.59474487835949,2.15719128792351,4.43314855508051));
#18840=CARTESIAN_POINT('Ctrl Pts',(-3.80114723098,2.26389903055612,4.4220347660237));
#18841=CARTESIAN_POINT('Ctrl Pts',(-3.82343705972838,2.49518136177793,4.4109209769669));
#18842=CARTESIAN_POINT('Ctrl Pts',(-3.64121277856108,2.63934345799643,4.3998071879101));
#18843=CARTESIAN_POINT('Ctrl Pts',(-3.4212652433475,2.56443108225311,4.38869339885329));
#18844=CARTESIAN_POINT('Ctrl Pts',(-3.36491712045917,2.33901445477475,4.3775796097965));
#18845=CARTESIAN_POINT('Ctrl Pts',(-3.52374009472539,2.16941582002738,4.36646582073968));
#18846=CARTESIAN_POINT('Ctrl Pts',(-3.75237048890211,2.21087904346051,4.35535203168288));
#18847=CARTESIAN_POINT('Ctrl Pts',(-3.84152270551859,2.42543572391857,4.34423824262608));
#18848=CARTESIAN_POINT('Ctrl Pts',(-3.70962996035205,2.61673302206395,4.33312445356927));
#18849=CARTESIAN_POINT('Ctrl Pts',(-3.47734458963256,2.60960762555316,4.32201066451247));
#18850=CARTESIAN_POINT('Ctrl Pts',(-3.35742145615876,2.41071512444121,4.31089687545567));
#18851=CARTESIAN_POINT('Ctrl Pts',(-3.45934316515028,2.20183612882053,4.29978308639885));
#18852=CARTESIAN_POINT('Ctrl Pts',(-3.69040350703126,2.17470170179864,4.28866929734206));
#18853=CARTESIAN_POINT('Ctrl Pts',(-3.7885754343637,2.29356865430552,4.28126010463752));
#18854=CARTESIAN_POINT('Ctrl Pts',(-3.80166758614466,2.36062792457102,4.27755550828525));
#18855=CARTESIAN_POINT('Ctrl Pts',(-3.64967348970877,2.21400211999972,5.20748149723825));
#18856=CARTESIAN_POINT('Ctrl Pts',(-3.71152220988337,2.2305197371096,5.20377690088598));
#18857=CARTESIAN_POINT('Ctrl Pts',(-3.81636896167925,2.32987270138258,5.19636770818145));
#18858=CARTESIAN_POINT('Ctrl Pts',(-3.7762589230805,2.54412670398045,5.18525391912464));
#18859=CARTESIAN_POINT('Ctrl Pts',(-3.57450297532427,2.62606859592404,5.17414013006784));
#18860=CARTESIAN_POINT('Ctrl Pts',(-3.39623976792153,2.50127640086039,5.16302634101103));
#18861=CARTESIAN_POINT('Ctrl Pts',(-3.404403315861,2.28369088559113,5.15191255195423));
#18862=CARTESIAN_POINT('Ctrl Pts',(-3.59163732076848,2.17261126982347,5.14079876289742));
#18863=CARTESIAN_POINT('Ctrl Pts',(-3.78650650684933,2.26963974340016,5.12968497384063));
#18864=CARTESIAN_POINT('Ctrl Pts',(-3.8106737979302,2.48600012163341,5.11857118478381));
#18865=CARTESIAN_POINT('Ctrl Pts',(-3.64200416517759,2.62363777825967,5.10745739572702));
#18866=CARTESIAN_POINT('Ctrl Pts',(-3.43489004460608,2.55658015434777,5.0963436066702));
#18867=CARTESIAN_POINT('Ctrl Pts',(-3.37890173959752,2.34620148403342,5.0852298176134));
#18868=CARTESIAN_POINT('Ctrl Pts',(-3.52528777861237,2.18506593235721,5.0741160285566));
#18869=CARTESIAN_POINT('Ctrl Pts',(-3.74005846207577,2.22066160730187,5.06300223949979));
#18870=CARTESIAN_POINT('Ctrl Pts',(-3.82663219619914,2.42040792821545,5.05188845044299));
#18871=CARTESIAN_POINT('Ctrl Pts',(-3.70576683635895,2.60147455044772,5.04077466138619));
#18872=CARTESIAN_POINT('Ctrl Pts',(-3.4880919289783,2.59812927699836,5.02966087232938));
#18873=CARTESIAN_POINT('Ctrl Pts',(-3.37284772952088,2.41343400678959,5.01854708327258));
#18874=CARTESIAN_POINT('Ctrl Pts',(-3.46551858860765,2.21644244909332,5.00743329421577));
#18875=CARTESIAN_POINT('Ctrl Pts',(-3.68128180402377,2.18746319379313,4.99631950515897));
#18876=CARTESIAN_POINT('Ctrl Pts',(-3.82264686473641,2.35302129035867,4.98520571610216));
#18877=CARTESIAN_POINT('Ctrl Pts',(-3.76022072401106,2.56157953122871,4.97409192704537));
#18878=CARTESIAN_POINT('Ctrl Pts',(-3.55114273814991,2.6222421954303,4.96297813798855));
#18879=CARTESIAN_POINT('Ctrl Pts',(-3.38678435785046,2.47948405740616,4.95186434893176));
#18880=CARTESIAN_POINT('Ctrl Pts',(-3.41758467298453,2.26397326040267,4.94075055987495));
#18881=CARTESIAN_POINT('Ctrl Pts',(-3.61535180559434,2.17296928071335,4.92963677081814));
#18882=CARTESIAN_POINT('Ctrl Pts',(-3.79906725647832,2.28976909313423,4.91852298176134));
#18883=CARTESIAN_POINT('Ctrl Pts',(-3.80057418991348,2.50746450469106,4.90740919270453));
#18884=CARTESIAN_POINT('Ctrl Pts',(-3.61849329266379,2.62679643638467,4.89629540364773));
#18885=CARTESIAN_POINT('Ctrl Pts',(-3.41948527490624,2.53853901780343,4.88518161459093));
#18886=CARTESIAN_POINT('Ctrl Pts',(-3.38570443220547,2.32347526509011,4.87406782553412));
#18887=CARTESIAN_POINT('Ctrl Pts',(-3.54807075298295,2.17845547008797,4.86295403647732));
#18888=CARTESIAN_POINT('Ctrl Pts',(-3.7579685024734,2.23621789580084,4.85184024742051));
#18889=CARTESIAN_POINT('Ctrl Pts',(-3.82327589016501,2.44389193890226,4.84072645836371));
#18890=CARTESIAN_POINT('Ctrl Pts',(-3.6842163234679,2.61139119255816,4.8296126693069));
#18891=CARTESIAN_POINT('Ctrl Pts',(-3.4680726008225,2.58540169032632,4.8184988802501));
#18892=CARTESIAN_POINT('Ctrl Pts',(-3.37268352280275,2.38971191834066,4.8073850911933));
#18893=CARTESIAN_POINT('Ctrl Pts',(-3.48535979430583,2.20343894417256,4.79627130213649));
#18894=CARTESIAN_POINT('Ctrl Pts',(-3.70296754618914,2.19708053355731,4.78515751307969));
#18895=CARTESIAN_POINT('Ctrl Pts',(-3.82632793531414,2.37645661184032,4.77404372402288));
#18896=CARTESIAN_POINT('Ctrl Pts',(-3.74252779851275,2.57738222030606,4.76292993496608));
#18897=CARTESIAN_POINT('Ctrl Pts',(-3.52827035135747,2.61594787087447,4.75181614590928));
#18898=CARTESIAN_POINT('Ctrl Pts',(-3.37966786507423,2.45685398621605,4.74070235685247));
#18899=CARTESIAN_POINT('Ctrl Pts',(-3.43273788062492,2.24572100320602,4.72958856779567));
#18900=CARTESIAN_POINT('Ctrl Pts',(-3.63890481092106,2.17580133560435,4.71847477873887));
#18901=CARTESIAN_POINT('Ctrl Pts',(-3.80946172657059,2.31109324810979,4.70736098968206));
#18902=CARTESIAN_POINT('Ctrl Pts',(-3.78829594843252,2.5277625188915,4.69624720062526));
#18903=CARTESIAN_POINT('Ctrl Pts',(-3.59478075327286,2.62748930720629,4.68513341156845));
#18904=CARTESIAN_POINT('Ctrl Pts',(-3.40604279383286,2.51899255273097,4.67401962251165));
#18905=CARTESIAN_POINT('Ctrl Pts',(-3.39483606482192,2.30158056527362,4.66290583345485));
#18906=CARTESIAN_POINT('Ctrl Pts',(-3.57141821239684,2.17425300257371,4.65179204439804));
#18907=CARTESIAN_POINT('Ctrl Pts',(-3.77416159430429,2.253554226763,4.64067825534124));
#18908=CARTESIAN_POINT('Ctrl Pts',(-3.81749289381852,2.46689892800445,4.62956446628442));
#18909=CARTESIAN_POINT('Ctrl Pts',(-3.66175048108285,2.61901028175737,4.61845067722763));
#18910=CARTESIAN_POINT('Ctrl Pts',(-3.44948715271524,2.57065904087346,4.60733688817082));
#18911=CARTESIAN_POINT('Ctrl Pts',(-3.37498994039659,2.36610164447049,4.59622309911403));
#18912=CARTESIAN_POINT('Ctrl Pts',(-3.50644698742571,2.19257179732202,4.58510931005721));
#18913=CARTESIAN_POINT('Ctrl Pts',(-3.72353416781713,2.20890333647083,4.57399552100042));
#18914=CARTESIAN_POINT('Ctrl Pts',(-3.82754912345333,2.40014781895086,4.5628817319436));
#18915=CARTESIAN_POINT('Ctrl Pts',(-3.723285785769,2.59125700102993,4.55176794288681));
#18916=CARTESIAN_POINT('Ctrl Pts',(-3.50617757029671,2.60730648114219,4.54065415382999));
#18917=CARTESIAN_POINT('Ctrl Pts',(-3.37494608858577,2.43360598789383,4.52954036477319));
#18918=CARTESIAN_POINT('Ctrl Pts',(-3.44970900460718,2.22914555312034,4.51842657571639));
#18919=CARTESIAN_POINT('Ctrl Pts',(-3.66203497246676,2.18107013057245,4.50731278665959));
#18920=CARTESIAN_POINT('Ctrl Pts',(-3.81757962782599,2.33338370159577,4.49619899760278));
#18921=CARTESIAN_POINT('Ctrl Pts',(-3.77397117966642,2.54667192352462,4.48508520854598));
#18922=CARTESIAN_POINT('Ctrl Pts',(-3.57112494309463,2.62570967549255,4.47397141948917));
#18923=CARTESIAN_POINT('Ctrl Pts',(-3.3947083629539,2.49815279172096,4.46285763043237));
#18924=CARTESIAN_POINT('Ctrl Pts',(-3.40619756763113,2.28075556466066,4.45174384137556));
#18925=CARTESIAN_POINT('Ctrl Pts',(-3.59507629394739,2.17250408134035,4.44063005231876));
#18926=CARTESIAN_POINT('Ctrl Pts',(-3.78846182950481,2.27248227294105,4.42951626326195));
#18927=CARTESIAN_POINT('Ctrl Pts',(-3.80934594451251,2.48917872489734,4.41840247420516));
#18928=CARTESIAN_POINT('Ctrl Pts',(-3.63861368415939,2.62424920171285,4.40728868514834));
#18929=CARTESIAN_POINT('Ctrl Pts',(-3.43253719640727,2.55406119407111,4.39617489609155));
#18930=CARTESIAN_POINT('Ctrl Pts',(-3.37974268227471,2.34286052375416,4.38506110703474));
#18931=CARTESIAN_POINT('Ctrl Pts',(-3.5285494451209,2.18395767020613,4.37394731797793));
#18932=CARTESIAN_POINT('Ctrl Pts',(-3.74276120511889,2.22280600486777,4.36283352892113));
#18933=CARTESIAN_POINT('Ctrl Pts',(-3.82629101443365,2.42383161349583,4.35171973986432));
#18934=CARTESIAN_POINT('Ctrl Pts',(-3.70271611891361,2.60306469869495,4.34060595080752));
#18935=CARTESIAN_POINT('Ctrl Pts',(-3.48507988440164,2.59638866713425,4.32949216175072));
#18936=CARTESIAN_POINT('Ctrl Pts',(-3.37271973395708,2.41003937238272,4.31837837269391));
#18937=CARTESIAN_POINT('Ctrl Pts',(-3.46821372435015,2.21433338394825,4.30726458363711));
#18938=CARTESIAN_POINT('Ctrl Pts',(-3.68470218678007,2.18891019649399,4.2961507945803));
#18939=CARTESIAN_POINT('Ctrl Pts',(-3.77668287645173,2.30028077429396,4.28874160187577));
#18940=CARTESIAN_POINT('Ctrl Pts',(-3.78894936833816,2.36311093455975,4.2850370055235));
#18941=CARTESIAN_POINT('Ctrl Pts',(-3.64632995769868,2.22652167256662,5.2149629944765));
#18942=CARTESIAN_POINT('Ctrl Pts',(-3.70401562879218,2.24192748573719,5.21125839812423));
#18943=CARTESIAN_POINT('Ctrl Pts',(-3.80180512584637,2.33459298314823,5.2038492054197));
#18944=CARTESIAN_POINT('Ctrl Pts',(-3.76439490155032,2.53442550820997,5.19273541636289));
#18945=CARTESIAN_POINT('Ctrl Pts',(-3.57621918488928,2.61085187587115,5.18162162730609));
#18946=CARTESIAN_POINT('Ctrl Pts',(-3.40995490777444,2.49445946711708,5.17050783824928));
#18947=CARTESIAN_POINT('Ctrl Pts',(-3.41756896575436,2.2915196741335,5.15939404919248));
#18948=CARTESIAN_POINT('Ctrl Pts',(-3.59220021429306,2.18791684836318,5.14828026013568));
#18949=CARTESIAN_POINT('Ctrl Pts',(-3.7739527185128,2.27841431698741,5.13716647107887));
#18950=CARTESIAN_POINT('Ctrl Pts',(-3.79649330464903,2.48021143714115,5.12605268202206));
#18951=CARTESIAN_POINT('Ctrl Pts',(-3.63917685685576,2.60858467700464,5.11493889296527));
#18952=CARTESIAN_POINT('Ctrl Pts',(-3.44600362700749,2.54604071447196,5.10382510390845));
#18953=CARTESIAN_POINT('Ctrl Pts',(-3.39378390542411,2.349822672343,5.09271131485166));
#18954=CARTESIAN_POINT('Ctrl Pts',(-3.53031667239896,2.19953318520045,5.08159752579485));
#18955=CARTESIAN_POINT('Ctrl Pts',(-3.73063110043921,2.23273290851586,5.07048373673805));
#18956=CARTESIAN_POINT('Ctrl Pts',(-3.81137754010487,2.41903426669804,5.05936994768123));
#18957=CARTESIAN_POINT('Ctrl Pts',(-3.69864765055087,2.58791326025872,5.04825615862444));
#18958=CARTESIAN_POINT('Ctrl Pts',(-3.49562448245587,2.58479315779948,5.03714236956762));
#18959=CARTESIAN_POINT('Ctrl Pts',(-3.38813739191354,2.41252976124558,5.02602858051083));
#18960=CARTESIAN_POINT('Ctrl Pts',(-3.47457055790533,2.22879774264625,5.01491479145402));
#18961=CARTESIAN_POINT('Ctrl Pts',(-3.67581071038439,2.20176908651461,5.00380100239723));
#18962=CARTESIAN_POINT('Ctrl Pts',(-3.8076604620585,2.35618343621151,4.99268721334041));
#18963=CARTESIAN_POINT('Ctrl Pts',(-3.74943623670099,2.5507035823472,4.98157342428361));
#18964=CARTESIAN_POINT('Ctrl Pts',(-3.55443132970808,2.6072830311201,4.97045963522681));
#18965=CARTESIAN_POINT('Ctrl Pts',(-3.40113594314794,2.47413397043246,4.95934584617));
#18966=CARTESIAN_POINT('Ctrl Pts',(-3.42986308323079,2.27312924603482,4.9482320571132));
#18967=CARTESIAN_POINT('Ctrl Pts',(-3.61431847264918,2.18825076147219,4.93711826805639));
#18968=CARTESIAN_POINT('Ctrl Pts',(-3.78566800170281,2.29718875637448,4.92600447899959));
#18969=CARTESIAN_POINT('Ctrl Pts',(-3.78707350316275,2.50023104850568,4.91489068994278));
#18970=CARTESIAN_POINT('Ctrl Pts',(-3.61724850562837,2.61153072525238,4.90377690088598));
#18971=CARTESIAN_POINT('Ctrl Pts',(-3.43163575527681,2.52921393024892,4.89266311182917));
#18972=CARTESIAN_POINT('Ctrl Pts',(-3.40012870750287,2.32862615950552,4.88154932277238));
#18973=CARTESIAN_POINT('Ctrl Pts',(-3.55156612044514,2.19336767439986,4.87043553371556));
#18974=CARTESIAN_POINT('Ctrl Pts',(-3.74733561262204,2.24724210028659,4.85932174465877));
#18975=CARTESIAN_POINT('Ctrl Pts',(-3.80824714766624,2.4409375641731,4.84820795560196));
#18976=CARTESIAN_POINT('Ctrl Pts',(-3.67854770676838,2.59716241130857,4.83709416654516));
#18977=CARTESIAN_POINT('Ctrl Pts',(-3.47695265907377,2.57292226739941,4.82598037748835));
#18978=CARTESIAN_POINT('Ctrl Pts',(-3.38798423798073,2.39040441106771,4.81486658843155));
#18979=CARTESIAN_POINT('Ctrl Pts',(-3.49307624828619,2.2166695061071,4.80375279937474));
#18980=CARTESIAN_POINT('Ctrl Pts',(-3.69603678113312,2.21073908131588,4.79263901031794));
#18981=CARTESIAN_POINT('Ctrl Pts',(-3.81109375907773,2.37804132176103,4.78152522126113));
#18982=CARTESIAN_POINT('Ctrl Pts',(-3.73293422537244,2.56544258942666,4.77041143220433));
#18983=CARTESIAN_POINT('Ctrl Pts',(-3.5330984876071,2.6014123787435,4.75929764314753));
#18984=CARTESIAN_POINT('Ctrl Pts',(-3.39449846284973,2.45302713362467,4.74818385409072));
#18985=CARTESIAN_POINT('Ctrl Pts',(-3.44399632559195,2.2561055517306,4.73707006503392));
#18986=CARTESIAN_POINT('Ctrl Pts',(-3.63628612072185,2.19089219021153,4.72595627597712));
#18987=CARTESIAN_POINT('Ctrl Pts',(-3.79536281804244,2.31707757843571,4.7148424869203));
#18988=CARTESIAN_POINT('Ctrl Pts',(-3.77562171244375,2.5191627995219,4.70372869786351));
#18989=CARTESIAN_POINT('Ctrl Pts',(-3.5951320617596,2.61217695880763,4.6926149088067));
#18990=CARTESIAN_POINT('Ctrl Pts',(-3.41909809015308,2.51098314144638,4.6815011197499));
#18991=CARTESIAN_POINT('Ctrl Pts',(-3.40864568819661,2.30820519608479,4.67038733069309));
#18992=CARTESIAN_POINT('Ctrl Pts',(-3.57334205793934,2.18944807577074,4.65927354163629));
#18993=CARTESIAN_POINT('Ctrl Pts',(-3.76243874437168,2.26341151952482,4.64815975257949));
#18994=CARTESIAN_POINT('Ctrl Pts',(-3.80285340590026,2.46239594847684,4.63704596352267));
#18995=CARTESIAN_POINT('Ctrl Pts',(-3.65759404449364,2.60426865816925,4.62593217446588));
#18996=CARTESIAN_POINT('Ctrl Pts',(-3.45961820100231,2.55917194847634,4.61481838540907));
#18997=CARTESIAN_POINT('Ctrl Pts',(-3.39013541016905,2.3683833492081,4.60370459635227));
#18998=CARTESIAN_POINT('Ctrl Pts',(-3.51274405843916,2.20653382897141,4.59259080729546));
#18999=CARTESIAN_POINT('Ctrl Pts',(-3.71521905956003,2.22176608912375,4.58147701823867));
#19000=CARTESIAN_POINT('Ctrl Pts',(-3.81223274881174,2.40013786922925,4.57036322918185));
#19001=CARTESIAN_POINT('Ctrl Pts',(-3.71498739615465,2.57838345602943,4.55924944012506));
#19002=CARTESIAN_POINT('Ctrl Pts',(-3.51249277582821,2.59335264259245,4.54813565106824));
#19003=CARTESIAN_POINT('Ctrl Pts',(-3.39009451003192,2.4313439624772,4.53702186201144));
#19004=CARTESIAN_POINT('Ctrl Pts',(-3.45982512000134,2.24064579833279,4.52590807295464));
#19005=CARTESIAN_POINT('Ctrl Pts',(-3.65785938670857,2.1958063415914,4.51479428389783));
#19006=CARTESIAN_POINT('Ctrl Pts',(-3.80293430182523,2.33786765727141,4.50368049484103));
#19007=CARTESIAN_POINT('Ctrl Pts',(-3.76226114657918,2.53679940854407,4.49256670578423));
#19008=CARTESIAN_POINT('Ctrl Pts',(-3.57306852864947,2.61051711444195,4.48145291672742));
#19009=CARTESIAN_POINT('Ctrl Pts',(-3.40852658196552,2.49154610870105,4.47033912767061));
#19010=CARTESIAN_POINT('Ctrl Pts',(-3.41924244609765,2.28878193021138,4.45922533861382));
#19011=CARTESIAN_POINT('Ctrl Pts',(-3.5954077095353,2.18781687475719,4.44811154955701));
#19012=CARTESIAN_POINT('Ctrl Pts',(-3.77577642802961,2.28106551532598,4.43699776050021));
#19013=CARTESIAN_POINT('Ctrl Pts',(-3.79525482929664,2.48317608801675,4.4258839714434));
#19014=CARTESIAN_POINT('Ctrl Pts',(-3.6360145897577,2.60915494542926,4.4147701823866));
#19015=CARTESIAN_POINT('Ctrl Pts',(-3.44380914946703,2.54369130588911,4.40365639332979));
#19016=CARTESIAN_POINT('Ctrl Pts',(-3.39456824409026,2.34670659273357,4.39254260427299));
#19017=CARTESIAN_POINT('Ctrl Pts',(-3.53335879551641,2.19849952038487,4.38142881521618));
#19018=CARTESIAN_POINT('Ctrl Pts',(-3.73315192133567,2.23473296627504,4.37031502615938));
#19019=CARTESIAN_POINT('Ctrl Pts',(-3.81105932334871,2.4222275030731,4.35920123710257));
#19020=CARTESIAN_POINT('Ctrl Pts',(-3.69580227747518,2.58939637532595,4.34808744804577));
#19021=CARTESIAN_POINT('Ctrl Pts',(-3.49281517917073,2.58316970871533,4.33697365898897));
#19022=CARTESIAN_POINT('Ctrl Pts',(-3.38801801175539,2.40936362032424,4.32585986993216));
#19023=CARTESIAN_POINT('Ctrl Pts',(-3.47708428355003,2.22683063907596,4.31474608087536));
#19024=CARTESIAN_POINT('Ctrl Pts',(-3.67900086652888,2.20311869118934,4.30363229181856));
#19025=CARTESIAN_POINT('Ctrl Pts',(-3.76479031853975,2.3069928942824,4.29622309911402));
#19026=CARTESIAN_POINT('Ctrl Pts',(-3.77623115053166,2.36559394454847,4.29251850276175));
#19027=CARTESIAN_POINT('Ctrl Pts',(-3.64298642568859,2.23904122513352,5.22244449171475));
#19028=CARTESIAN_POINT('Ctrl Pts',(-3.69650904770099,2.25333523436478,5.21873989536248));
#19029=CARTESIAN_POINT('Ctrl Pts',(-3.78724129001348,2.33931326491388,5.21133070265794));
#19030=CARTESIAN_POINT('Ctrl Pts',(-3.75253088002014,2.52472431243949,5.20021691360114));
#19031=CARTESIAN_POINT('Ctrl Pts',(-3.57793539445428,2.59563515581826,5.18910312454433));
#19032=CARTESIAN_POINT('Ctrl Pts',(-3.42367004762736,2.48764253337377,5.17798933548753));
#19033=CARTESIAN_POINT('Ctrl Pts',(-3.4307346156477,2.29934846267587,5.16687554643072));
#19034=CARTESIAN_POINT('Ctrl Pts',(-3.59276310781765,2.2032224269029,5.15576175737392));
#19035=CARTESIAN_POINT('Ctrl Pts',(-3.76139893017626,2.28718889057467,5.14464796831712));
#19036=CARTESIAN_POINT('Ctrl Pts',(-3.78231281136787,2.47442275264891,5.13353417926031));
#19037=CARTESIAN_POINT('Ctrl Pts',(-3.63634954853391,2.5935315757496,5.12242039020352));
#19038=CARTESIAN_POINT('Ctrl Pts',(-3.45711720940891,2.53550127459616,5.1113066011467));
#19039=CARTESIAN_POINT('Ctrl Pts',(-3.4086660712507,2.35344386065259,5.1001928120899));
#19040=CARTESIAN_POINT('Ctrl Pts',(-3.53534556618555,2.21400043804369,5.0890790230331));
#19041=CARTESIAN_POINT('Ctrl Pts',(-3.72120373880265,2.24480420972985,5.07796523397629));
#19042=CARTESIAN_POINT('Ctrl Pts',(-3.79612288401061,2.41766060518064,5.06685144491949));
#19043=CARTESIAN_POINT('Ctrl Pts',(-3.6915284647428,2.57435197006973,5.05573765586269));
#19044=CARTESIAN_POINT('Ctrl Pts',(-3.50315703593343,2.5714570386006,5.04462386680588));
#19045=CARTESIAN_POINT('Ctrl Pts',(-3.40342705430619,2.41162551570156,5.03351007774908));
#19046=CARTESIAN_POINT('Ctrl Pts',(-3.48362252720301,2.24115303619919,5.02239628869227));
#19047=CARTESIAN_POINT('Ctrl Pts',(-3.67033961674501,2.21607497923609,5.01128249963547));
#19048=CARTESIAN_POINT('Ctrl Pts',(-3.79267405938058,2.35934558206435,5.00016871057866));
#19049=CARTESIAN_POINT('Ctrl Pts',(-3.73865174939092,2.53982763346569,4.98905492152186));
#19050=CARTESIAN_POINT('Ctrl Pts',(-3.55771992126626,2.59232386680991,4.97794113246505));
#19051=CARTESIAN_POINT('Ctrl Pts',(-3.41548752844543,2.46878388345875,4.96682734340825));
#19052=CARTESIAN_POINT('Ctrl Pts',(-3.44214149347704,2.28228523166696,4.95571355435145));
#19053=CARTESIAN_POINT('Ctrl Pts',(-3.61328513970402,2.20353224223104,4.94459976529464));
#19054=CARTESIAN_POINT('Ctrl Pts',(-3.7722687469273,2.30460841961473,4.93348597623784));
#19055=CARTESIAN_POINT('Ctrl Pts',(-3.77357281641202,2.4929975923203,4.92237218718104));
#19056=CARTESIAN_POINT('Ctrl Pts',(-3.61600371859295,2.59626501412009,4.91125839812423));
#19057=CARTESIAN_POINT('Ctrl Pts',(-3.44378623564737,2.51988884269441,4.90014460906743));
#19058=CARTESIAN_POINT('Ctrl Pts',(-3.41455298280027,2.33377705392094,4.88903082001062));
#19059=CARTESIAN_POINT('Ctrl Pts',(-3.55506148790733,2.20827987871175,4.87791703095382));
#19060=CARTESIAN_POINT('Ctrl Pts',(-3.73670272277068,2.25826630477233,4.86680324189701));
#19061=CARTESIAN_POINT('Ctrl Pts',(-3.79321840516747,2.43798318944394,4.85568945284021));
#19062=CARTESIAN_POINT('Ctrl Pts',(-3.67287909006884,2.58293363005899,4.8445756637834));
#19063=CARTESIAN_POINT('Ctrl Pts',(-3.48583271732505,2.5604428444725,4.8334618747266));
#19064=CARTESIAN_POINT('Ctrl Pts',(-3.40328495315871,2.39109690379476,4.8223480856698));
#19065=CARTESIAN_POINT('Ctrl Pts',(-3.50079270226656,2.22990006804163,4.81123429661299));
#19066=CARTESIAN_POINT('Ctrl Pts',(-3.68910601607711,2.22439762907444,4.80012050755619));
#19067=CARTESIAN_POINT('Ctrl Pts',(-3.79585958284132,2.37962603168174,4.78900671849938));
#19068=CARTESIAN_POINT('Ctrl Pts',(-3.72334065223214,2.55350295854726,4.77789292944258));
#19069=CARTESIAN_POINT('Ctrl Pts',(-3.53792662385674,2.58687688661252,4.76677914038578));
#19070=CARTESIAN_POINT('Ctrl Pts',(-3.40932906062523,2.4492002810333,4.75566535132897));
#19071=CARTESIAN_POINT('Ctrl Pts',(-3.45525477055898,2.26649010025516,4.74455156227217));
#19072=CARTESIAN_POINT('Ctrl Pts',(-3.63366743052263,2.20598304481872,4.73343777321536));
#19073=CARTESIAN_POINT('Ctrl Pts',(-3.7812639095143,2.32306190876162,4.72232398415856));
#19074=CARTESIAN_POINT('Ctrl Pts',(-3.76294747645498,2.51056308015232,4.71121019510176));
#19075=CARTESIAN_POINT('Ctrl Pts',(-3.59548337024634,2.59686461040897,4.70009640604495));
#19076=CARTESIAN_POINT('Ctrl Pts',(-3.43215338647331,2.50297373016179,4.68898261698815));
#19077=CARTESIAN_POINT('Ctrl Pts',(-3.42245531157129,2.31482982689595,4.67786882793134));
#19078=CARTESIAN_POINT('Ctrl Pts',(-3.57526590348185,2.20464314896778,4.66675503887454));
#19079=CARTESIAN_POINT('Ctrl Pts',(-3.75071589443907,2.27326881228664,4.65564124981773));
#19080=CARTESIAN_POINT('Ctrl Pts',(-3.78821391798199,2.45789296894922,4.64452746076093));
#19081=CARTESIAN_POINT('Ctrl Pts',(-3.65343760790444,2.58952703458114,4.63341367170412));
#19082=CARTESIAN_POINT('Ctrl Pts',(-3.46974924928937,2.54768485607922,4.62229988264733));
#19083=CARTESIAN_POINT('Ctrl Pts',(-3.40528087994151,2.37066505394572,4.61118609359051));
#19084=CARTESIAN_POINT('Ctrl Pts',(-3.51904112945263,2.2204958606208,4.60007230453372));
#19085=CARTESIAN_POINT('Ctrl Pts',(-3.70690395130293,2.23462884177668,4.58895851547691));
#19086=CARTESIAN_POINT('Ctrl Pts',(-3.79691637417015,2.40012791950764,4.57784472642011));
#19087=CARTESIAN_POINT('Ctrl Pts',(-3.7066890065403,2.56550991102893,4.5667309373633));
#19088=CARTESIAN_POINT('Ctrl Pts',(-3.5188079813597,2.57939880404271,4.55561714830649));
#19089=CARTESIAN_POINT('Ctrl Pts',(-3.40524293147808,2.42908193706057,4.54450335924969));
#19090=CARTESIAN_POINT('Ctrl Pts',(-3.4699412353955,2.25214604354523,4.53338957019289));
#19091=CARTESIAN_POINT('Ctrl Pts',(-3.65368380095038,2.21054255261035,4.52227578113608));
#19092=CARTESIAN_POINT('Ctrl Pts',(-3.78828897582448,2.34235161294705,4.51116199207928));
#19093=CARTESIAN_POINT('Ctrl Pts',(-3.75055111349195,2.52692689356351,4.50004820302248));
#19094=CARTESIAN_POINT('Ctrl Pts',(-3.57501211420431,2.59532455339135,4.48893441396567));
#19095=CARTESIAN_POINT('Ctrl Pts',(-3.42234480097716,2.48493942568113,4.47782062490887));
#19096=CARTESIAN_POINT('Ctrl Pts',(-3.43228732456417,2.29680829576209,4.46670683585206));
#19097=CARTESIAN_POINT('Ctrl Pts',(-3.5957391251232,2.20312966817403,4.45559304679526));
#19098=CARTESIAN_POINT('Ctrl Pts',(-3.76309102655441,2.2896487577109,4.44447925773845));
#19099=CARTESIAN_POINT('Ctrl Pts',(-3.78116371408077,2.47717345113617,4.43336546868165));
#19100=CARTESIAN_POINT('Ctrl Pts',(-3.63341549535601,2.59406068914566,4.42225167962485));
#19101=CARTESIAN_POINT('Ctrl Pts',(-3.4550811025268,2.53332141770711,4.41113789056804));
#19102=CARTESIAN_POINT('Ctrl Pts',(-3.40939380590581,2.35055266171297,4.40002410151124));
#19103=CARTESIAN_POINT('Ctrl Pts',(-3.53816814591191,2.21304137056363,4.38891031245443));
#19104=CARTESIAN_POINT('Ctrl Pts',(-3.72354263755246,2.2466599276823,4.37779652339763));
#19105=CARTESIAN_POINT('Ctrl Pts',(-3.79582763226376,2.42062339265036,4.36668273434082));
#19106=CARTESIAN_POINT('Ctrl Pts',(-3.68888843603675,2.57572805195694,4.35556894528402));
#19107=CARTESIAN_POINT('Ctrl Pts',(-3.50055047393982,2.56995075029642,4.34445515622722));
#19108=CARTESIAN_POINT('Ctrl Pts',(-3.40331628955371,2.40868786826575,4.33334136717041));
#19109=CARTESIAN_POINT('Ctrl Pts',(-3.4859548427499,2.23932789420368,4.32222757811361));
#19110=CARTESIAN_POINT('Ctrl Pts',(-3.67329954627769,2.21732718588468,4.3111137890568));
#19111=CARTESIAN_POINT('Ctrl Pts',(-3.75289776062778,2.31370501427084,4.30370459635227));
#19112=CARTESIAN_POINT('Ctrl Pts',(-3.76351293272515,2.3680769545372,4.3));
#19113=CARTESIAN_POINT('Ctrl Pts',(-3.76638442018051,2.4000942147675,5.13785196366098));
#19114=CARTESIAN_POINT('Ctrl Pts',(-3.76649613151981,2.42168271873493,5.13641270219409));
#19115=CARTESIAN_POINT('Ctrl Pts',(-3.76259704654914,2.44323253526348,5.1349734407272));
#19116=CARTESIAN_POINT('Ctrl Pts',(-3.75449995403028,2.46306857948665,5.13353417926031));
#19117=CARTESIAN_POINT('Ctrl Pts',(-3.73365839042322,2.51412569368247,5.12982958290804));
#19118=CARTESIAN_POINT('Ctrl Pts',(-3.68500396947857,2.55382863471604,5.12612498655578));
#19119=CARTESIAN_POINT('Ctrl Pts',(-3.63080470248541,2.56400838837391,5.12242039020351));
#19120=CARTESIAN_POINT('Ctrl Pts',(-3.57660543549225,2.57418814203179,5.11871579385124));
#19121=CARTESIAN_POINT('Ctrl Pts',(-3.51686132245058,2.55484470831398,5.11501119749897));
#19122=CARTESIAN_POINT('Ctrl Pts',(-3.47891407623671,2.51483008913114,5.1113066011467));
#19123=CARTESIAN_POINT('Ctrl Pts',(-3.44096683002284,2.47481546994831,5.10760200479444));
#19124=CARTESIAN_POINT('Ctrl Pts',(-3.42481645063677,2.41412966530045,5.10389740844217));
#19125=CARTESIAN_POINT('Ctrl Pts',(-3.43785451009954,2.3605461925417,5.1001928120899));
#19126=CARTESIAN_POINT('Ctrl Pts',(-3.45089256956232,2.30696271978295,5.09648821573763));
#19127=CARTESIAN_POINT('Ctrl Pts',(-3.49311906787393,2.26048157891332,5.09278361938537));
#19128=CARTESIAN_POINT('Ctrl Pts',(-3.54520867913259,2.2423749704262,5.0890790230331));
#19129=CARTESIAN_POINT('Ctrl Pts',(-3.59729829039125,2.22426836193908,5.08537442668083));
#19130=CARTESIAN_POINT('Ctrl Pts',(-3.65925101459695,2.23453628583446,5.08166983032856));
#19131=CARTESIAN_POINT('Ctrl Pts',(-3.70271390090113,2.26847964702395,5.07796523397629));
#19132=CARTESIAN_POINT('Ctrl Pts',(-3.74226404132859,2.29936725748381,5.07459414387119));
#19133=CARTESIAN_POINT('Ctrl Pts',(-3.76650358790754,2.34985942080815,5.07122305376608));
#19134=CARTESIAN_POINT('Ctrl Pts',(-3.76682061973634,2.40008640134019,5.06785196366098));
#19135=CARTESIAN_POINT('Ctrl Pts',(-3.65301702171886,2.20148256743283,5.2));
#19136=CARTESIAN_POINT('Ctrl Pts',(-3.66542047547214,2.20607510650608,5.2));
#19137=CARTESIAN_POINT('Ctrl Pts',(-3.67726977303962,2.21193437262237,5.2));
#19138=CARTESIAN_POINT('Ctrl Pts',(-3.688447163997,2.21889712590693,5.2));
#19139=CARTESIAN_POINT('Ctrl Pts',(-3.69411334108481,2.22242676831449,5.2));
#19140=CARTESIAN_POINT('Ctrl Pts',(-3.69960641439008,2.22624073198774,5.2));
#19141=CARTESIAN_POINT('Ctrl Pts',(-3.70490760860864,2.23032132776193,5.2));
#19142=CARTESIAN_POINT('Ctrl Pts',(-3.70949455661916,2.2338521323121,5.2));
#19143=CARTESIAN_POINT('Ctrl Pts',(-3.71393782222619,2.23758261370384,5.2));
#19144=CARTESIAN_POINT('Ctrl Pts',(-3.71822343533123,2.24150219834368,5.2));
#19145=CARTESIAN_POINT('Ctrl Pts',(-3.72133392659836,2.24434702672511,5.2));
#19146=CARTESIAN_POINT('Ctrl Pts',(-3.72435518261367,2.24728605527231,5.2));
#19147=CARTESIAN_POINT('Ctrl Pts',(-3.72727779974184,2.25030906336475,5.2));
#19148=CARTESIAN_POINT('Ctrl Pts',(-3.73622279642463,2.25956131782473,5.2));
#19149=CARTESIAN_POINT('Ctrl Pts',(-3.74426351405243,2.26961342426582,5.2));
#19150=CARTESIAN_POINT('Ctrl Pts',(-3.75126091239845,2.28033434366482,5.2));
#19151=CARTESIAN_POINT('Ctrl Pts',(-3.75579176664188,2.28727619844431,5.2));
#19152=CARTESIAN_POINT('Ctrl Pts',(-3.75988435832116,2.29449904020269,5.2));
#19153=CARTESIAN_POINT('Ctrl Pts',(-3.76348920729151,2.30196994667654,5.2));
#19154=CARTESIAN_POINT('Ctrl Pts',(-3.76515597383801,2.30542425421759,5.2));
#19155=CARTESIAN_POINT('Ctrl Pts',(-3.76671433719502,2.30892350560647,5.2));
#19156=CARTESIAN_POINT('Ctrl Pts',(-3.76815916520543,2.31246074610162,5.2));
#19157=CARTESIAN_POINT('Ctrl Pts',(-3.77216128940432,2.32225878135629,5.2));
#19158=CARTESIAN_POINT('Ctrl Pts',(-3.77529844536059,2.33235630265294,5.2));
#19159=CARTESIAN_POINT('Ctrl Pts',(-3.77747651815115,2.34267992422407,5.2));
#19160=CARTESIAN_POINT('Ctrl Pts',(-3.77933030902448,2.35146651553144,5.2));
#19161=CARTESIAN_POINT('Ctrl Pts',(-3.78048860368035,2.36041737528633,5.2));
#19162=CARTESIAN_POINT('Ctrl Pts',(-3.78096403138949,2.36945420421056,5.2));
#19163=CARTESIAN_POINT('Ctrl Pts',(-3.781133173515,2.37266922180987,5.2));
#19164=CARTESIAN_POINT('Ctrl Pts',(-3.78121552286205,2.37589368165894,5.2));
#19165=CARTESIAN_POINT('Ctrl Pts',(-3.78121200959806,2.37911434872485,5.2));
#19166=CARTESIAN_POINT('Ctrl Pts',(-3.78119923720175,2.3908230151512,5.2));
#19167=CARTESIAN_POINT('Ctrl Pts',(-3.78005717470715,2.40251790081025,5.2));
#19168=CARTESIAN_POINT('Ctrl Pts',(-3.77783120806398,2.41402669258654,5.2));
#19169=CARTESIAN_POINT('Ctrl Pts',(-3.77668819949671,2.41993632633585,5.2));
#19170=CARTESIAN_POINT('Ctrl Pts',(-3.77525870411221,2.42579670928221,5.2));
#19171=CARTESIAN_POINT('Ctrl Pts',(-3.77354493887783,2.43158224657623,5.2));
#19172=CARTESIAN_POINT('Ctrl Pts',(-3.77185769889076,2.43727823671147,5.2));
#19173=CARTESIAN_POINT('Ctrl Pts',(-3.7698921652597,2.44290711736645,5.2));
#19174=CARTESIAN_POINT('Ctrl Pts',(-3.76766231085216,2.44841156899725,5.2));
#19175=CARTESIAN_POINT('Ctrl Pts',(-3.76420558690842,2.45694457890368,5.2));
#19176=CARTESIAN_POINT('Ctrl Pts',(-3.7601120066452,2.46519219654187,5.2));
#19177=CARTESIAN_POINT('Ctrl Pts',(-3.75539091261074,2.47305855746262,5.2));
#19178=CARTESIAN_POINT('Ctrl Pts',(-3.75297690030925,2.47708082261811,5.2));
#19179=CARTESIAN_POINT('Ctrl Pts',(-3.75039789825265,2.48100349927224,5.2));
#19180=CARTESIAN_POINT('Ctrl Pts',(-3.74766394598163,2.48480007876844,5.2));
#19181=CARTESIAN_POINT('Ctrl Pts',(-3.74222934299289,2.49234699262488,5.2));
#19182=CARTESIAN_POINT('Ctrl Pts',(-3.73617584476421,2.49941040205976,5.2));
#19183=CARTESIAN_POINT('Ctrl Pts',(-3.7295081017749,2.50587917960273,5.2));
#19184=CARTESIAN_POINT('Ctrl Pts',(-3.72872963243595,2.50663441941712,5.2));
#19185=CARTESIAN_POINT('Ctrl Pts',(-3.72794277607053,2.50738152833223,5.2));
#19186=CARTESIAN_POINT('Ctrl Pts',(-3.72714768981588,2.50812044061668,5.2));
#19187=CARTESIAN_POINT('Origin',(-3.6,2.4,4.7));
#19188=CARTESIAN_POINT('Origin',(3.6,2.4,4.3));
#19189=CARTESIAN_POINT('Ctrl Pts',(3.43648706727485,2.36807695453719,4.3));
#19190=CARTESIAN_POINT('Ctrl Pts',(3.43713128683271,2.3597806326638,4.3));
#19191=CARTESIAN_POINT('Ctrl Pts',(3.43844439010238,2.35157023568352,4.3));
#19192=CARTESIAN_POINT('Ctrl Pts',(3.44036779366958,2.34349709838219,4.3));
#19193=CARTESIAN_POINT('Ctrl Pts',(3.44142971905211,2.33903985936946,4.3));
#19194=CARTESIAN_POINT('Ctrl Pts',(3.44267796535882,2.33462439474099,4.3));
#19195=CARTESIAN_POINT('Ctrl Pts',(3.44410466805123,2.33025917432088,4.3));
#19196=CARTESIAN_POINT('Ctrl Pts',(3.44564438355751,2.32554817349018,4.3));
#19197=CARTESIAN_POINT('Ctrl Pts',(3.44738955334548,2.3209035962062,4.3));
#19198=CARTESIAN_POINT('Ctrl Pts',(3.4493265481332,2.31634215395336,4.3));
#19199=CARTESIAN_POINT('Ctrl Pts',(3.45254731917628,2.30875753823018,4.3));
#19200=CARTESIAN_POINT('Ctrl Pts',(3.45629959311852,2.30139710694769,4.3));
#19201=CARTESIAN_POINT('Ctrl Pts',(3.46054037353588,2.29430908064149,4.3));
#19202=CARTESIAN_POINT('Ctrl Pts',(3.46239353776121,2.29121170810954,4.3));
#19203=CARTESIAN_POINT('Ctrl Pts',(3.46433984867298,2.28816727138872,4.3));
#19204=CARTESIAN_POINT('Ctrl Pts',(3.46636983737831,2.28518826034786,4.3));
#19205=CARTESIAN_POINT('Ctrl Pts',(3.47324583140019,2.27509773026055,4.3));
#19206=CARTESIAN_POINT('Ctrl Pts',(3.48109365784268,2.26572974302294,4.3));
#19207=CARTESIAN_POINT('Ctrl Pts',(3.48977951837809,2.25723278343533,4.3));
#19208=CARTESIAN_POINT('Ctrl Pts',(3.49400932884437,2.25309496330239,4.3));
#19209=CARTESIAN_POINT('Ctrl Pts',(3.49843865454892,2.24916389122995,4.3));
#19210=CARTESIAN_POINT('Ctrl Pts',(3.50305598018317,2.24545876796073,4.3));
#19211=CARTESIAN_POINT('Ctrl Pts',(3.50696193979743,2.24232447269942,4.3));
#19212=CARTESIAN_POINT('Ctrl Pts',(3.51100698863209,2.23934939909905,4.3));
#19213=CARTESIAN_POINT('Ctrl Pts',(3.51515874429581,2.23656266075085,4.3));
#19214=CARTESIAN_POINT('Ctrl Pts',(3.52023402885856,2.23315603202204,4.3));
#19215=CARTESIAN_POINT('Ctrl Pts',(3.52547424287705,2.23002554171617,4.3));
#19216=CARTESIAN_POINT('Ctrl Pts',(3.53086412680946,2.22718930631114,4.3));
#19217=CARTESIAN_POINT('Ctrl Pts',(3.53843721702836,2.22320423596943,4.3));
#19218=CARTESIAN_POINT('Ctrl Pts',(3.54630546669305,2.21979946806346,4.3));
#19219=CARTESIAN_POINT('Ctrl Pts',(3.55440208317939,2.21695927394856,4.3));
#19220=CARTESIAN_POINT('Ctrl Pts',(3.56031223293849,2.21488606564082,4.3));
#19221=CARTESIAN_POINT('Ctrl Pts',(3.56634429400461,2.21311389140606,4.3));
#19222=CARTESIAN_POINT('Ctrl Pts',(3.57247452264395,2.21164027909917,4.3));
#19223=CARTESIAN_POINT('Ctrl Pts',(3.57600246534631,2.21079221614916,4.3));
#19224=CARTESIAN_POINT('Ctrl Pts',(3.57955843058062,2.21004433773534,4.3));
#19225=CARTESIAN_POINT('Ctrl Pts',(3.58312961367547,2.20939690917763,4.3));
#19226=CARTESIAN_POINT('Ctrl Pts',(3.59464652648698,2.20730897975681,4.3));
#19227=CARTESIAN_POINT('Ctrl Pts',(3.60634454881448,2.20625732608158,4.3));
#19228=CARTESIAN_POINT('Ctrl Pts',(3.61806689528204,2.2062086557371,4.3));
#19229=CARTESIAN_POINT('Ctrl Pts',(3.62473122101744,2.20618098593309,4.3));
#19230=CARTESIAN_POINT('Ctrl Pts',(3.63140379711974,2.20647808078856,4.3));
#19231=CARTESIAN_POINT('Ctrl Pts',(3.63805748358195,2.20709863975089,4.3));
#19232=CARTESIAN_POINT('Ctrl Pts',(3.64215439115276,2.20748073961769,4.3));
#19233=CARTESIAN_POINT('Ctrl Pts',(3.64624620849006,2.20798586737994,4.3));
#19234=CARTESIAN_POINT('Ctrl Pts',(3.65032009844121,2.20861337585159,4.3));
#19235=CARTESIAN_POINT('Ctrl Pts',(3.66357602962435,2.2106552103677,4.3));
#19236=CARTESIAN_POINT('Ctrl Pts',(3.67655558408475,2.21397441829708,4.3));
#19237=CARTESIAN_POINT('Ctrl Pts',(3.68904456814691,2.21853837010126,4.3));
#19238=CARTESIAN_POINT('Ctrl Pts',(3.69937753051516,2.22231442922732,4.3));
#19239=CARTESIAN_POINT('Ctrl Pts',(3.7093756794575,2.22694342372598,4.3));
#19240=CARTESIAN_POINT('Ctrl Pts',(3.71891590137671,2.23243384744346,4.3));
#19241=CARTESIAN_POINT('Ctrl Pts',(3.72007018093634,2.23309813847615,4.3));
#19242=CARTESIAN_POINT('Ctrl Pts',(3.72121774557788,2.23377506987061,4.3));
#19243=CARTESIAN_POINT('Ctrl Pts',(3.72235851517116,2.23446447326396,4.3));
#19244=CARTESIAN_POINT('Ctrl Pts',(3.78826275096636,2.31767678198967,4.3));
#19245=CARTESIAN_POINT('Ctrl Pts',(3.79091867322995,2.32572936860323,4.3));
#19246=CARTESIAN_POINT('Ctrl Pts',(3.79302804064853,2.33393960507108,4.3));
#19247=CARTESIAN_POINT('Ctrl Pts',(3.79460323981381,2.34225613442594,4.3));
#19248=CARTESIAN_POINT('Ctrl Pts',(3.79578956453863,2.34851953566168,4.3));
#19249=CARTESIAN_POINT('Ctrl Pts',(3.79667271897105,2.35484328449916,4.3));
#19250=CARTESIAN_POINT('Ctrl Pts',(3.79725488312451,2.36120517356094,4.3));
#19251=CARTESIAN_POINT('Ctrl Pts',(3.7976908683603,2.36596961961323,4.3));
#19252=CARTESIAN_POINT('Ctrl Pts',(3.79795758133253,2.37075408813906,4.3));
#19253=CARTESIAN_POINT('Ctrl Pts',(3.79805590956906,2.3755369878883,4.3));
#19254=CARTESIAN_POINT('Ctrl Pts',(3.79826159173226,2.3855418166282,4.3));
#19255=CARTESIAN_POINT('Ctrl Pts',(3.79773306912215,2.39555473221079,4.3));
#19256=CARTESIAN_POINT('Ctrl Pts',(3.79647804098653,2.40548740413607,4.3));
#19257=CARTESIAN_POINT('Ctrl Pts',(3.79582247707096,2.41067573507037,4.3));
#19258=CARTESIAN_POINT('Ctrl Pts',(3.79496739950913,2.41584508273998,4.3));
#19259=CARTESIAN_POINT('Ctrl Pts',(3.79391843118089,2.42095777287915,4.3));
#19260=CARTESIAN_POINT('Ctrl Pts',(3.79135148096571,2.43346913351755,4.3));
#19261=CARTESIAN_POINT('Ctrl Pts',(3.78762422716575,2.44567369959671,4.3));
#19262=CARTESIAN_POINT('Ctrl Pts',(3.78275033841106,2.45738291584384,4.3));
#19263=CARTESIAN_POINT('Ctrl Pts',(3.78051276867504,2.46275853872441,4.3));
#19264=CARTESIAN_POINT('Ctrl Pts',(3.77803290925375,2.46802940870032,4.3));
#19265=CARTESIAN_POINT('Ctrl Pts',(3.77530915968311,2.47317482247228,4.3));
#19266=CARTESIAN_POINT('Ctrl Pts',(3.7735285304889,2.4765385950002,4.3));
#19267=CARTESIAN_POINT('Ctrl Pts',(3.77164255910733,2.47985045045176,4.3));
#19268=CARTESIAN_POINT('Ctrl Pts',(3.76965384065618,2.48309856403818,4.3));
#19269=CARTESIAN_POINT('Ctrl Pts',(3.76538142018115,2.49007657894212,4.3));
#19270=CARTESIAN_POINT('Ctrl Pts',(3.76065254798511,2.4967339395313,4.3));
#19271=CARTESIAN_POINT('Ctrl Pts',(3.75546934621649,2.50301830246242,4.3));
#19272=CARTESIAN_POINT('Ctrl Pts',(3.7497639943478,2.5099357452696,4.3));
#19273=CARTESIAN_POINT('Ctrl Pts',(3.74350797317419,2.51640155748529,4.3));
#19274=CARTESIAN_POINT('Ctrl Pts',(3.73677354924283,2.52238273959095,4.3));
#19275=CARTESIAN_POINT('Ctrl Pts',(3.73252952287629,2.52615207380843,4.3));
#19276=CARTESIAN_POINT('Ctrl Pts',(3.72809532803267,2.52972869286917,4.3));
#19277=CARTESIAN_POINT('Ctrl Pts',(3.72348818609076,2.53310156466662,4.3));
#19278=CARTESIAN_POINT('Ctrl Pts',(3.72067461067475,2.53516137295782,4.3));
#19279=CARTESIAN_POINT('Ctrl Pts',(3.71779994290363,2.53714246961825,4.3));
#19280=CARTESIAN_POINT('Ctrl Pts',(3.71487521534485,2.53903869288715,4.3));
#19281=CARTESIAN_POINT('Ctrl Pts',(3.70626340571031,2.54462208945595,4.3));
#19282=CARTESIAN_POINT('Ctrl Pts',(3.69720115342902,2.54948407839451,4.3));
#19283=CARTESIAN_POINT('Ctrl Pts',(3.68779739443943,2.55357358531277,4.3));
#19284=CARTESIAN_POINT('Ctrl Pts',(3.67897143105616,2.55741182046492,4.3));
#19285=CARTESIAN_POINT('Ctrl Pts',(3.66984396791867,2.56056952878093,4.3));
#19286=CARTESIAN_POINT('Ctrl Pts',(3.66050457512214,2.56298263453418,4.3));
#19287=CARTESIAN_POINT('Ctrl Pts',(3.657017355811,2.56388365981129,4.3));
#19288=CARTESIAN_POINT('Ctrl Pts',(3.65350912975721,2.56467838913094,4.3));
#19289=CARTESIAN_POINT('Ctrl Pts',(3.64998789179307,2.5653638764114,4.3));
#19290=CARTESIAN_POINT('Ctrl Pts',(3.63890668202576,2.56752108033372,4.3));
#19291=CARTESIAN_POINT('Ctrl Pts',(3.62768560566387,2.56860271836266,4.3));
#19292=CARTESIAN_POINT('Ctrl Pts',(3.61647526972934,2.56851225659508,4.3));
#19293=CARTESIAN_POINT('Ctrl Pts',(3.61029339424358,2.56846237197194,4.3));
#19294=CARTESIAN_POINT('Ctrl Pts',(3.60411488972487,2.56805522437202,4.3));
#19295=CARTESIAN_POINT('Ctrl Pts',(3.59796731823988,2.56726810386747,4.3));
#19296=CARTESIAN_POINT('Ctrl Pts',(3.5968916538024,2.56713037833848,4.3));
#19297=CARTESIAN_POINT('Ctrl Pts',(3.59581694274575,2.56698100748364,4.3));
#19298=CARTESIAN_POINT('Ctrl Pts',(3.59474333802771,2.56682006235004,4.3));
#19299=CARTESIAN_POINT('Origin',(3.6,2.4,5.35459252805377));
#19300=CARTESIAN_POINT('Ctrl Pts',(3.39434265438876,2.4001499379742,5.17959252805377));
#19301=CARTESIAN_POINT('Ctrl Pts',(3.3942608381295,2.40997903394326,5.17905813053169));
#19302=CARTESIAN_POINT('Ctrl Pts',(3.39937061019979,2.4878631610827,5.17481913665734));
#19303=CARTESIAN_POINT('Ctrl Pts',(3.4989044460774,2.62084298387434,5.16687554643073));
#19304=CARTESIAN_POINT('Ctrl Pts',(3.73070050850364,2.60468899581803,5.15576175737391));
#19305=CARTESIAN_POINT('Ctrl Pts',(3.84286218134804,2.40121305191012,5.14464796831713));
#19306=CARTESIAN_POINT('Ctrl Pts',(3.73273070961532,2.19661070737624,5.1335341792603));
#19307=CARTESIAN_POINT('Ctrl Pts',(3.50110863285869,2.17818091869864,5.12242039020352));
#19308=CARTESIAN_POINT('Ctrl Pts',(3.39978420373419,2.31073763553012,5.11443983980133));
#19309=CARTESIAN_POINT('Ctrl Pts',(3.39427096205728,2.38932589106744,5.11016388575141));
#19310=CARTESIAN_POINT('Ctrl Pts',(3.39436118415265,2.39983962587988,5.10959252805377));
#19311=CARTESIAN_POINT('Ctrl Pts',(3.39473291096846,2.39977036782444,5.18540747194623));
#19312=CARTESIAN_POINT('Ctrl Pts',(3.39508769603641,2.44679019469361,5.18286245525962));
#19313=CARTESIAN_POINT('Ctrl Pts',(3.43434460318779,2.56295297845058,5.17661284222074));
#19314=CARTESIAN_POINT('Ctrl Pts',(3.62721323264599,2.64128528195604,5.16665863282959));
#19315=CARTESIAN_POINT('Ctrl Pts',(3.81747536314189,2.50809334538988,5.15554484377278));
#19316=CARTESIAN_POINT('Ctrl Pts',(3.80876232811303,2.27586209318291,5.14443105471598));
#19317=CARTESIAN_POINT('Ctrl Pts',(3.60892557137656,2.15730570431671,5.13331726565918));
#19318=CARTESIAN_POINT('Ctrl Pts',(3.42787436374214,2.24745398081386,5.12364273806926));
#19319=CARTESIAN_POINT('Ctrl Pts',(3.39500774851697,2.35820797614884,5.11767280683161));
#19320=CARTESIAN_POINT('Ctrl Pts',(3.39479089114249,2.40011619889285,5.11540747194623));
#19321=CARTESIAN_POINT('Ctrl Pts',(3.72690708798524,2.50793586530485,5.2));
#19322=CARTESIAN_POINT('Ctrl Pts',(3.76279833110066,2.46573623930395,5.19629540364773));
#19323=CARTESIAN_POINT('Ctrl Pts',(3.78852074717293,2.34341311981147,5.1888862109432));
#19324=CARTESIAN_POINT('Ctrl Pts',(3.65451258117961,2.21065853310285,5.17777242188639));
#19325=CARTESIAN_POINT('Ctrl Pts',(3.47057722493071,2.25164322990955,5.16665863282959));
#19326=CARTESIAN_POINT('Ctrl Pts',(3.405121385579,2.4282098150683,5.15554484377278));
#19327=CARTESIAN_POINT('Ctrl Pts',(3.5180312968317,2.57906042639477,5.14443105471598));
#19328=CARTESIAN_POINT('Ctrl Pts',(3.70597252569269,2.56596270448124,5.13331726565917));
#19329=CARTESIAN_POINT('Ctrl Pts',(3.79691368493775,2.4009835476249,5.12220347660237));
#19330=CARTESIAN_POINT('Ctrl Pts',(3.70761862135009,2.23509110037173,5.11108968754557));
#19331=CARTESIAN_POINT('Ctrl Pts',(3.51981846080671,2.22014814967852,5.09997589848877));
#19332=CARTESIAN_POINT('Ctrl Pts',(3.40540964822557,2.3698223862213,5.08886210943195));
#19333=CARTESIAN_POINT('Ctrl Pts',(3.46911145369901,2.54712015828428,5.07774832037516));
#19334=CARTESIAN_POINT('Ctrl Pts',(3.65261709875363,2.58975637037653,5.06663453131834));
#19335=CARTESIAN_POINT('Ctrl Pts',(3.78796168225801,2.4587068294695,5.05552074226155));
#19336=CARTESIAN_POINT('Ctrl Pts',(3.75126282351006,2.27392205963726,5.04440695320474));
#19337=CARTESIAN_POINT('Ctrl Pts',(3.576111378403,2.20453795937386,5.03329316414794));
#19338=CARTESIAN_POINT('Ctrl Pts',(3.42282546383512,2.31406243118482,5.02217937509113));
#19339=CARTESIAN_POINT('Ctrl Pts',(3.43170940937961,2.50224655949829,5.01106558603433));
#19340=CARTESIAN_POINT('Ctrl Pts',(3.59463164213028,2.59684323978071,4.99995179697753));
#19341=CARTESIAN_POINT('Ctrl Pts',(3.762467593188,2.51126707661319,4.98883800792072));
#19342=CARTESIAN_POINT('Ctrl Pts',(3.78159511395878,2.32384689323348,4.97772421886391));
#19343=CARTESIAN_POINT('Ctrl Pts',(3.63450656736167,2.20613051367693,4.96661042980712));
#19344=CARTESIAN_POINT('Ctrl Pts',(3.45583376839362,2.26586507280002,4.95549664075031));
#19345=CARTESIAN_POINT('Ctrl Pts',(3.40911795613805,2.44837485237297,4.94438285169351));
#19346=CARTESIAN_POINT('Ctrl Pts',(3.53711864339547,2.58660658076597,4.9332690626367));
#19347=CARTESIAN_POINT('Ctrl Pts',(3.72267534946784,2.5540351896186,4.9221552735799));
#19348=CARTESIAN_POINT('Ctrl Pts',(3.79594591694334,2.38047364248689,4.91104148452309));
#19349=CARTESIAN_POINT('Ctrl Pts',(3.6898649644607,2.22478479185514,4.89992769546629));
#19350=CARTESIAN_POINT('Ctrl Pts',(3.5015295908702,2.22947240830188,4.88881390640948));
#19351=CARTESIAN_POINT('Ctrl Pts',(3.40332529948609,2.39024586335038,4.87770011735268));
#19352=CARTESIAN_POINT('Ctrl Pts',(3.48513959192542,2.5599473902907,4.86658632829587));
#19353=CARTESIAN_POINT('Ctrl Pts',(3.67208691848091,2.58324725697266,4.85547253923907));
#19354=CARTESIAN_POINT('Ctrl Pts',(3.79305227102963,2.43881883118157,4.84435875018227));
#19355=CARTESIAN_POINT('Ctrl Pts',(3.73731469054324,2.25885908897487,4.83324496112546));
#19356=CARTESIAN_POINT('Ctrl Pts',(3.55589141654812,2.20808722327608,4.82213117206866));
#19357=CARTESIAN_POINT('Ctrl Pts',(3.41484122921187,2.33297529855171,4.81101738301186));
#19358=CARTESIAN_POINT('Ctrl Pts',(3.44326896462127,2.51921184317472,4.79990359395504));
#19359=CARTESIAN_POINT('Ctrl Pts',(3.61515439416365,2.59633243578568,4.78878980489825));
#19360=CARTESIAN_POINT('Ctrl Pts',(3.77316883486553,2.49374772336074,4.77767601584144));
#19361=CARTESIAN_POINT('Ctrl Pts',(3.77267987714682,2.30535465657222,4.76656222678464));
#19362=CARTESIAN_POINT('Ctrl Pts',(3.61413506955264,2.20359154597435,4.75544843772783));
#19363=CARTESIAN_POINT('Ctrl Pts',(3.44265227249432,2.28160332076952,4.74433464867103));
#19364=CARTESIAN_POINT('Ctrl Pts',(3.41519163486656,2.46798491877402,4.73322085961423));
#19365=CARTESIAN_POINT('Ctrl Pts',(3.55688818971484,2.59213914962324,4.72210707055742));
#19366=CARTESIAN_POINT('Ctrl Pts',(3.73804547343831,2.54042623781615,4.71099328150061));
#19367=CARTESIAN_POINT('Ctrl Pts',(3.79284816978155,2.36017959799409,4.69987949244381));
#19368=CARTESIAN_POINT('Ctrl Pts',(3.67113474927674,2.2163810237221,4.68876570338701));
#19369=CARTESIAN_POINT('Ctrl Pts',(3.48431088603601,2.24065098081811,4.67765191433021));
#19370=CARTESIAN_POINT('Ctrl Pts',(3.4033785808103,2.41077490231207,4.6665381252734));
#19371=CARTESIAN_POINT('Ctrl Pts',(3.50241609040748,2.57103643352413,4.65542433621659));
#19372=CARTESIAN_POINT('Ctrl Pts',(3.69077325913151,2.57474637744638,4.64431054715979));
#19373=CARTESIAN_POINT('Ctrl Pts',(3.79604463433366,2.41850898033344,4.63319675810299));
#19374=CARTESIAN_POINT('Ctrl Pts',(3.72187413243292,2.24533010361481,4.62208296904618));
#19375=CARTESIAN_POINT('Ctrl Pts',(3.5361508549695,2.21372233713422,4.61096917998938));
#19376=CARTESIAN_POINT('Ctrl Pts',(3.40886942405137,2.35261662800557,4.59985539093258));
#19377=CARTESIAN_POINT('Ctrl Pts',(3.45653197686655,2.53488145663037,4.58874160187577));
#19378=CARTESIAN_POINT('Ctrl Pts',(3.63551243829507,2.5936877583357,4.57762781281897));
#19379=CARTESIAN_POINT('Ctrl Pts',(3.78198796221116,2.47520945827968,4.56651402376216));
#19380=CARTESIAN_POINT('Ctrl Pts',(3.76188784043654,2.28789108810318,4.55540023470536));
#19381=CARTESIAN_POINT('Ctrl Pts',(3.5936099423673,2.20318727643507,4.54428644564855));
#19382=CARTESIAN_POINT('Ctrl Pts',(3.43118093653762,2.29862838255851,4.53317265659175));
#19383=CARTESIAN_POINT('Ctrl Pts',(3.42327393399308,2.4868560799498,4.52205886753494));
#19384=CARTESIAN_POINT('Ctrl Pts',(3.57712630395541,2.59558342196495,4.51094507847815));
#19385=CARTESIAN_POINT('Ctrl Pts',(3.75191522715083,2.52529104055601,4.49983128942133));
#19386=CARTESIAN_POINT('Ctrl Pts',(3.78765442042343,2.34031834729253,4.48871750036454));
#19387=CARTESIAN_POINT('Ctrl Pts',(3.65163139388737,2.20997295066536,4.47760371130772));
#19388=CARTESIAN_POINT('Ctrl Pts',(3.4683495682865,2.25356146118509,4.46648992225093));
#19389=CARTESIAN_POINT('Ctrl Pts',(3.40556887324678,2.431186839349,4.45537613319411));
#19390=CARTESIAN_POINT('Ctrl Pts',(3.52075319873735,2.58026652505992,4.44426234413732));
#19391=CARTESIAN_POINT('Ctrl Pts',(3.70847300970163,2.56434626551467,4.43314855508051));
#19392=CARTESIAN_POINT('Ctrl Pts',(3.79690626562936,2.39799790621595,4.4220347660237));
#19393=CARTESIAN_POINT('Ctrl Pts',(3.7051089416811,2.23348228455085,4.4109209769669));
#19394=CARTESIAN_POINT('Ctrl Pts',(3.51710429525804,2.22138181878176,4.3998071879101));
#19395=CARTESIAN_POINT('Ctrl Pts',(3.40497485954275,2.37277339597561,4.38869339885329));
#19396=CARTESIAN_POINT('Ctrl Pts',(3.47135448294965,2.54908419847293,4.37757960979649));
#19397=CARTESIAN_POINT('Ctrl Pts',(3.65548413352142,2.58893973580292,4.36646582073968));
#19398=CARTESIAN_POINT('Ctrl Pts',(3.78882987626983,2.45585019704184,4.35535203168288));
#19399=CARTESIAN_POINT('Ctrl Pts',(3.7493347906086,2.27165314263956,4.34423824262608));
#19400=CARTESIAN_POINT('Ctrl Pts',(3.57315728718835,2.20490778239848,4.33312445356927));
#19401=CARTESIAN_POINT('Ctrl Pts',(3.4215383866044,2.31678389237007,4.32201066451247));
#19402=CARTESIAN_POINT('Ctrl Pts',(3.43328916816391,2.50472575846861,4.31089687545566));
#19403=CARTESIAN_POINT('Ctrl Pts',(3.59758812791782,2.59701775419156,4.29978308639886));
#19404=CARTESIAN_POINT('Ctrl Pts',(3.76418967154123,2.50855366821667,4.28866929734205));
#19405=CARTESIAN_POINT('Ctrl Pts',(3.77483953817107,2.38400982617006,4.28126010463752));
#19406=CARTESIAN_POINT('Ctrl Pts',(3.75264423560529,2.33325198627316,4.27755550828525));
#19407=CARTESIAN_POINT('Ctrl Pts',(3.73677806246588,2.51633123698097,5.20748149723825));
#19408=CARTESIAN_POINT('Ctrl Pts',(3.77546096639785,2.47084927712496,5.20377690088598));
#19409=CARTESIAN_POINT('Ctrl Pts',(3.80318410060701,2.33901172932062,5.19636770818144));
#19410=CARTESIAN_POINT('Ctrl Pts',(3.658752630386,2.19593134317562,5.18525391912464));
#19411=CARTESIAN_POINT('Ctrl Pts',(3.46051057751011,2.24010387529317,5.17414013006783));
#19412=CARTESIAN_POINT('Ctrl Pts',(3.3899635101576,2.43040400586618,5.16302634101103));
#19413=CARTESIAN_POINT('Ctrl Pts',(3.5116556799136,2.59298794555462,5.15191255195423));
#19414=CARTESIAN_POINT('Ctrl Pts',(3.71421518662967,2.57887146826017,5.14079876289742));
#19415=CARTESIAN_POINT('Ctrl Pts',(3.81222985040785,2.40106004905331,5.12968497384063));
#19416=CARTESIAN_POINT('Ctrl Pts',(3.7159893174385,2.22226430270657,5.11857118478381));
#19417=CARTESIAN_POINT('Ctrl Pts',(3.5135818514907,2.20615907268523,5.10745739572702));
#19418=CARTESIAN_POINT('Ctrl Pts',(3.3902741941935,2.36747513785065,5.0963436066702));
#19419=CARTESIAN_POINT('Ctrl Pts',(3.45893079696141,2.55856332785872,5.08522981761341));
#19420=CARTESIAN_POINT('Ctrl Pts',(3.65670971522832,2.60451583195793,5.07411602855659));
#19421=CARTESIAN_POINT('Ctrl Pts',(3.80258155100106,2.46327311197376,5.0630022394998));
#19422=CARTESIAN_POINT('Ctrl Pts',(3.76302821419424,2.26411557718108,5.05188845044299));
#19423=CARTESIAN_POINT('Ctrl Pts',(3.57425329484041,2.18933470441319,5.04077466138619));
#19424=CARTESIAN_POINT('Ctrl Pts',(3.40904463131529,2.30737811148155,5.02966087232938));
#19425=CARTESIAN_POINT('Ctrl Pts',(3.41861958002714,2.51019941063974,5.01854708327258));
#19426=CARTESIAN_POINT('Ctrl Pts',(3.59421408528317,2.61215392594813,5.00743329421578));
#19427=CARTESIAN_POINT('Ctrl Pts',(3.77510450332242,2.51992155361066,4.99631950515897));
#19428=CARTESIAN_POINT('Ctrl Pts',(3.79571978393707,2.31792361987304,4.98520571610216));
#19429=CARTESIAN_POINT('Ctrl Pts',(3.63719052655772,2.19105112936158,4.97409192704537));
#19430=CARTESIAN_POINT('Ctrl Pts',(3.44462035852227,2.25543190894468,4.96297813798855));
#19431=CARTESIAN_POINT('Ctrl Pts',(3.3942709384207,2.4521375022049,4.95186434893175));
#19432=CARTESIAN_POINT('Ctrl Pts',(3.53222766152672,2.6011210482075,4.94075055987495));
#19433=CARTESIAN_POINT('Ctrl Pts',(3.73221717461903,2.56601621802281,4.92963677081814));
#19434=CARTESIAN_POINT('Ctrl Pts',(3.81118680834224,2.37895486067752,4.91852298176134));
#19435=CARTESIAN_POINT('Ctrl Pts',(3.69685476136628,2.21115635804835,4.90740919270453));
#19436=CARTESIAN_POINT('Ctrl Pts',(3.49387045290517,2.21620858251703,4.89629540364774));
#19437=CARTESIAN_POINT('Ctrl Pts',(3.38802772249033,2.38948717575083,4.88518161459092));
#19438=CARTESIAN_POINT('Ctrl Pts',(3.47620562160949,2.57238827624017,4.87406782553412));
#19439=CARTESIAN_POINT('Ctrl Pts',(3.67769391919309,2.59750043247249,4.86295403647732));
#19440=CARTESIAN_POINT('Ctrl Pts',(3.80806809143035,2.44183820305468,4.85184024742052));
#19441=CARTESIAN_POINT('Ctrl Pts',(3.74799517992873,2.24788099190383,4.84072645836371));
#19442=CARTESIAN_POINT('Ctrl Pts',(3.55246060185887,2.19316003401009,4.82961266930691));
#19443=CARTESIAN_POINT('Ctrl Pts',(3.40043937404102,2.32776204271177,4.8184988802501));
#19444=CARTESIAN_POINT('Ctrl Pts',(3.43107825033486,2.52848427295347,4.8073850911933));
#19445=CARTESIAN_POINT('Ctrl Pts',(3.61633311980013,2.61160339105013,4.79627130213649));
#19446=CARTESIAN_POINT('Ctrl Pts',(3.78663809948217,2.50103952557292,4.78515751307969));
#19447=CARTESIAN_POINT('Ctrl Pts',(3.78611111008816,2.29799303647267,4.77404372402288));
#19448=CARTESIAN_POINT('Ctrl Pts',(3.61523451098693,2.18831467792663,4.76292993496608));
#19449=CARTESIAN_POINT('Ctrl Pts',(3.43041359120824,2.27239429534918,4.75181614590927));
#19450=CARTESIAN_POINT('Ctrl Pts',(3.40081703463734,2.47327286138574,4.74070235685248));
#19451=CARTESIAN_POINT('Ctrl Pts',(3.55353490515134,2.60708394642517,4.72958856779567));
#19452=CARTESIAN_POINT('Ctrl Pts',(3.74878280393034,2.55134874680995,4.71847477873887));
#19453=CARTESIAN_POINT('Ctrl Pts',(3.80784811496013,2.35708232282806,4.70736098968206));
#19454=CARTESIAN_POINT('Ctrl Pts',(3.67666768920898,2.2020989354812,4.69624720062525));
#19455=CARTESIAN_POINT('Ctrl Pts',(3.47531245805411,2.22825663683913,4.68513341156846));
#19456=CARTESIAN_POINT('Ctrl Pts',(3.38808514809522,2.41161298620039,4.67401962251165));
#19457=CARTESIAN_POINT('Ctrl Pts',(3.49482590536264,2.58433983759226,4.66290583345484));
#19458=CARTESIAN_POINT('Ctrl Pts',(3.69783370420702,2.58833834507989,4.65179204439804));
#19459=CARTESIAN_POINT('Ctrl Pts',(3.811293204081,2.419948629414,4.64067825534124));
#19460=CARTESIAN_POINT('Ctrl Pts',(3.73135363803182,2.23329970701222,4.62956446628443));
#19461=CARTESIAN_POINT('Ctrl Pts',(3.53118459744037,2.19923345329287,4.61845067722763));
#19462=CARTESIAN_POINT('Ctrl Pts',(3.39400307523184,2.34893109662045,4.60733688817082));
#19463=CARTESIAN_POINT('Ctrl Pts',(3.44537287442694,2.54537268637529,4.59622309911402));
#19464=CARTESIAN_POINT('Ctrl Pts',(3.6382746352513,2.60875300764603,4.58510931005721));
#19465=CARTESIAN_POINT('Ctrl Pts',(3.79614318836354,2.48105933361106,4.57399552100041));
#19466=CARTESIAN_POINT('Ctrl Pts',(3.77447965675701,2.27917113222085,4.56288173194361));
#19467=CARTESIAN_POINT('Ctrl Pts',(3.59311291657604,2.18787896385287,4.5517679428868));
#19468=CARTESIAN_POINT('Ctrl Pts',(3.4180500019796,2.29074358538356,4.54065415383));
#19469=CARTESIAN_POINT('Ctrl Pts',(3.40952798398103,2.4936118424709,4.5295403647732));
#19470=CARTESIAN_POINT('Ctrl Pts',(3.57534716243134,2.61079611810118,4.51842657571639));
#19471=CARTESIAN_POINT('Ctrl Pts',(3.76373136251596,2.53503631706984,4.50731278665959));
#19472=CARTESIAN_POINT('Ctrl Pts',(3.80225038999918,2.33567624195239,4.49619899760278));
#19473=CARTESIAN_POINT('Ctrl Pts',(3.65564734114102,2.19519243537347,4.48508520854597));
#19474=CARTESIAN_POINT('Ctrl Pts',(3.45810965125396,2.24217130873125,4.47397141948918));
#19475=CARTESIAN_POINT('Ctrl Pts',(3.39044580391398,2.4336125864072,4.46285763043236));
#19476=CARTESIAN_POINT('Ctrl Pts',(3.51458929437743,2.59428785591567,4.45174384137557));
#19477=CARTESIAN_POINT('Ctrl Pts',(3.71691016106647,2.57712930087258,4.44063005231875));
#19478=CARTESIAN_POINT('Ctrl Pts',(3.8122218540174,2.39784218113421,4.42951626326196));
#19479=CARTESIAN_POINT('Ctrl Pts',(3.71328443209297,2.22053035140142,4.41840247420515));
#19480=CARTESIAN_POINT('Ctrl Pts',(3.5106565751263,2.2074886979437,4.40728868514835));
#19481=CARTESIAN_POINT('Ctrl Pts',(3.38980558716325,2.3706556804265,4.39617489609155));
#19482=CARTESIAN_POINT('Ctrl Pts',(3.46134829152241,2.56068013327812,4.38506110703473));
#19483=CARTESIAN_POINT('Ctrl Pts',(3.65979975114976,2.60363567863874,4.37394731797794));
#19484=CARTESIAN_POINT('Ctrl Pts',(3.80351727410895,2.46019428749802,4.36283352892113));
#19485=CARTESIAN_POINT('Ctrl Pts',(3.76095021674888,2.26167018129524,4.35171973986433));
#19486=CARTESIAN_POINT('Ctrl Pts',(3.57106943112482,2.18973329268408,4.34060595080752));
#19487=CARTESIAN_POINT('Ctrl Pts',(3.40765744378577,2.31031125094527,4.32949216175072));
#19488=CARTESIAN_POINT('Ctrl Pts',(3.42032221420706,2.51287144446394,4.31837837269392));
#19489=CARTESIAN_POINT('Ctrl Pts',(3.5974005298242,2.61234201428399,4.30726458363711));
#19490=CARTESIAN_POINT('Ctrl Pts',(3.77696052684568,2.51699709329055,4.29615079458031));
#19491=CARTESIAN_POINT('Ctrl Pts',(3.78843875194939,2.38276609266138,4.28874160187577));
#19492=CARTESIAN_POINT('Ctrl Pts',(3.76451707405898,2.328060251512,4.2850370055235));
#19493=CARTESIAN_POINT('Ctrl Pts',(3.74664903694653,2.52472660865709,5.2149629944765));
#19494=CARTESIAN_POINT('Ctrl Pts',(3.78812360169505,2.47596231494597,5.21125839812423));
#19495=CARTESIAN_POINT('Ctrl Pts',(3.81784745404107,2.33461033882977,5.20384920541969));
#19496=CARTESIAN_POINT('Ctrl Pts',(3.66299267959241,2.1812041532484,5.19273541636289));
#19497=CARTESIAN_POINT('Ctrl Pts',(3.4504439300895,2.22856452067679,5.18162162730609));
#19498=CARTESIAN_POINT('Ctrl Pts',(3.3748056347362,2.43259819666406,5.17050783824928));
#19499=CARTESIAN_POINT('Ctrl Pts',(3.5052800629955,2.60691546471448,5.15939404919248));
#19500=CARTESIAN_POINT('Ctrl Pts',(3.72245784756665,2.5917802320391,5.14828026013567));
#19501=CARTESIAN_POINT('Ctrl Pts',(3.82754601587795,2.40113655048171,5.13716647107887));
#19502=CARTESIAN_POINT('Ctrl Pts',(3.72436001352691,2.2094375050414,5.12605268202206));
#19503=CARTESIAN_POINT('Ctrl Pts',(3.5073452421747,2.19216999569193,5.11493889296526));
#19504=CARTESIAN_POINT('Ctrl Pts',(3.37513874016143,2.36512788948001,5.10382510390846));
#19505=CARTESIAN_POINT('Ctrl Pts',(3.44875014022381,2.57000649743315,5.09271131485165));
#19506=CARTESIAN_POINT('Ctrl Pts',(3.660802331703,2.61927529353934,5.08159752579485));
#19507=CARTESIAN_POINT('Ctrl Pts',(3.81720141974412,2.46783939447801,5.07048373673805));
#19508=CARTESIAN_POINT('Ctrl Pts',(3.77479360487843,2.25430909472489,5.05936994768124));
#19509=CARTESIAN_POINT('Ctrl Pts',(3.57239521127782,2.17413144945252,5.04825615862444));
#19510=CARTESIAN_POINT('Ctrl Pts',(3.39526379879546,2.30069379177829,5.03714236956763));
#19511=CARTESIAN_POINT('Ctrl Pts',(3.40552975067466,2.51815226178119,5.02602858051083));
#19512=CARTESIAN_POINT('Ctrl Pts',(3.59379652843607,2.62746461211554,5.01491479145402));
#19513=CARTESIAN_POINT('Ctrl Pts',(3.78774141345684,2.52857603060814,5.00380100239722));
#19514=CARTESIAN_POINT('Ctrl Pts',(3.80984445391536,2.3120003465126,4.99268721334041));
#19515=CARTESIAN_POINT('Ctrl Pts',(3.63987448575377,2.17597174504624,4.98157342428361));
#19516=CARTESIAN_POINT('Ctrl Pts',(3.43340694865093,2.24499874508934,4.9704596352268));
#19517=CARTESIAN_POINT('Ctrl Pts',(3.37942392070334,2.45590015203683,4.95934584617001));
#19518=CARTESIAN_POINT('Ctrl Pts',(3.52733667965797,2.61563551564903,4.94823205711319));
#19519=CARTESIAN_POINT('Ctrl Pts',(3.74175899977021,2.57799724642702,4.9371182680564));
#19520=CARTESIAN_POINT('Ctrl Pts',(3.82642769974115,2.37743607886815,4.92600447899959));
#19521=CARTESIAN_POINT('Ctrl Pts',(3.70384455827186,2.19752792424157,4.91489068994279));
#19522=CARTESIAN_POINT('Ctrl Pts',(3.48621131494014,2.20294475673219,4.90377690088598));
#19523=CARTESIAN_POINT('Ctrl Pts',(3.37273014549458,2.38872848815129,4.89266311182918));
#19524=CARTESIAN_POINT('Ctrl Pts',(3.46727165129357,2.58482916218966,4.88154932277237));
#19525=CARTESIAN_POINT('Ctrl Pts',(3.68330091990526,2.61175360797231,4.87043553371557));
#19526=CARTESIAN_POINT('Ctrl Pts',(3.82308391183106,2.4448575749278,4.85932174465876));
#19527=CARTESIAN_POINT('Ctrl Pts',(3.75867566931422,2.2369028948328,4.84820795560196));
#19528=CARTESIAN_POINT('Ctrl Pts',(3.54902978716961,2.1782328447441,4.83709416654516));
#19529=CARTESIAN_POINT('Ctrl Pts',(3.38603751887018,2.32254878687183,4.82598037748835));
#19530=CARTESIAN_POINT('Ctrl Pts',(3.41888753604845,2.53775670273222,4.81486658843155));
#19531=CARTESIAN_POINT('Ctrl Pts',(3.61751184543661,2.62687434631457,4.80375279937474));
#19532=CARTESIAN_POINT('Ctrl Pts',(3.80010736409881,2.5083313277851,4.79263901031794));
#19533=CARTESIAN_POINT('Ctrl Pts',(3.79954234302951,2.29063141637312,4.78152522126113));
#19534=CARTESIAN_POINT('Ctrl Pts',(3.61633395242122,2.17303780987892,4.77041143220434));
#19535=CARTESIAN_POINT('Ctrl Pts',(3.41817490992216,2.26318526992884,4.75929764314752));
#19536=CARTESIAN_POINT('Ctrl Pts',(3.38644243440813,2.47856080399747,4.74818385409073));
#19537=CARTESIAN_POINT('Ctrl Pts',(3.55018162058784,2.62202874322709,4.73707006503392));
#19538=CARTESIAN_POINT('Ctrl Pts',(3.75952013442236,2.56227125580376,4.72595627597711));
#19539=CARTESIAN_POINT('Ctrl Pts',(3.82284806013872,2.35398504766203,4.71484248692031));
#19540=CARTESIAN_POINT('Ctrl Pts',(3.68220062914122,2.1878168472403,4.7037286978635));
#19541=CARTESIAN_POINT('Ctrl Pts',(3.46631403007222,2.21586229286015,4.6926149088067));
#19542=CARTESIAN_POINT('Ctrl Pts',(3.37279171538014,2.4124510700887,4.6815011197499));
#19543=CARTESIAN_POINT('Ctrl Pts',(3.48723572031781,2.59764324166039,4.67038733069309));
#19544=CARTESIAN_POINT('Ctrl Pts',(3.70489414928252,2.6019303127134,4.65927354163629));
#19545=CARTESIAN_POINT('Ctrl Pts',(3.82654177382834,2.42138827849455,4.64815975257948));
#19546=CARTESIAN_POINT('Ctrl Pts',(3.74083314363071,2.22126931040964,4.63704596352268));
#19547=CARTESIAN_POINT('Ctrl Pts',(3.52621833991124,2.18474456945152,4.62593217446588));
#19548=CARTESIAN_POINT('Ctrl Pts',(3.3791367264123,2.34524556523533,4.61481838540907));
#19549=CARTESIAN_POINT('Ctrl Pts',(3.43421377198734,2.55586391612019,4.60370459635226));
#19550=CARTESIAN_POINT('Ctrl Pts',(3.64103683220752,2.62381825695636,4.59259080729547));
#19551=CARTESIAN_POINT('Ctrl Pts',(3.81029841451592,2.48690920894243,4.58147701823866));
#19552=CARTESIAN_POINT('Ctrl Pts',(3.78707147307748,2.27045117633852,4.57036322918186));
#19553=CARTESIAN_POINT('Ctrl Pts',(3.59261589078479,2.17257065127066,4.55924944012505));
#19554=CARTESIAN_POINT('Ctrl Pts',(3.40491906742157,2.28285878820862,4.54813565106825));
#19555=CARTESIAN_POINT('Ctrl Pts',(3.39578203396899,2.500367604992,4.53702186201145));
#19556=CARTESIAN_POINT('Ctrl Pts',(3.57356802090726,2.62600881423741,4.52590807295463));
#19557=CARTESIAN_POINT('Ctrl Pts',(3.77554749788108,2.54478159358368,4.51479428389784));
#19558=CARTESIAN_POINT('Ctrl Pts',(3.81684635957493,2.33103413661225,4.50368049484102));
#19559=CARTESIAN_POINT('Ctrl Pts',(3.65966328839466,2.18041192008159,4.49256670578423));
#19560=CARTESIAN_POINT('Ctrl Pts',(3.44786973422143,2.23078115627741,4.48145291672742));
#19561=CARTESIAN_POINT('Ctrl Pts',(3.37532273458119,2.43603833346541,4.47033912767062));
#19562=CARTESIAN_POINT('Ctrl Pts',(3.50842539001751,2.60830918677142,4.45922533861381));
#19563=CARTESIAN_POINT('Ctrl Pts',(3.72534731243133,2.58991233623048,4.44811154955701));
#19564=CARTESIAN_POINT('Ctrl Pts',(3.82753744240543,2.39768645605247,4.4369977605002));
#19565=CARTESIAN_POINT('Ctrl Pts',(3.72145992250484,2.20757841825199,4.4258839714434));
#19566=CARTESIAN_POINT('Ctrl Pts',(3.50420885499455,2.19359557710565,4.41477018238659));
#19567=CARTESIAN_POINT('Ctrl Pts',(3.37463631478375,2.36853796487738,4.40365639332979));
#19568=CARTESIAN_POINT('Ctrl Pts',(3.45134210009517,2.57227606808331,4.39254260427299));
#19569=CARTESIAN_POINT('Ctrl Pts',(3.6641153687781,2.61833162147455,4.38142881521619));
#19570=CARTESIAN_POINT('Ctrl Pts',(3.81820467194806,2.46453837795421,4.37031502615938));
#19571=CARTESIAN_POINT('Ctrl Pts',(3.77256564288916,2.25168721995093,4.35920123710258));
#19572=CARTESIAN_POINT('Ctrl Pts',(3.56898157506129,2.17455880296967,4.34808744804577));
#19573=CARTESIAN_POINT('Ctrl Pts',(3.39377650096713,2.30383860952047,4.33697365898897));
#19574=CARTESIAN_POINT('Ctrl Pts',(3.40735526025023,2.52101713045927,4.32585986993216));
#19575=CARTESIAN_POINT('Ctrl Pts',(3.59721293173057,2.62766627437643,4.31474608087536));
#19576=CARTESIAN_POINT('Ctrl Pts',(3.78973138215013,2.52544051836443,4.30363229181856));
#19577=CARTESIAN_POINT('Ctrl Pts',(3.8020379657277,2.3815223591527,4.29622309911402));
#19578=CARTESIAN_POINT('Ctrl Pts',(3.77638991251267,2.32286851675083,4.29251850276175));
#19579=CARTESIAN_POINT('Ctrl Pts',(3.75652001142717,2.53312198033322,5.22244449171475));
#19580=CARTESIAN_POINT('Ctrl Pts',(3.80078623699225,2.48107535276698,5.21873989536248));
#19581=CARTESIAN_POINT('Ctrl Pts',(3.83251080747514,2.33020894833891,5.21133070265794));
#19582=CARTESIAN_POINT('Ctrl Pts',(3.6672327287988,2.16647696332117,5.20021691360114));
#19583=CARTESIAN_POINT('Ctrl Pts',(3.44037728266889,2.21702516606042,5.18910312454433));
#19584=CARTESIAN_POINT('Ctrl Pts',(3.3596477593148,2.43479238746194,5.17798933548753));
#19585=CARTESIAN_POINT('Ctrl Pts',(3.4989044460774,2.62084298387434,5.16687554643073));
#19586=CARTESIAN_POINT('Ctrl Pts',(3.73070050850364,2.60468899581803,5.15576175737391));
#19587=CARTESIAN_POINT('Ctrl Pts',(3.84286218134804,2.40121305191012,5.14464796831713));
#19588=CARTESIAN_POINT('Ctrl Pts',(3.73273070961532,2.19661070737624,5.1335341792603));
#19589=CARTESIAN_POINT('Ctrl Pts',(3.50110863285869,2.17818091869864,5.12242039020352));
#19590=CARTESIAN_POINT('Ctrl Pts',(3.36000328612935,2.36278064110937,5.1113066011467));
#19591=CARTESIAN_POINT('Ctrl Pts',(3.43856948348621,2.58144966700758,5.10019281208991));
#19592=CARTESIAN_POINT('Ctrl Pts',(3.66489494817768,2.63403475512075,5.08907902303309));
#19593=CARTESIAN_POINT('Ctrl Pts',(3.83182128848718,2.47240567698227,5.0779652339763));
#19594=CARTESIAN_POINT('Ctrl Pts',(3.78655899556261,2.24450261226871,5.06685144491949));
#19595=CARTESIAN_POINT('Ctrl Pts',(3.57053712771522,2.15892819449186,5.05573765586269));
#19596=CARTESIAN_POINT('Ctrl Pts',(3.38148296627563,2.29400947207503,5.04462386680588));
#19597=CARTESIAN_POINT('Ctrl Pts',(3.39243992132218,2.52610511292264,5.03351007774908));
#19598=CARTESIAN_POINT('Ctrl Pts',(3.59337897158896,2.64277529828296,5.02239628869227));
#19599=CARTESIAN_POINT('Ctrl Pts',(3.80037832359127,2.53723050760561,5.01128249963547));
#19600=CARTESIAN_POINT('Ctrl Pts',(3.82396912389365,2.30607707315216,5.00016871057866));
#19601=CARTESIAN_POINT('Ctrl Pts',(3.64255844494981,2.16089236073089,4.98905492152186));
#19602=CARTESIAN_POINT('Ctrl Pts',(3.42219353877959,2.234565581234,4.97794113246505));
#19603=CARTESIAN_POINT('Ctrl Pts',(3.36457690298599,2.45966280186876,4.96682734340826));
#19604=CARTESIAN_POINT('Ctrl Pts',(3.52244569778922,2.63014998309056,4.95571355435144));
#19605=CARTESIAN_POINT('Ctrl Pts',(3.7513008249214,2.58997827483123,4.94459976529465));
#19606=CARTESIAN_POINT('Ctrl Pts',(3.84166859114005,2.37591729705878,4.93348597623783));
#19607=CARTESIAN_POINT('Ctrl Pts',(3.71083435517744,2.18389949043478,4.92237218718104));
#19608=CARTESIAN_POINT('Ctrl Pts',(3.47855217697512,2.18968093094735,4.91125839812423));
#19609=CARTESIAN_POINT('Ctrl Pts',(3.35743256849882,2.38796980055174,4.90014460906743));
#19610=CARTESIAN_POINT('Ctrl Pts',(3.45833768097764,2.59727004813914,4.88903082001062));
#19611=CARTESIAN_POINT('Ctrl Pts',(3.68890792061744,2.62600678347214,4.87791703095382));
#19612=CARTESIAN_POINT('Ctrl Pts',(3.83809973223177,2.44787694680091,4.86680324189701));
#19613=CARTESIAN_POINT('Ctrl Pts',(3.76935615869971,2.22592479776177,4.85568945284022));
#19614=CARTESIAN_POINT('Ctrl Pts',(3.54559897248035,2.16330565547811,4.8445756637834));
#19615=CARTESIAN_POINT('Ctrl Pts',(3.37163566369933,2.31733553103189,4.83346187472661));
#19616=CARTESIAN_POINT('Ctrl Pts',(3.40669682176204,2.54702913251096,4.82234808566979));
#19617=CARTESIAN_POINT('Ctrl Pts',(3.61869057107309,2.64214530157901,4.811234296613));
#19618=CARTESIAN_POINT('Ctrl Pts',(3.81357662871545,2.51562312999728,4.80012050755618));
#19619=CARTESIAN_POINT('Ctrl Pts',(3.81297357597085,2.28326979627357,4.78900671849939));
#19620=CARTESIAN_POINT('Ctrl Pts',(3.61743339385551,2.1577609418312,4.77789292944258));
#19621=CARTESIAN_POINT('Ctrl Pts',(3.40593622863608,2.2539762445085,4.76677914038578));
#19622=CARTESIAN_POINT('Ctrl Pts',(3.37206783417891,2.48384874660919,4.75566535132897));
#19623=CARTESIAN_POINT('Ctrl Pts',(3.54682833602434,2.63697354002902,4.74455156227216));
#19624=CARTESIAN_POINT('Ctrl Pts',(3.77025746491439,2.57319376479756,4.73343777321537));
#19625=CARTESIAN_POINT('Ctrl Pts',(3.83784800531731,2.35088777249601,4.72232398415856));
#19626=CARTESIAN_POINT('Ctrl Pts',(3.68773356907346,2.1735347589994,4.71121019510175));
#19627=CARTESIAN_POINT('Ctrl Pts',(3.45731560209032,2.20346794888116,4.70009640604495));
#19628=CARTESIAN_POINT('Ctrl Pts',(3.35749828266505,2.41328915397702,4.68898261698814));
#19629=CARTESIAN_POINT('Ctrl Pts',(3.47964553527297,2.61094664572852,4.67786882793135));
#19630=CARTESIAN_POINT('Ctrl Pts',(3.71195459435803,2.61552228034691,4.66675503887453));
#19631=CARTESIAN_POINT('Ctrl Pts',(3.84179034357568,2.42282792757511,4.65564124981774));
#19632=CARTESIAN_POINT('Ctrl Pts',(3.75031264922961,2.20923891380705,4.64452746076093));
#19633=CARTESIAN_POINT('Ctrl Pts',(3.5212520823821,2.17025568561017,4.63341367170412));
#19634=CARTESIAN_POINT('Ctrl Pts',(3.36427037759277,2.34156003385021,4.62229988264733));
#19635=CARTESIAN_POINT('Ctrl Pts',(3.42305466954774,2.56635514586511,4.61118609359051));
#19636=CARTESIAN_POINT('Ctrl Pts',(3.64379902916374,2.63888350626668,4.60007230453372));
#19637=CARTESIAN_POINT('Ctrl Pts',(3.8244536406683,2.49275908427381,4.5889585154769));
#19638=CARTESIAN_POINT('Ctrl Pts',(3.79966328939795,2.26173122045618,4.57784472642011));
#19639=CARTESIAN_POINT('Ctrl Pts',(3.59211886499353,2.15726233868846,4.56673093736329));
#19640=CARTESIAN_POINT('Ctrl Pts',(3.39178813286355,2.27497399103367,4.55561714830651));
#19641=CARTESIAN_POINT('Ctrl Pts',(3.38203608395695,2.50712336751311,4.54450335924968));
#19642=CARTESIAN_POINT('Ctrl Pts',(3.57178887938318,2.64122151037363,4.5333895701929));
#19643=CARTESIAN_POINT('Ctrl Pts',(3.78736363324621,2.55452687009752,4.52227578113608));
#19644=CARTESIAN_POINT('Ctrl Pts',(3.83144232915068,2.3263920312721,4.51116199207928));
#19645=CARTESIAN_POINT('Ctrl Pts',(3.66367923564831,2.1656314047897,4.50004820302247));
#19646=CARTESIAN_POINT('Ctrl Pts',(3.43762981718889,2.21939100382357,4.48893441396567));
#19647=CARTESIAN_POINT('Ctrl Pts',(3.36019966524839,2.43846408052362,4.47782062490886));
#19648=CARTESIAN_POINT('Ctrl Pts',(3.5022614856576,2.62233051762717,4.46670683585207));
#19649=CARTESIAN_POINT('Ctrl Pts',(3.73378446379617,2.60269537158839,4.45559304679526));
#19650=CARTESIAN_POINT('Ctrl Pts',(3.84285303079348,2.39753073097072,4.44447925773845));
#19651=CARTESIAN_POINT('Ctrl Pts',(3.72963541291671,2.19462648510256,4.43336546868165));
#19652=CARTESIAN_POINT('Ctrl Pts',(3.49776113486282,2.17970245626759,4.42225167962485));
#19653=CARTESIAN_POINT('Ctrl Pts',(3.35946704240424,2.36642024932827,4.41113789056804));
#19654=CARTESIAN_POINT('Ctrl Pts',(3.44133590866794,2.5838720028885,4.40002410151124));
#19655=CARTESIAN_POINT('Ctrl Pts',(3.66843098640644,2.63302756431036,4.38891031245443));
#19656=CARTESIAN_POINT('Ctrl Pts',(3.83289206978718,2.4688824684104,4.37779652339763));
#19657=CARTESIAN_POINT('Ctrl Pts',(3.78418106902943,2.24170425860662,4.36668273434082));
#19658=CARTESIAN_POINT('Ctrl Pts',(3.56689371899776,2.15938431325527,4.35556894528402));
#19659=CARTESIAN_POINT('Ctrl Pts',(3.37989555814849,2.29736596809567,4.34445515622721));
#19660=CARTESIAN_POINT('Ctrl Pts',(3.39438830629339,2.5291628164546,4.33334136717041));
#19661=CARTESIAN_POINT('Ctrl Pts',(3.59702533363695,2.64299053446886,4.32222757811361));
#19662=CARTESIAN_POINT('Ctrl Pts',(3.80250223745458,2.5338839434383,4.3111137890568));
#19663=CARTESIAN_POINT('Ctrl Pts',(3.81563717950601,2.38027862564402,4.30370459635227));
#19664=CARTESIAN_POINT('Ctrl Pts',(3.78826275096636,2.31767678198967,4.3));
#19665=CARTESIAN_POINT('Ctrl Pts',(3.72690708798524,2.50793586530485,5.2));
#19666=CARTESIAN_POINT('Ctrl Pts',(3.7351188943469,2.50027512151453,5.2));
#19667=CARTESIAN_POINT('Ctrl Pts',(3.74243605781657,2.49177396851828,5.2));
#19668=CARTESIAN_POINT('Ctrl Pts',(3.74885415042291,2.48262661237479,5.2));
#19669=CARTESIAN_POINT('Ctrl Pts',(3.75362491760652,2.47582709900174,5.2));
#19670=CARTESIAN_POINT('Ctrl Pts',(3.75789857135109,2.46866923842676,5.2));
#19671=CARTESIAN_POINT('Ctrl Pts',(3.7616631109362,2.46121836915243,5.2));
#19672=CARTESIAN_POINT('Ctrl Pts',(3.76388040997986,2.45682983638691,5.2));
#19673=CARTESIAN_POINT('Ctrl Pts',(3.76592247954252,2.45233444011456,5.2));
#19674=CARTESIAN_POINT('Ctrl Pts',(3.76777440855395,2.44777396604178,5.2));
#19675=CARTESIAN_POINT('Ctrl Pts',(3.77233273486399,2.43654884411541,5.2));
#19676=CARTESIAN_POINT('Ctrl Pts',(3.77575805024602,2.42490557824884,5.2));
#19677=CARTESIAN_POINT('Ctrl Pts',(3.77802226640697,2.41304266545579,5.2));
#19678=CARTESIAN_POINT('Ctrl Pts',(3.7794611438358,2.4055039517268,5.2));
#19679=CARTESIAN_POINT('Ctrl Pts',(3.78043038990374,2.39787565429666,5.2));
#19680=CARTESIAN_POINT('Ctrl Pts',(3.78091323142362,2.39020359559663,5.2));
#19681=CARTESIAN_POINT('Ctrl Pts',(3.78113855699256,2.38662330906275,5.2));
#19682=CARTESIAN_POINT('Ctrl Pts',(3.78125741264451,2.38303694149785,5.2));
#19683=CARTESIAN_POINT('Ctrl Pts',(3.78126865224829,2.37945929304311,5.2));
#19684=CARTESIAN_POINT('Ctrl Pts',(3.7813036985799,2.36830378822358,5.2));
#19685=CARTESIAN_POINT('Ctrl Pts',(3.78029680360483,2.3572059009501,5.2));
#19686=CARTESIAN_POINT('Ctrl Pts',(3.77821424861763,2.34630678216484,5.2));
#19687=CARTESIAN_POINT('Ctrl Pts',(3.77705386628862,2.34023388376937,5.2));
#19688=CARTESIAN_POINT('Ctrl Pts',(3.77555898983988,2.33422245704814,5.2));
#19689=CARTESIAN_POINT('Ctrl Pts',(3.77374834890996,2.32828864283844,5.2));
#19690=CARTESIAN_POINT('Ctrl Pts',(3.7726157055599,2.32457675546527,5.2));
#19691=CARTESIAN_POINT('Ctrl Pts',(3.77135884755536,2.32089372066286,5.2));
#19692=CARTESIAN_POINT('Ctrl Pts',(3.76998347568685,2.31724835341447,5.2));
#19693=CARTESIAN_POINT('Ctrl Pts',(3.76560168937412,2.30563460684914,5.2));
#19694=CARTESIAN_POINT('Ctrl Pts',(3.76005258957863,2.29448378034876,5.2));
#19695=CARTESIAN_POINT('Ctrl Pts',(3.75350159415067,2.28391841534468,5.2));
#19696=CARTESIAN_POINT('Ctrl Pts',(3.74916061754095,2.27691734155978,5.2));
#19697=CARTESIAN_POINT('Ctrl Pts',(3.74437851970176,2.27017319623005,5.2));
#19698=CARTESIAN_POINT('Ctrl Pts',(3.73919188354146,2.26372385230471,5.2));
#19699=CARTESIAN_POINT('Ctrl Pts',(3.73648175856153,2.26035393632525,5.2));
#19700=CARTESIAN_POINT('Ctrl Pts',(3.73365978483958,2.25706319070089,5.2));
#19701=CARTESIAN_POINT('Ctrl Pts',(3.73073434111394,2.25386182215374,5.2));
#19702=CARTESIAN_POINT('Ctrl Pts',(3.72446791350779,2.24700435158764,5.2));
#19703=CARTESIAN_POINT('Ctrl Pts',(3.71775194552741,2.24058263588329,5.2));
#19704=CARTESIAN_POINT('Ctrl Pts',(3.71064052052299,2.23464742809312,5.2));
#19705=CARTESIAN_POINT('Ctrl Pts',(3.70611387191905,2.23086947922341,5.2));
#19706=CARTESIAN_POINT('Ctrl Pts',(3.70142674452504,2.22728872352275,5.2));
#19707=CARTESIAN_POINT('Ctrl Pts',(3.69659089091882,2.22391966825811,5.2));
#19708=CARTESIAN_POINT('Ctrl Pts',(3.69251851777989,2.22108251658222,5.2));
#19709=CARTESIAN_POINT('Ctrl Pts',(3.68834767342073,2.21840053637087,5.2));
#19710=CARTESIAN_POINT('Ctrl Pts',(3.68408917108174,2.21588334611703,5.2));
#19711=CARTESIAN_POINT('Ctrl Pts',(3.67536611602187,2.21072716973562,5.2));
#19712=CARTESIAN_POINT('Ctrl Pts',(3.66627202526677,2.20625880103906,5.2));
#19713=CARTESIAN_POINT('Ctrl Pts',(3.65686566645047,2.20255201748434,5.2));
#19714=CARTESIAN_POINT('Ctrl Pts',(3.65562635833217,2.2020636407339,5.2));
#19715=CARTESIAN_POINT('Ctrl Pts',(3.65438161447105,2.20158850411268,5.2));
#19716=CARTESIAN_POINT('Ctrl Pts',(3.65313162618094,2.20112654952031,5.2));
#19717=CARTESIAN_POINT('Ctrl Pts',(3.43326717741735,2.39986996798437,5.08714803633902));
#19718=CARTESIAN_POINT('Ctrl Pts',(3.43319402496042,2.39134538728232,5.08771939403666));
#19719=CARTESIAN_POINT('Ctrl Pts',(3.43379133263065,2.38283109195966,5.08829075173431));
#19720=CARTESIAN_POINT('Ctrl Pts',(3.43509475123467,2.374426308808,5.08886210943196));
#19721=CARTESIAN_POINT('Ctrl Pts',(3.44354591908595,2.31993097404037,5.09256670578422));
#19722=CARTESIAN_POINT('Ctrl Pts',(3.48168218994633,2.27003956185944,5.0962713021365));
#19723=CARTESIAN_POINT('Ctrl Pts',(3.53205035213375,2.24758434755118,5.09997589848876));
#19724=CARTESIAN_POINT('Ctrl Pts',(3.58241851432117,2.22512913324292,5.10368049484103));
#19725=CARTESIAN_POINT('Ctrl Pts',(3.64501856783563,2.23011011680733,5.1073850911933));
#19726=CARTESIAN_POINT('Ctrl Pts',(3.69120110519081,2.26024934979839,5.11108968754557));
#19727=CARTESIAN_POINT('Ctrl Pts',(3.73738364254598,2.29038858278945,5.11479428389783));
#19728=CARTESIAN_POINT('Ctrl Pts',(3.76714866374187,2.34568606520718,5.1184988802501));
#19729=CARTESIAN_POINT('Ctrl Pts',(3.76687431446563,2.40083133255876,5.12220347660237));
#19730=CARTESIAN_POINT('Ctrl Pts',(3.7665999651894,2.45597659991035,5.12590807295464));
#19731=CARTESIAN_POINT('Ctrl Pts',(3.73628624544104,2.51096965219579,5.12961266930691));
#19732=CARTESIAN_POINT('Ctrl Pts',(3.68980584742337,2.54064913199077,5.13331726565917));
#19733=CARTESIAN_POINT('Ctrl Pts',(3.6433254494057,2.57032861178575,5.13702186201144));
#19734=CARTESIAN_POINT('Ctrl Pts',(3.5806783731187,2.57469451909026,5.14072645836371));
#19735=CARTESIAN_POINT('Ctrl Pts',(3.53053651643308,2.5517357041881,5.14443105471598));
#19736=CARTESIAN_POINT('Ctrl Pts',(3.48039465974747,2.52877688928595,5.14813565106825));
#19737=CARTESIAN_POINT('Ctrl Pts',(3.44275802266323,2.47849335217712,5.15184024742051));
#19738=CARTESIAN_POINT('Ctrl Pts',(3.43484901067973,2.42392381942959,5.15554484377278));
#19739=CARTESIAN_POINT('Ctrl Pts',(3.43370811542309,2.41605202441919,5.15607924129486));
#19740=CARTESIAN_POINT('Ctrl Pts',(3.43318581643692,2.40809104297335,5.15661363881694));
#19741=CARTESIAN_POINT('Ctrl Pts',(3.43325215340634,2.40012157034435,5.15714803633902));
#19742=CARTESIAN_POINT('Ctrl Pts',(3.54698297828114,2.20148256743283,5.2));
#19743=CARTESIAN_POINT('Ctrl Pts',(3.48097120902544,2.21911198848201,5.19629540364773));
#19744=CARTESIAN_POINT('Ctrl Pts',(3.36906718698604,2.32515231990061,5.1888862109432));
#19745=CARTESIAN_POINT('Ctrl Pts',(3.41187706889408,2.55382793971174,5.17777242188639));
#19746=CARTESIAN_POINT('Ctrl Pts',(3.62721323264599,2.64128528195604,5.16665863282959));
#19747=CARTESIAN_POINT('Ctrl Pts',(3.81747536314189,2.50809334538988,5.15554484377278));
#19748=CARTESIAN_POINT('Ctrl Pts',(3.80876232811303,2.27586209318291,5.14443105471598));
#19749=CARTESIAN_POINT('Ctrl Pts',(3.60892557137656,2.15730570431671,5.13331726565918));
#19750=CARTESIAN_POINT('Ctrl Pts',(3.40093971248811,2.26086517215761,5.12220347660237));
#19751=CARTESIAN_POINT('Ctrl Pts',(3.37514571617861,2.4917888042929,5.11108968754557));
#19752=CARTESIAN_POINT('Ctrl Pts',(3.55516852834243,2.63869087044012,5.09997589848876));
#19753=CARTESIAN_POINT('Ctrl Pts',(3.77622353148193,2.56711958879047,5.08886210943196));
#19754=CARTESIAN_POINT('Ctrl Pts',(3.8359804180852,2.34258029751366,5.07774832037515));
#19755=CARTESIAN_POINT('Ctrl Pts',(3.6797411123384,2.17059868763558,5.06663453131835));
#19756=CARTESIAN_POINT('Ctrl Pts',(3.45051418153466,2.2085903127083,5.05552074226155));
#19757=CARTESIAN_POINT('Ctrl Pts',(3.3581131561336,2.4217815890047,5.04440695320474));
#19758=CARTESIAN_POINT('Ctrl Pts',(3.48711398178203,2.61503583311392,5.03329316414794));
#19759=CARTESIAN_POINT('Ctrl Pts',(3.71944062032543,2.61146538882495,5.02217937509113));
#19760=CARTESIAN_POINT('Ctrl Pts',(3.84244192441188,2.41433825182845,5.01106558603433));
#19761=CARTESIAN_POINT('Ctrl Pts',(3.74353337567863,2.20408716238119,4.99995179697753));
#19762=CARTESIAN_POINT('Ctrl Pts',(3.51324710536571,2.17315730898832,4.98883800792072));
#19763=CARTESIAN_POINT('Ctrl Pts',(3.36236674087989,2.34985914625667,4.97772421886392));
#19764=CARTESIAN_POINT('Ctrl Pts',(3.42899479464802,2.5724554740903,4.96661042980711));
#19765=CARTESIAN_POINT('Ctrl Pts',(3.652145851588,2.63720135146115,4.95549664075031));
#19766=CARTESIAN_POINT('Ctrl Pts',(3.82756721950384,2.48483414141864,4.9443828516935));
#19767=CARTESIAN_POINT('Ctrl Pts',(3.79469373046592,2.25481727983819,4.9332690626367));
#19768=CARTESIAN_POINT('Ctrl Pts',(3.58361486203243,2.15768780841241,4.9221552735799));
#19769=CARTESIAN_POINT('Ctrl Pts',(3.38753349616232,2.28234943400059,4.91104148452309));
#19770=CARTESIAN_POINT('Ctrl Pts',(3.38592513080807,2.51469795687288,4.89992769546629));
#19771=CARTESIAN_POINT('Ctrl Pts',(3.58026192098975,2.64206213906777,4.88881390640948));
#19772=CARTESIAN_POINT('Ctrl Pts',(3.79266519873933,2.54786410019675,4.87770011735268));
#19773=CARTESIAN_POINT('Ctrl Pts',(3.82871983510845,2.3183243735256,4.86658632829587));
#19774=CARTESIAN_POINT('Ctrl Pts',(3.65542461254465,2.16354327402962,4.85547253923907));
#19775=CARTESIAN_POINT('Ctrl Pts',(3.43139861356028,2.22519369741672,4.84435875018226));
#19776=CARTESIAN_POINT('Ctrl Pts',(3.36169537565425,2.44684631199623,4.83324496112547));
#19777=CARTESIAN_POINT('Ctrl Pts',(3.51011506296999,2.62561996593247,4.82213117206865));
#19778=CARTESIAN_POINT('Ctrl Pts',(3.74080745251389,2.59788110634618,4.81101738301186));
#19779=CARTESIAN_POINT('Ctrl Pts',(3.84261718390667,2.38901942599691,4.79990359395504));
#19780=CARTESIAN_POINT('Ctrl Pts',(3.72235665540369,2.19020838956081,4.78878980489825));
#19781=CARTESIAN_POINT('Ctrl Pts',(3.49010169259086,2.18342199335841,4.77767601584144));
#19782=CARTESIAN_POINT('Ctrl Pts',(3.35843789688119,2.37487190279669,4.76656222678464));
#19783=CARTESIAN_POINT('Ctrl Pts',(3.44787863365674,2.58932184457717,4.75544843772783));
#19784=CARTESIAN_POINT('Ctrl Pts',(3.67655778221991,2.63048335496042,4.74433464867103));
#19785=CARTESIAN_POINT('Ctrl Pts',(3.8351627244929,2.46068083668937,4.73322085961423));
#19786=CARTESIAN_POINT('Ctrl Pts',(3.77852055811084,2.23533646042905,4.72210707055742));
#19787=CARTESIAN_POINT('Ctrl Pts',(3.55847650032912,2.16071048934957,4.71099328150062));
#19788=CARTESIAN_POINT('Ctrl Pts',(3.37643937270466,2.30510892109605,4.69987949244382));
#19789=CARTESIAN_POINT('Ctrl Pts',(3.39902982259358,2.53636223350135,4.68876570338701));
#19790=CARTESIAN_POINT('Ctrl Pts',(3.60557055501943,2.64280164712995,4.67765191433021));
#19791=CARTESIAN_POINT('Ctrl Pts',(3.80701249526159,2.52700195958257,4.6665381252734));
#19792=CARTESIAN_POINT('Ctrl Pts',(3.81897355090948,2.29495593812904,4.65542433621659));
#19793=CARTESIAN_POINT('Ctrl Pts',(3.63050563208088,2.15905793778677,4.6443105471598));
#19794=CARTESIAN_POINT('Ctrl Pts',(3.41411556225142,2.24369693945694,4.63319675810298));
#19795=CARTESIAN_POINT('Ctrl Pts',(3.3678676263658,2.47140190503977,4.62208296904619));
#19796=CARTESIAN_POINT('Ctrl Pts',(3.53409308462842,2.63375189718637,4.61096917998938));
#19797=CARTESIAN_POINT('Ctrl Pts',(3.76064388996454,2.58214612691277,4.59985539093257));
#19798=CARTESIAN_POINT('Ctrl Pts',(3.84015552099323,2.36381994099575,4.58874160187577));
#19799=CARTESIAN_POINT('Ctrl Pts',(3.6998500801025,2.17860977340027,4.57762781281896));
#19800=CARTESIAN_POINT('Ctrl Pts',(3.46815072852799,2.1960405909371,4.56651402376216));
#19801=CARTESIAN_POINT('Ctrl Pts',(3.3571345103823,2.40015776866696,4.55540023470536));
#19802=CARTESIAN_POINT('Ctrl Pts',(3.46841582920963,2.6041305389052,4.54428644564855));
#19803=CARTESIAN_POINT('Ctrl Pts',(3.70013763173937,2.6212603119689,4.53317265659175));
#19804=CARTESIAN_POINT('Ctrl Pts',(3.84020232447629,2.43586801205837,4.52205886753494));
#19805=CARTESIAN_POINT('Ctrl Pts',(3.76040710518764,2.21764531427324,4.51094507847815));
#19806=CARTESIAN_POINT('Ctrl Pts',(3.53378944408678,2.16633392770918,4.49983128942133));
#19807=CARTESIAN_POINT('Ctrl Pts',(3.36777505427786,2.32889974840269,4.48871750036454));
#19808=CARTESIAN_POINT('Ctrl Pts',(3.4143187937299,2.55654443303944,4.47760371130772));
#19809=CARTESIAN_POINT('Ctrl Pts',(3.63081864137997,2.64090222813732,4.46648992225093));
#19810=CARTESIAN_POINT('Ctrl Pts',(3.81910984841827,2.50475947107891,4.45537613319412));
#19811=CARTESIAN_POINT('Ctrl Pts',(3.80684730359907,2.27272920356226,4.44426234413732));
#19812=CARTESIAN_POINT('Ctrl Pts',(3.60525512148808,2.15719129638054,4.43314855508051));
#19813=CARTESIAN_POINT('Ctrl Pts',(3.39885277598246,2.26389903533996,4.42203476602371));
#19814=CARTESIAN_POINT('Ctrl Pts',(3.3765629481812,2.49518135839549,4.4109209769669));
#19815=CARTESIAN_POINT('Ctrl Pts',(3.55878722266986,2.63934344974957,4.3998071879101));
#19816=CARTESIAN_POINT('Ctrl Pts',(3.77873475080197,2.56443107632444,4.38869339885329));
#19817=CARTESIAN_POINT('Ctrl Pts',(3.8350828706128,2.33901445723046,4.37757960979649));
#19818=CARTESIAN_POINT('Ctrl Pts',(3.67625990394949,2.16941582752504,4.36646582073968));
#19819=CARTESIAN_POINT('Ctrl Pts',(3.44762951395987,2.21087905095695,4.35535203168288));
#19820=CARTESIAN_POINT('Ctrl Pts',(3.35847730739013,2.42543572165447,4.34423824262608));
#19821=CARTESIAN_POINT('Ctrl Pts',(3.49037003538787,2.61673301642169,4.33312445356927));
#19822=CARTESIAN_POINT('Ctrl Pts',(3.72265542052987,2.60960761604941,4.32201066451248));
#19823=CARTESIAN_POINT('Ctrl Pts',(3.84257850979074,2.41071512516748,4.31089687545566));
#19824=CARTESIAN_POINT('Ctrl Pts',(3.7406568756376,2.20183613957205,4.29978308639887));
#19825=CARTESIAN_POINT('Ctrl Pts',(3.50959639242813,2.17470169312488,4.28866929734205));
#19826=CARTESIAN_POINT('Ctrl Pts',(3.41142456563631,2.29356865430551,4.28126010463752));
#19827=CARTESIAN_POINT('Ctrl Pts',(3.39833241385534,2.360627924571,4.27755550828525));
#19828=CARTESIAN_POINT('Ctrl Pts',(3.55032651029123,2.21400211999972,5.20748149723825));
#19829=CARTESIAN_POINT('Ctrl Pts',(3.48847779011663,2.2305197371096,5.20377690088598));
#19830=CARTESIAN_POINT('Ctrl Pts',(3.38363102379655,2.32987260795489,5.19636770818144));
#19831=CARTESIAN_POINT('Ctrl Pts',(3.42374108957258,2.54412674142112,5.18525391912464));
#19832=CARTESIAN_POINT('Ctrl Pts',(3.62549702318155,2.62606856404868,5.17414013006783));
#19833=CARTESIAN_POINT('Ctrl Pts',(3.8037602238433,2.50127641096634,5.16302634101103));
#19834=CARTESIAN_POINT('Ctrl Pts',(3.79559667859298,2.28369088196908,5.15191255195422));
#19835=CARTESIAN_POINT('Ctrl Pts',(3.60836267793897,2.1726112820345,5.14079876289743));
#19836=CARTESIAN_POINT('Ctrl Pts',(3.41349350034069,2.269639745597,5.12968497384062));
#19837=CARTESIAN_POINT('Ctrl Pts',(3.38932620899373,2.48600011991624,5.11857118478381));
#19838=CARTESIAN_POINT('Ctrl Pts',(3.55799583654811,2.62363776975738,5.10745739572701));
#19839=CARTESIAN_POINT('Ctrl Pts',(3.76510994947867,2.55658014925731,5.0963436066702));
#19840=CARTESIAN_POINT('Ctrl Pts',(3.82109825277221,2.34620148571036,5.08522981761341));
#19841=CARTESIAN_POINT('Ctrl Pts',(3.67471221873066,2.18506593996663,5.0741160285566));
#19842=CARTESIAN_POINT('Ctrl Pts',(3.45994154284032,2.22066161350478,5.0630022394998));
#19843=CARTESIAN_POINT('Ctrl Pts',(3.37336781169642,2.42040792753322,5.05188845044299));
#19844=CARTESIAN_POINT('Ctrl Pts',(3.49423316734106,2.60147454339935,5.04077466138619));
#19845=CARTESIAN_POINT('Ctrl Pts',(3.71190806711109,2.59812927009101,5.02966087232938));
#19846=CARTESIAN_POINT('Ctrl Pts',(3.82715226255275,2.41343400631629,5.01854708327258));
#19847=CARTESIAN_POINT('Ctrl Pts',(3.73448140669699,2.21644245550271,5.00743329421577));
#19848=CARTESIAN_POINT('Ctrl Pts',(3.51871819881407,2.18746320121053,4.99631950515897));
#19849=CARTESIAN_POINT('Ctrl Pts',(3.37735314303472,2.35302129199909,4.98520571610216));
#19850=CARTESIAN_POINT('Ctrl Pts',(3.43977928158165,2.56157952558844,4.97409192704536));
#19851=CARTESIAN_POINT('Ctrl Pts',(3.64885726014462,2.62224218767309,4.96297813798855));
#19852=CARTESIAN_POINT('Ctrl Pts',(3.81321563470729,2.47948405463168,4.95186434893176));
#19853=CARTESIAN_POINT('Ctrl Pts',(3.78241532064824,2.26397326515074,4.94075055987495));
#19854=CARTESIAN_POINT('Ctrl Pts',(3.58464819494153,2.17296928863785,4.92963677081815));
#19855=CARTESIAN_POINT('Ctrl Pts',(3.40093275047013,2.28976909698186,4.91852298176134));
#19856=CARTESIAN_POINT('Ctrl Pts',(3.39942581708757,2.50746450093999,4.90740919270454));
#19857=CARTESIAN_POINT('Ctrl Pts',(3.58150670798172,2.62679642846834,4.89629540364773));
#19858=CARTESIAN_POINT('Ctrl Pts',(3.78051471879288,2.53853901296773,4.88518161459093));
#19859=CARTESIAN_POINT('Ctrl Pts',(3.81429556031454,2.32347526776122,4.87406782553412));
#19860=CARTESIAN_POINT('Ctrl Pts',(3.65192924520447,2.17845547782099,4.86295403647733));
#19861=CARTESIAN_POINT('Ctrl Pts',(3.4420315030405,2.23621790151766,4.85184024742051));
#19862=CARTESIAN_POINT('Ctrl Pts',(3.37672411762845,2.4438919373702,4.84072645836372));
#19863=CARTESIAN_POINT('Ctrl Pts',(3.51578367947165,2.61139118517954,4.8296126693069));
#19864=CARTESIAN_POINT('Ctrl Pts',(3.73192739457257,2.58540168385487,4.81849888025011));
#19865=CARTESIAN_POINT('Ctrl Pts',(3.82731646926276,2.38971191869978,4.8073850911933));
#19866=CARTESIAN_POINT('Ctrl Pts',(3.71464020169267,2.20343895103354,4.7962713021365));
#19867=CARTESIAN_POINT('Ctrl Pts',(3.49703245740495,2.19708054064022,4.78515751307969));
#19868=CARTESIAN_POINT('Ctrl Pts',(3.37367207258585,2.37645661266209,4.77404372402289));
#19869=CARTESIAN_POINT('Ctrl Pts',(3.45747220646219,2.57738221411453,4.76292993496608));
#19870=CARTESIAN_POINT('Ctrl Pts',(3.6717296461388,2.6159478633368,4.75181614590928));
#19871=CARTESIAN_POINT('Ctrl Pts',(3.82033212723505,2.45685398423157,4.74070235685248));
#19872=CARTESIAN_POINT('Ctrl Pts',(3.7672621135368,2.24572100859114,4.72958856779567));
#19873=CARTESIAN_POINT('Ctrl Pts',(3.56109519043692,2.17580134343001,4.71847477873887));
#19874=CARTESIAN_POINT('Ctrl Pts',(3.39053828074069,2.31109325121307,4.70736098968206));
#19875=CARTESIAN_POINT('Ctrl Pts',(3.41170405813995,2.52776251443194,4.69624720062526));
#19876=CARTESIAN_POINT('Ctrl Pts',(3.60521924654496,2.62748929926577,4.68513341156846));
#19877=CARTESIAN_POINT('Ctrl Pts',(3.79395719939706,2.51899254857754,4.67401962251165));
#19878=CARTESIAN_POINT('Ctrl Pts',(3.80516392801682,2.30158056870897,4.66290583345484));
#19879=CARTESIAN_POINT('Ctrl Pts',(3.62858178660552,2.17425301045342,4.65179204439804));
#19880=CARTESIAN_POINT('Ctrl Pts',(3.42583841177484,2.25355423187469,4.64067825534123));
#19881=CARTESIAN_POINT('Ctrl Pts',(3.38250711377307,2.46689892566933,4.62956446628444));
#19882=CARTESIAN_POINT('Ctrl Pts',(3.53824952107254,2.61901027411281,4.61845067722762));
#19883=CARTESIAN_POINT('Ctrl Pts',(3.7505128420311,2.57065903491661,4.60733688817083));
#19884=CARTESIAN_POINT('Ctrl Pts',(3.82501005174943,2.36610164565372,4.59622309911402));
#19885=CARTESIAN_POINT('Ctrl Pts',(3.69355300930883,2.19257180456232,4.58510931005721));
#19886=CARTESIAN_POINT('Ctrl Pts',(3.47646583649485,2.20890334314105,4.57399552100041));
#19887=CARTESIAN_POINT('Ctrl Pts',(3.37245088448926,2.4001478189457,4.5628817319436));
#19888=CARTESIAN_POINT('Ctrl Pts',(3.47671421853432,2.59125699435405,4.55176794288681));
#19889=CARTESIAN_POINT('Ctrl Pts',(3.69382242642831,2.60730647390622,4.54065415382999));
#19890=CARTESIAN_POINT('Ctrl Pts',(3.82505390355888,2.43360598672071,4.5295403647732));
#19891=CARTESIAN_POINT('Ctrl Pts',(3.75029099014661,2.22914555908425,4.51842657571639));
#19892=CARTESIAN_POINT('Ctrl Pts',(3.53796502969918,2.18107013821379,4.50731278665959));
#19893=CARTESIAN_POINT('Ctrl Pts',(3.3824203797675,2.33338370392177,4.49619899760278));
#19894=CARTESIAN_POINT('Ctrl Pts',(3.42602882640825,2.54667191840358,4.48508520854598));
#19895=CARTESIAN_POINT('Ctrl Pts',(3.62887505589326,2.62570966761684,4.47397141948917));
#19896=CARTESIAN_POINT('Ctrl Pts',(3.80529162988842,2.49815278828994,4.46285763043237));
#19897=CARTESIAN_POINT('Ctrl Pts',(3.79380242558891,2.28075556883219,4.45174384137556));
#19898=CARTESIAN_POINT('Ctrl Pts',(3.60492370590979,2.17250408926403,4.44063005231877));
#19899=CARTESIAN_POINT('Ctrl Pts',(3.41153817701856,2.2724822774232,4.42951626326195));
#19900=CARTESIAN_POINT('Ctrl Pts',(3.39065406289825,2.48917872172821,4.41840247420516));
#19901=CARTESIAN_POINT('Ctrl Pts',(3.56138631699392,2.62424919398607,4.40728868514835));
#19902=CARTESIAN_POINT('Ctrl Pts',(3.76746279811117,2.55406118851634,4.39617489609155));
#19903=CARTESIAN_POINT('Ctrl Pts',(3.82025730936029,2.342860526055,4.38506110703474));
#19904=CARTESIAN_POINT('Ctrl Pts',(3.67145055363756,2.18395767723095,4.37394731797794));
#19905=CARTESIAN_POINT('Ctrl Pts',(3.4572387975626,2.22280601189145,4.36283352892113));
#19906=CARTESIAN_POINT('Ctrl Pts',(3.37370899766098,2.42383161137452,4.35171973986432));
#19907=CARTESIAN_POINT('Ctrl Pts',(3.49728387709496,2.60306469340852,4.34060595080753));
#19908=CARTESIAN_POINT('Ctrl Pts',(3.71492012511989,2.59638865822985,4.32949216175072));
#19909=CARTESIAN_POINT('Ctrl Pts',(3.82728023413982,2.4100393730632,4.31837837269392));
#19910=CARTESIAN_POINT('Ctrl Pts',(3.73178631386543,2.21433339402172,4.30726458363711));
#19911=CARTESIAN_POINT('Ctrl Pts',(3.51529771901994,2.18891018836724,4.29615079458031));
#19912=CARTESIAN_POINT('Ctrl Pts',(3.42331712354828,2.30028077429395,4.28874160187577));
#19913=CARTESIAN_POINT('Ctrl Pts',(3.41105063166184,2.36311093455973,4.2850370055235));
#19914=CARTESIAN_POINT('Ctrl Pts',(3.55367004230132,2.22652167256662,5.2149629944765));
#19915=CARTESIAN_POINT('Ctrl Pts',(3.49598437120782,2.24192748573719,5.21125839812423));
#19916=CARTESIAN_POINT('Ctrl Pts',(3.39819486060706,2.33459289600918,5.20384920541969));
#19917=CARTESIAN_POINT('Ctrl Pts',(3.43560511025108,2.5344255431305,5.19273541636289));
#19918=CARTESIAN_POINT('Ctrl Pts',(3.62378081371712,2.61085184614133,5.18162162730608));
#19919=CARTESIAN_POINT('Ctrl Pts',(3.79004508454469,2.4944594765428,5.17050783824928));
#19920=CARTESIAN_POINT('Ctrl Pts',(3.78243102907294,2.29151967075525,5.15939404919247));
#19921=CARTESIAN_POINT('Ctrl Pts',(3.60779978450139,2.18791685975229,5.14828026013568));
#19922=CARTESIAN_POINT('Ctrl Pts',(3.42604728819327,2.27841431903638,5.13716647107886));
#19923=CARTESIAN_POINT('Ctrl Pts',(3.40350670180884,2.48021143553957,5.12605268202207));
#19924=CARTESIAN_POINT('Ctrl Pts',(3.56082314475379,2.60858466907463,5.11493889296526));
#19925=CARTESIAN_POINT('Ctrl Pts',(3.75399636747541,2.54604070972415,5.10382510390846));
#19926=CARTESIAN_POINT('Ctrl Pts',(3.80621608745921,2.34982267390707,5.09271131485165));
#19927=CARTESIAN_POINT('Ctrl Pts',(3.66968332512291,2.19953319229768,5.08159752579485));
#19928=CARTESIAN_POINT('Ctrl Pts',(3.46936890414598,2.23273291430124,5.07048373673804));
#19929=CARTESIAN_POINT('Ctrl Pts',(3.38862246725923,2.41903426606174,5.05936994768124));
#19930=CARTESIAN_POINT('Ctrl Pts',(3.50135235290009,2.58791325368478,5.04825615862443));
#19931=CARTESIAN_POINT('Ctrl Pts',(3.70437551389675,2.58479315135706,5.03714236956764));
#19932=CARTESIAN_POINT('Ctrl Pts',(3.81186260069363,2.41252976080414,5.02602858051082));
#19933=CARTESIAN_POINT('Ctrl Pts',(3.72542943771535,2.22879774862422,5.01491479145403));
#19934=CARTESIAN_POINT('Ctrl Pts',(3.52418929226243,2.20176909343275,5.00380100239722));
#19935=CARTESIAN_POINT('Ctrl Pts',(3.39233954518956,2.35618343774151,4.99268721334042));
#19936=CARTESIAN_POINT('Ctrl Pts',(3.45056376851527,2.55070357708658,4.98157342428361));
#19937=CARTESIAN_POINT('Ctrl Pts',(3.64556866870124,2.60728302388504,4.9704596352268));
#19938=CARTESIAN_POINT('Ctrl Pts',(3.79886404991074,2.47413396784473,4.95934584617));
#19939=CARTESIAN_POINT('Ctrl Pts',(3.77013691083056,2.27312925046329,4.9482320571132));
#19940=CARTESIAN_POINT('Ctrl Pts',(3.58568152785062,2.18825076886329,4.93711826805639));
#19941=CARTESIAN_POINT('Ctrl Pts',(3.41433200477794,2.29718875996312,4.92600447899959));
#19942=CARTESIAN_POINT('Ctrl Pts',(3.41292650336706,2.5002310450071,4.91489068994278));
#19943=CARTESIAN_POINT('Ctrl Pts',(3.58275149497368,2.61153071786889,4.90377690088598));
#19944=CARTESIAN_POINT('Ctrl Pts',(3.76836423884643,2.52921392573871,4.89266311182918));
#19945=CARTESIAN_POINT('Ctrl Pts',(3.79987128552062,2.32862616199684,4.88154932277237));
#19946=CARTESIAN_POINT('Ctrl Pts',(3.64843387786428,2.19336768161237,4.87043553371557));
#19947=CARTESIAN_POINT('Ctrl Pts',(3.45266439252072,2.24724210561861,4.85932174465876));
#19948=CARTESIAN_POINT('Ctrl Pts',(3.39175285960263,2.44093756274417,4.84820795560197));
#19949=CARTESIAN_POINT('Ctrl Pts',(3.52145229597333,2.59716240442661,4.83709416654515));
#19950=CARTESIAN_POINT('Ctrl Pts',(3.72304733663125,2.57292226136356,4.82598037748836));
#19951=CARTESIAN_POINT('Ctrl Pts',(3.81201575461885,2.39040441140265,4.81486658843155));
#19952=CARTESIAN_POINT('Ctrl Pts',(3.70692374798164,2.21666951250626,4.80375279937475));
#19953=CARTESIAN_POINT('Ctrl Pts',(3.50396322221905,2.21073908792203,4.79263901031794));
#19954=CARTESIAN_POINT('Ctrl Pts',(3.3889062482905,2.37804132252749,4.78152522126113));
#19955=CARTESIAN_POINT('Ctrl Pts',(3.46706577926762,2.56544258365188,4.77041143220433));
#19956=CARTESIAN_POINT('Ctrl Pts',(3.66690151005769,2.60141237171319,4.75929764314753));
#19957=CARTESIAN_POINT('Ctrl Pts',(3.80550152997722,2.45302713177377,4.74818385409072));
#19958=CARTESIAN_POINT('Ctrl Pts',(3.75600366896275,2.25610555675324,4.73707006503392));
#19959=CARTESIAN_POINT('Ctrl Pts',(3.56371388054473,2.19089219751045,4.72595627597711));
#19960=CARTESIAN_POINT('Ctrl Pts',(3.40463718877671,2.31707758133011,4.71484248692031));
#19961=CARTESIAN_POINT('Ctrl Pts',(3.42437829368633,2.51916279536252,4.7037286978635));
#19962=CARTESIAN_POINT('Ctrl Pts',(3.60486793807048,2.61217695140159,4.69261490880671));
#19963=CARTESIAN_POINT('Ctrl Pts',(3.78090190353252,2.51098313757252,4.6815011197499));
#19964=CARTESIAN_POINT('Ctrl Pts',(3.79135430512417,2.3082051992889,4.67038733069309));
#19965=CARTESIAN_POINT('Ctrl Pts',(3.62665794113017,2.18944808312007,4.65927354163629));
#19966=CARTESIAN_POINT('Ctrl Pts',(3.43756126129826,2.26341152429244,4.64815975257949));
#19967=CARTESIAN_POINT('Ctrl Pts',(3.39714660118035,2.46239594629889,4.63704596352268));
#19968=CARTESIAN_POINT('Ctrl Pts',(3.54240595751667,2.60426865103925,4.62593217446588));
#19969=CARTESIAN_POINT('Ctrl Pts',(3.74038179409766,2.55917194292045,4.61481838540907));
#19970=CARTESIAN_POINT('Ctrl Pts',(3.80986458250562,2.36838335031169,4.60370459635227));
#19971=CARTESIAN_POINT('Ctrl Pts',(3.68725593851517,2.20653383572437,4.59259080729547));
#19972=CARTESIAN_POINT('Ctrl Pts',(3.48478094446172,2.221766095345,4.58147701823866));
#19973=CARTESIAN_POINT('Ctrl Pts',(3.38776725859624,2.40013786922444,4.57036322918186));
#19974=CARTESIAN_POINT('Ctrl Pts',(3.48501260785902,2.57838344980291,4.55924944012505));
#19975=CARTESIAN_POINT('Ctrl Pts',(3.68750722111726,2.59335263584353,4.54813565106824));
#19976=CARTESIAN_POINT('Ctrl Pts',(3.80990548264146,2.43134396138305,4.53702186201145));
#19977=CARTESIAN_POINT('Ctrl Pts',(3.74017487510557,2.24064580389526,4.52590807295464));
#19978=CARTESIAN_POINT('Ctrl Pts',(3.54214061531159,2.19580634871841,4.51479428389784));
#19979=CARTESIAN_POINT('Ctrl Pts',(3.39706570525713,2.33786765944084,4.50368049484103));
#19980=CARTESIAN_POINT('Ctrl Pts',(3.4377388590866,2.53679940376773,4.49256670578423));
#19981=CARTESIAN_POINT('Ctrl Pts',(3.62693147040654,2.61051710709635,4.48145291672742));
#19982=CARTESIAN_POINT('Ctrl Pts',(3.79147341135858,2.49154610550097,4.47033912767062));
#19983=CARTESIAN_POINT('Ctrl Pts',(3.78075754757875,2.28878193410212,4.45922533861381));
#19984=CARTESIAN_POINT('Ctrl Pts',(3.60459229033149,2.18781688214753,4.44811154955701));
#19985=CARTESIAN_POINT('Ctrl Pts',(3.42422357805467,2.28106551950643,4.43699776050021));
#19986=CARTESIAN_POINT('Ctrl Pts',(3.4047451776153,2.48317608506094,4.4258839714434));
#19987=CARTESIAN_POINT('Ctrl Pts',(3.56398541131798,2.60915493822257,4.4147701823866));
#19988=CARTESIAN_POINT('Ctrl Pts',(3.75619084542037,2.54369130070823,4.40365639332979));
#19989=CARTESIAN_POINT('Ctrl Pts',(3.80543174810779,2.34670659487954,4.39254260427299));
#19990=CARTESIAN_POINT('Ctrl Pts',(3.66664120332562,2.19849952693685,4.38142881521618));
#19991=CARTESIAN_POINT('Ctrl Pts',(3.46684808116532,2.23473297282595,4.37031502615938));
#19992=CARTESIAN_POINT('Ctrl Pts',(3.38894068793183,2.42222750109457,4.35920123710257));
#19993=CARTESIAN_POINT('Ctrl Pts',(3.50419771880206,2.58939637039535,4.34808744804578));
#19994=CARTESIAN_POINT('Ctrl Pts',(3.70718482970991,2.5831697004103,4.33697365898896));
#19995=CARTESIAN_POINT('Ctrl Pts',(3.81198195848891,2.40936362095891,4.32585986993217));
#19996=CARTESIAN_POINT('Ctrl Pts',(3.72291575209325,2.22683064847139,4.31474608087536));
#19997=CARTESIAN_POINT('Ctrl Pts',(3.52099904561175,2.2031186836096,4.30363229181856));
#19998=CARTESIAN_POINT('Ctrl Pts',(3.43520968146025,2.30699289428239,4.29622309911402));
#19999=CARTESIAN_POINT('Ctrl Pts',(3.42376884946835,2.36559394454846,4.29251850276175));
#20000=CARTESIAN_POINT('Ctrl Pts',(3.55701357431141,2.23904122513352,5.22244449171475));
#20001=CARTESIAN_POINT('Ctrl Pts',(3.50349095229901,2.25333523436478,5.21873989536248));
#20002=CARTESIAN_POINT('Ctrl Pts',(3.41275869741756,2.33931318406347,5.21133070265794));
#20003=CARTESIAN_POINT('Ctrl Pts',(3.44746913092958,2.52472434483988,5.20021691360114));
#20004=CARTESIAN_POINT('Ctrl Pts',(3.62206460425269,2.59563512823397,5.18910312454433));
#20005=CARTESIAN_POINT('Ctrl Pts',(3.77632994524609,2.48764254211926,5.17798933548754));
#20006=CARTESIAN_POINT('Ctrl Pts',(3.76926537955289,2.29934845954141,5.16687554643072));
#20007=CARTESIAN_POINT('Ctrl Pts',(3.60723689106381,2.20322243747008,5.15576175737393));
#20008=CARTESIAN_POINT('Ctrl Pts',(3.43860107604584,2.28718889247577,5.14464796831712));
#20009=CARTESIAN_POINT('Ctrl Pts',(3.41768719462395,2.47442275116291,5.13353417926031));
#20010=CARTESIAN_POINT('Ctrl Pts',(3.56365045295948,2.59353156839189,5.12242039020351));
#20011=CARTESIAN_POINT('Ctrl Pts',(3.74288278547214,2.53550127019098,5.1113066011467));
#20012=CARTESIAN_POINT('Ctrl Pts',(3.79133392214622,2.35344386210378,5.1001928120899));
#20013=CARTESIAN_POINT('Ctrl Pts',(3.66465443151516,2.21400044462873,5.0890790230331));
#20014=CARTESIAN_POINT('Ctrl Pts',(3.47879626545164,2.24480421509772,5.0779652339763));
#20015=CARTESIAN_POINT('Ctrl Pts',(3.40387712282204,2.41766060459026,5.06685144491948));
#20016=CARTESIAN_POINT('Ctrl Pts',(3.50847153845911,2.57435196397021,5.05573765586269));
#20017=CARTESIAN_POINT('Ctrl Pts',(3.69684296068241,2.57145703262312,5.04462386680587));
#20018=CARTESIAN_POINT('Ctrl Pts',(3.7965729388345,2.41162551529198,5.03351007774909));
#20019=CARTESIAN_POINT('Ctrl Pts',(3.71637746873371,2.24115304174574,5.02239628869227));
#20020=CARTESIAN_POINT('Ctrl Pts',(3.5296603857108,2.21607498565497,5.01128249963547));
#20021=CARTESIAN_POINT('Ctrl Pts',(3.40732594734439,2.35934558348393,5.00016871057866));
#20022=CARTESIAN_POINT('Ctrl Pts',(3.46134825544889,2.53982762858472,4.98905492152187));
#20023=CARTESIAN_POINT('Ctrl Pts',(3.64228007725786,2.59232386009698,4.97794113246505));
#20024=CARTESIAN_POINT('Ctrl Pts',(3.7845124651142,2.46878388105777,4.96682734340826));
#20025=CARTESIAN_POINT('Ctrl Pts',(3.75785850101288,2.28228523577585,4.95571355435144));
#20026=CARTESIAN_POINT('Ctrl Pts',(3.58671486075972,2.20353224908873,4.94459976529465));
#20027=CARTESIAN_POINT('Ctrl Pts',(3.42773125908574,2.30460842294439,4.93348597623783));
#20028=CARTESIAN_POINT('Ctrl Pts',(3.42642718964655,2.4929975890742,4.92237218718104));
#20029=CARTESIAN_POINT('Ctrl Pts',(3.58399628196565,2.59626500726946,4.91125839812423));
#20030=CARTESIAN_POINT('Ctrl Pts',(3.75621375889998,2.51988883850969,4.90014460906743));
#20031=CARTESIAN_POINT('Ctrl Pts',(3.7854470107267,2.33377705623246,4.88903082001062));
#20032=CARTESIAN_POINT('Ctrl Pts',(3.6449385105241,2.20827988540375,4.87791703095382));
#20033=CARTESIAN_POINT('Ctrl Pts',(3.46329728200094,2.25826630971955,4.86680324189701));
#20034=CARTESIAN_POINT('Ctrl Pts',(3.40678160157682,2.43798318811813,4.85568945284022));
#20035=CARTESIAN_POINT('Ctrl Pts',(3.527120912475,2.58293362367368,4.8445756637834));
#20036=CARTESIAN_POINT('Ctrl Pts',(3.71416727868993,2.56044283887224,4.8334618747266));
#20037=CARTESIAN_POINT('Ctrl Pts',(3.79671503997494,2.39109690410553,4.82234808566979));
#20038=CARTESIAN_POINT('Ctrl Pts',(3.69920729427062,2.22990007397898,4.811234296613));
#20039=CARTESIAN_POINT('Ctrl Pts',(3.51089398703315,2.22439763520385,4.80012050755619));
#20040=CARTESIAN_POINT('Ctrl Pts',(3.40414042399517,2.37962603239289,4.78900671849938));
#20041=CARTESIAN_POINT('Ctrl Pts',(3.47665935207306,2.55350295318923,4.77789292944258));
#20042=CARTESIAN_POINT('Ctrl Pts',(3.66207337397658,2.58687688008957,4.76677914038578));
#20043=CARTESIAN_POINT('Ctrl Pts',(3.79067093271938,2.44920027931597,4.75566535132897));
#20044=CARTESIAN_POINT('Ctrl Pts',(3.7447452243887,2.26649010491534,4.74455156227217));
#20045=CARTESIAN_POINT('Ctrl Pts',(3.56633257065254,2.20598305159089,4.73343777321536));
#20046=CARTESIAN_POINT('Ctrl Pts',(3.41873609681274,2.32306191144714,4.72232398415856));
#20047=CARTESIAN_POINT('Ctrl Pts',(3.4370525292327,2.5105630762931,4.71121019510175));
#20048=CARTESIAN_POINT('Ctrl Pts',(3.604516629596,2.59686460353741,4.70009640604495));
#20049=CARTESIAN_POINT('Ctrl Pts',(3.76784660766799,2.50297372656749,4.68898261698814));
#20050=CARTESIAN_POINT('Ctrl Pts',(3.77754468223151,2.31482982986883,4.67786882793134));
#20051=CARTESIAN_POINT('Ctrl Pts',(3.62473409565482,2.20464315578672,4.66675503887454));
#20052=CARTESIAN_POINT('Ctrl Pts',(3.44928411082169,2.27326881671019,4.65564124981774));
#20053=CARTESIAN_POINT('Ctrl Pts',(3.41178608858762,2.45789296692846,4.64452746076093));
#20054=CARTESIAN_POINT('Ctrl Pts',(3.5465623939608,2.58952702796569,4.63341367170412));
#20055=CARTESIAN_POINT('Ctrl Pts',(3.73025074616421,2.54768485092428,4.62229988264732));
#20056=CARTESIAN_POINT('Ctrl Pts',(3.79471911326182,2.37066505496967,4.61118609359052));
#20057=CARTESIAN_POINT('Ctrl Pts',(3.6809588677215,2.22049586688641,4.60007230453371));
#20058=CARTESIAN_POINT('Ctrl Pts',(3.49309605242859,2.23462884754895,4.58895851547691));
#20059=CARTESIAN_POINT('Ctrl Pts',(3.4030836327032,2.40012791950318,4.5778447264201));
#20060=CARTESIAN_POINT('Ctrl Pts',(3.49331099718372,2.56550990525176,4.56673093736331));
#20061=CARTESIAN_POINT('Ctrl Pts',(3.6811920158062,2.57939879778085,4.55561714830649));
#20062=CARTESIAN_POINT('Ctrl Pts',(3.79475706172405,2.42908193604538,4.5445033592497));
#20063=CARTESIAN_POINT('Ctrl Pts',(3.73005876006454,2.25214604870627,4.53338957019289));
#20064=CARTESIAN_POINT('Ctrl Pts',(3.54631620092399,2.21054255922302,4.52227578113609));
#20065=CARTESIAN_POINT('Ctrl Pts',(3.41171103074677,2.34235161495991,4.51116199207928));
#20066=CARTESIAN_POINT('Ctrl Pts',(3.44944889176494,2.52692688913187,4.50004820302248));
#20067=CARTESIAN_POINT('Ctrl Pts',(3.62498788491984,2.59532454657587,4.48893441396567));
#20068=CARTESIAN_POINT('Ctrl Pts',(3.77765519282873,2.484939422712,4.47782062490886));
#20069=CARTESIAN_POINT('Ctrl Pts',(3.76771266956859,2.29680829937205,4.46670683585207));
#20070=CARTESIAN_POINT('Ctrl Pts',(3.6042608747532,2.20312967503102,4.45559304679526));
#20071=CARTESIAN_POINT('Ctrl Pts',(3.43690897909078,2.28964876158967,4.44447925773845));
#20072=CARTESIAN_POINT('Ctrl Pts',(3.41883629233234,2.47717344839367,4.43336546868165));
#20073=CARTESIAN_POINT('Ctrl Pts',(3.56658450564204,2.59406068245907,4.42225167962485));
#20074=CARTESIAN_POINT('Ctrl Pts',(3.74491889272957,2.53332141290012,4.41113789056804));
#20075=CARTESIAN_POINT('Ctrl Pts',(3.7906061868553,2.35055266370407,4.40002410151124));
#20076=CARTESIAN_POINT('Ctrl Pts',(3.66183185301368,2.21304137664276,4.38891031245443));
#20077=CARTESIAN_POINT('Ctrl Pts',(3.47645736476805,2.24665993376045,4.37779652339763));
#20078=CARTESIAN_POINT('Ctrl Pts',(3.40417237820268,2.42062339081462,4.36668273434083));
#20079=CARTESIAN_POINT('Ctrl Pts',(3.51111156050916,2.57572804738218,4.35556894528402));
#20080=CARTESIAN_POINT('Ctrl Pts',(3.69944953429992,2.56995074259074,4.34445515622722));
#20081=CARTESIAN_POINT('Ctrl Pts',(3.796683682838,2.40868786885462,4.33334136717041));
#20082=CARTESIAN_POINT('Ctrl Pts',(3.71404519032108,2.23932790292106,4.32222757811361));
#20083=CARTESIAN_POINT('Ctrl Pts',(3.52670037220356,2.21732717885196,4.3111137890568));
#20084=CARTESIAN_POINT('Ctrl Pts',(3.44710223937223,2.31370501427082,4.30370459635227));
#20085=CARTESIAN_POINT('Ctrl Pts',(3.43648706727485,2.36807695453719,4.3));
#20086=CARTESIAN_POINT('Ctrl Pts',(3.43361558566414,2.40009421455432,5.13785196366098));
#20087=CARTESIAN_POINT('Ctrl Pts',(3.43350387426567,2.42168271797136,5.13641270219409));
#20088=CARTESIAN_POINT('Ctrl Pts',(3.43740295903752,2.4432325339629,5.1349734407272));
#20089=CARTESIAN_POINT('Ctrl Pts',(3.44550005125019,2.46306857758655,5.13353417926031));
#20090=CARTESIAN_POINT('Ctrl Pts',(3.46634161406913,2.51412569023923,5.12982958290805));
#20091=CARTESIAN_POINT('Ctrl Pts',(3.5149960335143,2.55382862931556,5.12612498655578));
#20092=CARTESIAN_POINT('Ctrl Pts',(3.56919529865567,2.56400838248691,5.12242039020351));
#20093=CARTESIAN_POINT('Ctrl Pts',(3.62339456379703,2.57418813565826,5.11871579385124));
#20094=CARTESIAN_POINT('Ctrl Pts',(3.68313867463459,2.55484470292462,5.11501119749897));
#20095=CARTESIAN_POINT('Ctrl Pts',(3.72108591949905,2.51483008520994,5.1113066011467));
#20096=CARTESIAN_POINT('Ctrl Pts',(3.7590331643635,2.47481546749525,5.10760200479444));
#20097=CARTESIAN_POINT('Ctrl Pts',(3.77518354325486,2.41412966479952,5.10389740844217));
#20098=CARTESIAN_POINT('Ctrl Pts',(3.76214548426203,2.36054619387247,5.1001928120899));
#20099=CARTESIAN_POINT('Ctrl Pts',(3.7491074252692,2.30696272294543,5.09648821573763));
#20100=CARTESIAN_POINT('Ctrl Pts',(3.70688092839218,2.26048158378708,5.09278361938537));
#20101=CARTESIAN_POINT('Ctrl Pts',(3.65479131894308,2.24237497595273,5.0890790230331));
#20102=CARTESIAN_POINT('Ctrl Pts',(3.60270170949399,2.22426836811839,5.08537442668083));
#20103=CARTESIAN_POINT('Ctrl Pts',(3.54074898747281,2.23453629160805,5.08166983032856));
#20104=CARTESIAN_POINT('Ctrl Pts',(3.49728610269062,2.26847965160164,5.0779652339763));
#20105=CARTESIAN_POINT('Ctrl Pts',(3.45773596364813,2.29936726097326,5.07459414387119));
#20106=CARTESIAN_POINT('Ctrl Pts',(3.43349641790554,2.34985942255505,5.07122305376608));
#20107=CARTESIAN_POINT('Ctrl Pts',(3.43317938608394,2.40008640134203,5.06785196366098));
#20108=CARTESIAN_POINT('Ctrl Pts',(3.54698297828114,2.20148256743283,5.2));
#20109=CARTESIAN_POINT('Ctrl Pts',(3.5345795220974,2.20607510740599,5.2));
#20110=CARTESIAN_POINT('Ctrl Pts',(3.52273022202852,2.21193437307052,5.2));
#20111=CARTESIAN_POINT('Ctrl Pts',(3.51155282869243,2.21889712518446,5.2));
#20112=CARTESIAN_POINT('Ctrl Pts',(3.50588663673039,2.22242677551307,5.2));
#20113=CARTESIAN_POINT('Ctrl Pts',(3.50039354941666,2.2262407482932,5.2));
#20114=CARTESIAN_POINT('Ctrl Pts',(3.49509234222245,2.23032135431632,5.2));
#20115=CARTESIAN_POINT('Ctrl Pts',(3.49050523644823,2.2338522805309,5.2));
#20116=CARTESIAN_POINT('Ctrl Pts',(3.48606182302158,2.23758289719759,5.2));
#20117=CARTESIAN_POINT('Ctrl Pts',(3.48177607353762,2.24150262969935,5.2));
#20118=CARTESIAN_POINT('Ctrl Pts',(3.4786657164721,2.24434735212827,5.2));
#20119=CARTESIAN_POINT('Ctrl Pts',(3.47564458925343,2.24728626535177,5.2));
#20120=CARTESIAN_POINT('Ctrl Pts',(3.47272209234032,2.25030915184069,5.2));
#20121=CARTESIAN_POINT('Ctrl Pts',(3.4637771038367,2.25956140622969,5.2));
#20122=CARTESIAN_POINT('Ctrl Pts',(3.45573639448352,2.26961351156597,5.2));
#20123=CARTESIAN_POINT('Ctrl Pts',(3.44873900472013,2.28033442966861,5.2));
#20124=CARTESIAN_POINT('Ctrl Pts',(3.44420815653473,2.28727628284152,5.2));
#20125=CARTESIAN_POINT('Ctrl Pts',(3.44011557094646,2.29449912284867,5.2));
#20126=CARTESIAN_POINT('Ctrl Pts',(3.43651072814608,2.30197002765831,5.2));
#20127=CARTESIAN_POINT('Ctrl Pts',(3.43484397915084,2.30542430396786,5.2));
#20128=CARTESIAN_POINT('Ctrl Pts',(3.43328563163244,2.30892352292903,5.2));
#20129=CARTESIAN_POINT('Ctrl Pts',(3.43184081732517,2.31246073059787,5.2));
#20130=CARTESIAN_POINT('Ctrl Pts',(3.42783869836044,2.3222587550377,5.2));
#20131=CARTESIAN_POINT('Ctrl Pts',(3.42470154623616,2.33235626573064,5.2));
#20132=CARTESIAN_POINT('Ctrl Pts',(3.42252347569321,2.34267987754179,5.2));
#20133=CARTESIAN_POINT('Ctrl Pts',(3.42066968522458,2.35146646769115,5.2));
#20134=CARTESIAN_POINT('Ctrl Pts',(3.41951139095334,2.36041732716722,5.2));
#20135=CARTESIAN_POINT('Ctrl Pts',(3.41903596356978,2.36945415649734,5.2));
#20136=CARTESIAN_POINT('Ctrl Pts',(3.41886682155969,2.37266917424891,5.2));
#20137=CARTESIAN_POINT('Ctrl Pts',(3.41878447232058,2.37589363434567,5.2));
#20138=CARTESIAN_POINT('Ctrl Pts',(3.41878798568376,2.3791143017356,5.2));
#20139=CARTESIAN_POINT('Ctrl Pts',(3.41880075844281,2.39082297128446,5.2));
#20140=CARTESIAN_POINT('Ctrl Pts',(3.41994282155898,2.40251786108517,5.2));
#20141=CARTESIAN_POINT('Ctrl Pts',(3.42216878897262,2.41402665747967,5.2));
#20142=CARTESIAN_POINT('Ctrl Pts',(3.42331180168116,2.41993631296624,5.2));
#20143=CARTESIAN_POINT('Ctrl Pts',(3.42474130312271,2.42579671745434,5.2));
#20144=CARTESIAN_POINT('Ctrl Pts',(3.4264550762976,2.43158227576526,5.2));
#20145=CARTESIAN_POINT('Ctrl Pts',(3.42814231216907,2.43727824630656,5.2));
#20146=CARTESIAN_POINT('Ctrl Pts',(3.43010783958643,2.44290710782216,5.2));
#20147=CARTESIAN_POINT('Ctrl Pts',(3.43233768577066,2.4484115412056,5.2));
#20148=CARTESIAN_POINT('Ctrl Pts',(3.43579440729991,2.4569445483329,5.2));
#20149=CARTESIAN_POINT('Ctrl Pts',(3.43988798414899,2.46519216359733,5.2));
#20150=CARTESIAN_POINT('Ctrl Pts',(3.44460907372922,2.4730585225122,5.2));
#20151=CARTESIAN_POINT('Ctrl Pts',(3.44702309019998,2.47708079738387,5.2));
#20152=CARTESIAN_POINT('Ctrl Pts',(3.44960209705083,2.48100348334585,5.2));
#20153=CARTESIAN_POINT('Ctrl Pts',(3.45233605468006,2.48480007154667,5.2));
#20154=CARTESIAN_POINT('Ctrl Pts',(3.45777065901345,2.49234698978257,5.2));
#20155=CARTESIAN_POINT('Ctrl Pts',(3.46382415870923,2.499410402925,5.2));
#20156=CARTESIAN_POINT('Ctrl Pts',(3.47049190322584,2.5058791831385,5.2));
#20157=CARTESIAN_POINT('Ctrl Pts',(3.47127037259775,2.50663442312367,5.2));
#20158=CARTESIAN_POINT('Ctrl Pts',(3.47205722899383,2.5073815321984,5.2));
#20159=CARTESIAN_POINT('Ctrl Pts',(3.47285231527688,2.50812044463164,5.2));
#20160=CARTESIAN_POINT('Origin',(3.6,2.4,4.7));
#20161=CARTESIAN_POINT('Origin',(3.6,-2.4,4.3));
#20162=CARTESIAN_POINT('Ctrl Pts',(3.43648706727485,-2.43192304546281,4.3));
#20163=CARTESIAN_POINT('Ctrl Pts',(3.43713128683253,-2.44021936733391,4.3));
#20164=CARTESIAN_POINT('Ctrl Pts',(3.43844438912273,-2.44842976439641,4.3));
#20165=CARTESIAN_POINT('Ctrl Pts',(3.44036779101517,-2.45650290183658,4.3));
#20166=CARTESIAN_POINT('Ctrl Pts',(3.44142971550231,-2.46096014104879,4.3));
#20167=CARTESIAN_POINT('Ctrl Pts',(3.44267796071139,-2.46537560589173,4.3));
#20168=CARTESIAN_POINT('Ctrl Pts',(3.44410466214797,-2.4697408265362,4.3));
#20169=CARTESIAN_POINT('Ctrl Pts',(3.44564437628146,-2.47445182755564,4.3));
#20170=CARTESIAN_POINT('Ctrl Pts',(3.44738954450943,-2.47909640503965,4.3));
#20171=CARTESIAN_POINT('Ctrl Pts',(3.44932653760859,-2.48365784749895,4.3));
#20172=CARTESIAN_POINT('Ctrl Pts',(3.45254730792056,-2.49124246845553,4.3));
#20173=CARTESIAN_POINT('Ctrl Pts',(3.45629958145885,-2.49860290469935,4.3));
#20174=CARTESIAN_POINT('Ctrl Pts',(3.460540361967,-2.50569093557372,4.3));
#20175=CARTESIAN_POINT('Ctrl Pts',(3.46239352486579,-2.50878830781843,4.3));
#20176=CARTESIAN_POINT('Ctrl Pts',(3.46433983439221,-2.51183274422802,4.3));
#20177=CARTESIAN_POINT('Ctrl Pts',(3.46636982169588,-2.5148117549636,4.3));
#20178=CARTESIAN_POINT('Ctrl Pts',(3.4732458122516,-2.52490228589753,4.3));
#20179=CARTESIAN_POINT('Ctrl Pts',(3.48109363537456,-2.5342702737356,4.3));
#20180=CARTESIAN_POINT('Ctrl Pts',(3.4897794934809,-2.54276723354547,4.3));
#20181=CARTESIAN_POINT('Ctrl Pts',(3.49400930325249,-2.54690505426423,4.3));
#20182=CARTESIAN_POINT('Ctrl Pts',(3.49843862851918,-2.55083612678489,4.3));
#20183=CARTESIAN_POINT('Ctrl Pts',(3.50305595405548,-2.55454125034048,4.3));
#20184=CARTESIAN_POINT('Ctrl Pts',(3.50696190635494,-2.55767554004086,4.3));
#20185=CARTESIAN_POINT('Ctrl Pts',(3.51100694759131,-2.56065060854479,4.3));
#20186=CARTESIAN_POINT('Ctrl Pts',(3.51515869554757,-2.56343734237232,4.3));
#20187=CARTESIAN_POINT('Ctrl Pts',(3.52023397904373,-2.56684397118314,4.3));
#20188=CARTESIAN_POINT('Ctrl Pts',(3.52547419237578,-2.56997446151731,4.3));
#20189=CARTESIAN_POINT('Ctrl Pts',(3.53086407609141,-2.57281069688687,4.3));
#20190=CARTESIAN_POINT('Ctrl Pts',(3.53843716228638,-2.57679576522158,4.3));
#20191=CARTESIAN_POINT('Ctrl Pts',(3.5463054085634,-2.58020053156405,4.3));
#20192=CARTESIAN_POINT('Ctrl Pts',(3.55440202217605,-2.58304072456499,4.3));
#20193=CARTESIAN_POINT('Ctrl Pts',(3.56031216163472,-2.58511392918216,4.3));
#20194=CARTESIAN_POINT('Ctrl Pts',(3.5663442123363,-2.58688610080112,4.3));
#20195=CARTESIAN_POINT('Ctrl Pts',(3.57247443059928,-2.58835971156752,4.3));
#20196=CARTESIAN_POINT('Ctrl Pts',(3.57600236806727,-2.58920777380822,4.3));
#20197=CARTESIAN_POINT('Ctrl Pts',(3.57955832823423,-2.58995565186198,4.3));
#20198=CARTESIAN_POINT('Ctrl Pts',(3.58312950627136,-2.59060308036101,4.3));
#20199=CARTESIAN_POINT('Ctrl Pts',(3.59464642713376,-2.59269101400921,4.3));
#20200=CARTESIAN_POINT('Ctrl Pts',(3.6063444588111,-2.59374267077427,4.3));
#20201=CARTESIAN_POINT('Ctrl Pts',(3.61806681517941,-2.59379134323091,4.3));
#20202=CARTESIAN_POINT('Ctrl Pts',(3.62473112824741,-2.59381901415975,4.3));
#20203=CARTESIAN_POINT('Ctrl Pts',(3.63140369181744,-2.59352192189353,4.3));
#20204=CARTESIAN_POINT('Ctrl Pts',(3.63805736597901,-2.59290136699938,4.3));
#20205=CARTESIAN_POINT('Ctrl Pts',(3.64215429545284,-2.59251926688834,4.3));
#20206=CARTESIAN_POINT('Ctrl Pts',(3.64624613464129,-2.59201413768455,4.3));
#20207=CARTESIAN_POINT('Ctrl Pts',(3.65032004640889,-2.59138662655135,4.3));
#20208=CARTESIAN_POINT('Ctrl Pts',(3.6635759835922,-2.58934479338508,4.3));
#20209=CARTESIAN_POINT('Ctrl Pts',(3.67655554403262,-2.58602558677096,4.3));
#20210=CARTESIAN_POINT('Ctrl Pts',(3.68904453335804,-2.58146163637399,4.3));
#20211=CARTESIAN_POINT('Ctrl Pts',(3.69937751045428,-2.5776855746214,4.3));
#20212=CARTESIAN_POINT('Ctrl Pts',(3.70937567296629,-2.57305657585047,4.3));
#20213=CARTESIAN_POINT('Ctrl Pts',(3.7189159065364,-2.56756614624894,4.3));
#20214=CARTESIAN_POINT('Ctrl Pts',(3.72007018633274,-2.56690185517936,4.3));
#20215=CARTESIAN_POINT('Ctrl Pts',(3.72121775119647,-2.56622492375,4.3));
#20216=CARTESIAN_POINT('Ctrl Pts',(3.72235852099786,-2.56553552032368,4.3));
#20217=CARTESIAN_POINT('Ctrl Pts',(3.78826275096637,-2.48232321801033,4.3));
#20218=CARTESIAN_POINT('Ctrl Pts',(3.79091867325729,-2.4742706313139,4.3));
#20219=CARTESIAN_POINT('Ctrl Pts',(3.79302804122654,-2.46606039506531,4.3));
#20220=CARTESIAN_POINT('Ctrl Pts',(3.79460324133206,-2.45774386615892,4.3));
#20221=CARTESIAN_POINT('Ctrl Pts',(3.79578956705146,-2.45148046374845,4.3));
#20222=CARTESIAN_POINT('Ctrl Pts',(3.79667272255332,-2.44515671383718,4.3));
#20223=CARTESIAN_POINT('Ctrl Pts',(3.79725488779627,-2.43879482378833,4.3));
#20224=CARTESIAN_POINT('Ctrl Pts',(3.79769087373759,-2.43403037820329,4.3));
#20225=CARTESIAN_POINT('Ctrl Pts',(3.79795758751143,-2.42924591021267,4.3));
#20226=CARTESIAN_POINT('Ctrl Pts',(3.79805591662036,-2.4244630110418,4.3));
#20227=CARTESIAN_POINT('Ctrl Pts',(3.79826160078478,-2.41445817493456,4.3));
#20228=CARTESIAN_POINT('Ctrl Pts',(3.79773307923007,-2.40444525216584,4.3));
#20229=CARTESIAN_POINT('Ctrl Pts',(3.7964780509907,-2.39451257334247,4.3));
#20230=CARTESIAN_POINT('Ctrl Pts',(3.79582248849211,-2.38932425044823,4.3));
#20231=CARTESIAN_POINT('Ctrl Pts',(3.7949674129287,-2.38415491083777,4.3));
#20232=CARTESIAN_POINT('Ctrl Pts',(3.79391844712734,-2.37904222861684,4.3));
#20233=CARTESIAN_POINT('Ctrl Pts',(3.79135149974265,-2.3665308710123,4.3));
#20234=CARTESIAN_POINT('Ctrl Pts',(3.78762424888679,-2.35432630792998,4.3));
#20235=CARTESIAN_POINT('Ctrl Pts',(3.78275036269461,-2.34261709433331,4.3));
#20236=CARTESIAN_POINT('Ctrl Pts',(3.78051279286925,-2.33724146962858,4.3));
#20237=CARTESIAN_POINT('Ctrl Pts',(3.77803293300414,-2.33197059787363,4.3));
#20238=CARTESIAN_POINT('Ctrl Pts',(3.77530918258224,-2.32682518237142,4.3));
#20239=CARTESIAN_POINT('Ctrl Pts',(3.77352855433059,-2.32346141154425,4.3));
#20240=CARTESIAN_POINT('Ctrl Pts',(3.77164258388613,-2.32014955771335,4.3));
#20241=CARTESIAN_POINT('Ctrl Pts',(3.76965386637616,-2.31690144569075,4.3));
#20242=CARTESIAN_POINT('Ctrl Pts',(3.76538144816038,-2.30992343453397,4.3));
#20243=CARTESIAN_POINT('Ctrl Pts',(3.76065257819642,-2.3032660772289,4.3));
#20244=CARTESIAN_POINT('Ctrl Pts',(3.7554693784929,-2.29698171698016,4.3));
#20245=CARTESIAN_POINT('Ctrl Pts',(3.74976402854315,-2.29006427669614,4.3));
#20246=CARTESIAN_POINT('Ctrl Pts',(3.74350800901797,-2.28359846633093,4.3));
#20247=CARTESIAN_POINT('Ctrl Pts',(3.73677358655615,-2.27761728545388,4.3));
#20248=CARTESIAN_POINT('Ctrl Pts',(3.73252958089122,-2.2738479695743,4.3));
#20249=CARTESIAN_POINT('Ctrl Pts',(3.72809540845025,-2.27027136680987,4.3));
#20250=CARTESIAN_POINT('Ctrl Pts',(3.72348829039508,-2.26689850911598,4.3));
#20251=CARTESIAN_POINT('Ctrl Pts',(3.72067474538276,-2.26483872101672,4.3));
#20252=CARTESIAN_POINT('Ctrl Pts',(3.71780010895487,-2.26285764263401,4.3));
#20253=CARTESIAN_POINT('Ctrl Pts',(3.71487541375918,-2.26096143585197,4.3));
#20254=CARTESIAN_POINT('Ctrl Pts',(3.70626359340869,-2.25537801909854,4.3));
#20255=CARTESIAN_POINT('Ctrl Pts',(3.69720132775591,-2.25051601191126,4.3));
#20256=CARTESIAN_POINT('Ctrl Pts',(3.6877975535831,-2.24642648892188,4.3));
#20257=CARTESIAN_POINT('Ctrl Pts',(3.67897161991428,-2.24258825780551,4.3));
#20258=CARTESIAN_POINT('Ctrl Pts',(3.66984418789588,-2.23943054868187,4.3));
#20259=CARTESIAN_POINT('Ctrl Pts',(3.66050482692203,-2.23701743659906,4.3));
#20260=CARTESIAN_POINT('Ctrl Pts',(3.65701754284817,-2.23611638915498,4.3));
#20261=CARTESIAN_POINT('Ctrl Pts',(3.65350925028094,-2.23532164136865,4.3));
#20262=CARTESIAN_POINT('Ctrl Pts',(3.64998794572223,-2.2346361398089,4.3));
#20263=CARTESIAN_POINT('Ctrl Pts',(3.63890673460959,-2.23247893148594,4.3));
#20264=CARTESIAN_POINT('Ctrl Pts',(3.62768565700141,-2.23139728883196,4.3));
#20265=CARTESIAN_POINT('Ctrl Pts',(3.61647532022068,-2.23148774583768,4.3));
#20266=CARTESIAN_POINT('Ctrl Pts',(3.61029342610439,-2.23153762798149,4.3));
#20267=CARTESIAN_POINT('Ctrl Pts',(3.60411490309515,-2.23194477515726,4.3));
#20268=CARTESIAN_POINT('Ctrl Pts',(3.59796731355722,-2.23273189751379,4.3));
#20269=CARTESIAN_POINT('Ctrl Pts',(3.59689164899642,-2.23286962297817,4.3));
#20270=CARTESIAN_POINT('Ctrl Pts',(3.59581693782457,-2.2330189937725,4.3));
#20271=CARTESIAN_POINT('Ctrl Pts',(3.5947433329992,-2.23317993884958,4.3));
#20272=CARTESIAN_POINT('Origin',(3.6,-2.4,5.35459252805377));
#20273=CARTESIAN_POINT('Ctrl Pts',(3.39434265963601,-2.39985006386652,5.17959252805377));
#20274=CARTESIAN_POINT('Ctrl Pts',(3.39426084301402,-2.39002096866549,5.17905813053169));
#20275=CARTESIAN_POINT('Ctrl Pts',(3.39937061245186,-2.31213684688635,5.17481913665734));
#20276=CARTESIAN_POINT('Ctrl Pts',(3.49890445172815,-2.1791570162937,5.16687554643073));
#20277=CARTESIAN_POINT('Ctrl Pts',(3.73070050348011,-2.19531101338576,5.15576175737392));
#20278=CARTESIAN_POINT('Ctrl Pts',(3.84286217522106,-2.398786946145,5.14464796831712));
#20279=CARTESIAN_POINT('Ctrl Pts',(3.73273070558319,-2.60338928804541,5.13353417926031));
#20280=CARTESIAN_POINT('Ctrl Pts',(3.50110863577888,-2.62181907448596,5.12242039020351));
#20281=CARTESIAN_POINT('Ctrl Pts',(3.39978420932204,-2.4892623620427,5.11443983980132));
#20282=CARTESIAN_POINT('Ctrl Pts',(3.3942709677865,-2.41067410874191,5.11016388575141));
#20283=CARTESIAN_POINT('Ctrl Pts',(3.39436118987868,-2.40016037422423,5.10959252805377));
#20284=CARTESIAN_POINT('Ctrl Pts',(3.39473290683218,-2.40022967700174,5.18540747194623));
#20285=CARTESIAN_POINT('Ctrl Pts',(3.39508769549541,-2.35320983503088,5.18286245525962));
#20286=CARTESIAN_POINT('Ctrl Pts',(3.4343446160921,-2.23704698664849,5.17661284222074));
#20287=CARTESIAN_POINT('Ctrl Pts',(3.62721323091929,-2.15871475485289,5.16665863282959));
#20288=CARTESIAN_POINT('Ctrl Pts',(3.81747535364037,-2.29190664293025,5.15554484377279));
#20289=CARTESIAN_POINT('Ctrl Pts',(3.80876232171537,-2.52413791100821,5.14443105471598));
#20290=CARTESIAN_POINT('Ctrl Pts',(3.60892556988421,-2.64269428158759,5.13331726565918));
#20291=CARTESIAN_POINT('Ctrl Pts',(3.42787437077081,-2.55254601515802,5.12364273806926));
#20292=CARTESIAN_POINT('Ctrl Pts',(3.39500775643356,-2.44179202298147,5.11767280683161));
#20293=CARTESIAN_POINT('Ctrl Pts',(3.39479089893477,-2.39988380139174,5.11540747194623));
#20294=CARTESIAN_POINT('Ctrl Pts',(3.72690708798524,-2.29206413469515,5.2));
#20295=CARTESIAN_POINT('Ctrl Pts',(3.76279833110066,-2.33426376069605,5.19629540364773));
#20296=CARTESIAN_POINT('Ctrl Pts',(3.78852079223234,-2.45658683270444,5.18888621094319));
#20297=CARTESIAN_POINT('Ctrl Pts',(3.65451255926051,-2.58934148319728,5.1777724218864));
#20298=CARTESIAN_POINT('Ctrl Pts',(3.47057723832131,-2.54835675254144,5.16665863282959));
#20299=CARTESIAN_POINT('Ctrl Pts',(3.40512138630522,-2.37179019391731,5.15554484377279));
#20300=CARTESIAN_POINT('Ctrl Pts',(3.51803130141336,-2.22093957374148,5.14443105471598));
#20301=CARTESIAN_POINT('Ctrl Pts',(3.7059725216196,-2.23403730298123,5.13331726565917));
#20302=CARTESIAN_POINT('Ctrl Pts',(3.79691367996997,-2.39901645079819,5.12220347660237));
#20303=CARTESIAN_POINT('Ctrl Pts',(3.70761861808084,-2.56490889591613,5.11108968754556));
#20304=CARTESIAN_POINT('Ctrl Pts',(3.5198184631744,-2.57985184479553,5.09997589848876));
#20305=CARTESIAN_POINT('Ctrl Pts',(3.40540965360542,-2.43017761320763,5.08886210943196));
#20306=CARTESIAN_POINT('Ctrl Pts',(3.46911145738791,-2.25287984568082,5.07774832037515));
#20307=CARTESIAN_POINT('Ctrl Pts',(3.65261709726835,-2.21024363500907,5.06663453131835));
#20308=CARTESIAN_POINT('Ctrl Pts',(3.7879616770095,-2.34129317212888,5.05552074226154));
#20309=CARTESIAN_POINT('Ctrl Pts',(3.75126281927757,-2.52607793686066,5.04440695320475));
#20310=CARTESIAN_POINT('Ctrl Pts',(3.57611137907248,-2.59546203514889,5.03329316414793));
#20311=CARTESIAN_POINT('Ctrl Pts',(3.42282546878807,-2.4859375664189,5.02217937509114));
#20312=CARTESIAN_POINT('Ctrl Pts',(3.43170941408529,-2.29775344335704,5.01106558603433));
#20313=CARTESIAN_POINT('Ctrl Pts',(3.59463164228021,-2.20315676572473,4.99995179697753));
#20314=CARTESIAN_POINT('Ctrl Pts',(3.76246758864558,-2.28873292649683,4.98883800792072));
#20315=CARTESIAN_POINT('Ctrl Pts',(3.78159510888145,-2.47615310463782,4.97772421886392));
#20316=CARTESIAN_POINT('Ctrl Pts',(3.63450656639691,-2.59386948090233,4.96661042980711));
#20317=CARTESIAN_POINT('Ctrl Pts',(3.45583377242442,-2.53413492344978,4.95549664075031));
#20318=CARTESIAN_POINT('Ctrl Pts',(3.40911796147502,-2.3516251489795,4.94438285169351));
#20319=CARTESIAN_POINT('Ctrl Pts',(3.53711864515359,-2.21339342445149,4.93326906263669));
#20320=CARTESIAN_POINT('Ctrl Pts',(3.7226753460379,-2.24596481468812,4.9221552735799));
#20321=CARTESIAN_POINT('Ctrl Pts',(3.7959459114648,-2.41952635696717,4.91104148452308));
#20322=CARTESIAN_POINT('Ctrl Pts',(3.68986496194813,-2.57521520324594,4.89992769546629));
#20323=CARTESIAN_POINT('Ctrl Pts',(3.50152959362338,-2.57052758693027,4.88881390640948));
#20324=CARTESIAN_POINT('Ctrl Pts',(3.403325304985,-2.4097541363769,4.87770011735268));
#20325=CARTESIAN_POINT('Ctrl Pts',(3.48513959513685,-2.24005261418135,4.86658632829587));
#20326=CARTESIAN_POINT('Ctrl Pts',(3.6720869164654,-2.21675274815082,4.85547253923907));
#20327=CARTESIAN_POINT('Ctrl Pts',(3.79305226563199,-2.36118116990379,4.84435875018227));
#20328=CARTESIAN_POINT('Ctrl Pts',(3.73731468670399,-2.54114090707891,4.83324496112546));
#20329=CARTESIAN_POINT('Ctrl Pts',(3.55589141778138,-2.59191277135814,4.82213117206866));
#20330=CARTESIAN_POINT('Ctrl Pts',(3.41484123438881,-2.46702469957432,4.81101738301185));
#20331=CARTESIAN_POINT('Ctrl Pts',(3.44326896900338,-2.28078816015838,4.79990359395505));
#20332=CARTESIAN_POINT('Ctrl Pts',(3.61515439373994,-2.20366756970366,4.78878980489824));
#20333=CARTESIAN_POINT('Ctrl Pts',(3.77316883002382,-2.3062522792604,4.77767601584144));
#20334=CARTESIAN_POINT('Ctrl Pts',(3.77267987231879,-2.49464534078155,4.76656222678464));
#20335=CARTESIAN_POINT('Ctrl Pts',(3.61413506915742,-2.59640844853418,4.75544843772783));
#20336=CARTESIAN_POINT('Ctrl Pts',(3.44265227689368,-2.51839667592017,4.74433464867102));
#20337=CARTESIAN_POINT('Ctrl Pts',(3.4151916400337,-2.33201508312681,4.73322085961423));
#20338=CARTESIAN_POINT('Ctrl Pts',(3.55688819092022,-2.20786085574886,4.72210707055742));
#20339=CARTESIAN_POINT('Ctrl Pts',(3.73804546957863,-2.25957376611009,4.71099328150061));
#20340=CARTESIAN_POINT('Ctrl Pts',(3.79284816438962,-2.43982040089255,4.69987949244382));
#20341=CARTESIAN_POINT('Ctrl Pts',(3.67113474728785,-2.58361897114401,4.688765703387));
#20342=CARTESIAN_POINT('Ctrl Pts',(3.48431088927061,-2.55934901472658,4.67765191433021));
#20343=CARTESIAN_POINT('Ctrl Pts',(3.40337858630773,-2.38922509798919,4.66653812527339));
#20344=CARTESIAN_POINT('Ctrl Pts',(3.50241609313587,-2.22896357125796,4.6554243362166));
#20345=CARTESIAN_POINT('Ctrl Pts',(3.69077325659353,-2.22525362743943,4.64431054715978));
#20346=CARTESIAN_POINT('Ctrl Pts',(3.79604462885236,-2.38149102018406,4.63319675810299));
#20347=CARTESIAN_POINT('Ctrl Pts',(3.72187412902538,-2.5546698920607,4.62208296904618));
#20348=CARTESIAN_POINT('Ctrl Pts',(3.53615085675469,-2.58627765765756,4.61096917998938));
#20349=CARTESIAN_POINT('Ctrl Pts',(3.40886942939528,-2.44738337066962,4.59985539093257));
#20350=CARTESIAN_POINT('Ctrl Pts',(3.45653198087784,-2.26511854714084,4.58874160187577));
#20351=CARTESIAN_POINT('Ctrl Pts',(3.63551243730216,-2.20631224707971,4.57762781281896));
#20352=CARTESIAN_POINT('Ctrl Pts',(3.78198795712288,-2.32479054382313,4.56651402376216));
#20353=CARTESIAN_POINT('Ctrl Pts',(3.76188783591025,-2.51210890876234,4.55540023470536));
#20354=CARTESIAN_POINT('Ctrl Pts',(3.59360994254596,-2.59681271806211,4.54428644564855));
#20355=CARTESIAN_POINT('Ctrl Pts',(3.43118094125773,-2.50137161460726,4.53317265659175));
#20356=CARTESIAN_POINT('Ctrl Pts',(3.42327393893419,-2.31314392247853,4.52205886753494));
#20357=CARTESIAN_POINT('Ctrl Pts',(3.57712630459504,-2.2044165835037,4.51094507847814));
#20358=CARTESIAN_POINT('Ctrl Pts',(3.75191522290318,-2.2747089629466,4.49983128942133));
#20359=CARTESIAN_POINT('Ctrl Pts',(3.78765441517707,-2.45968165103968,4.48871750036453));
#20360=CARTESIAN_POINT('Ctrl Pts',(3.6516313924431,-2.59002704401991,4.47760371130773));
#20361=CARTESIAN_POINT('Ctrl Pts',(3.46834957196871,-2.54643853472375,4.46648992225092));
#20362=CARTESIAN_POINT('Ctrl Pts',(3.40556887868038,-2.36881316151698,4.45537613319412));
#20363=CARTESIAN_POINT('Ctrl Pts',(3.52075320095807,-2.21973347999151,4.44426234413732));
#20364=CARTESIAN_POINT('Ctrl Pts',(3.70847300665902,-2.23565373905929,4.43314855508051));
#20365=CARTESIAN_POINT('Ctrl Pts',(3.79690626014289,-2.40200209376731,4.4220347660237));
#20366=CARTESIAN_POINT('Ctrl Pts',(3.70510893870568,-2.56651771072077,4.4109209769669));
#20367=CARTESIAN_POINT('Ctrl Pts',(3.51710429764661,-2.57861817635772,4.3998071879101));
#20368=CARTESIAN_POINT('Ctrl Pts',(3.4049748648587,-2.42722660301959,4.3886933988533));
#20369=CARTESIAN_POINT('Ctrl Pts',(3.47135448681048,-2.25091580613535,4.37757960979649));
#20370=CARTESIAN_POINT('Ctrl Pts',(3.65548413146169,-2.21106026869437,4.36646582073969));
#20371=CARTESIAN_POINT('Ctrl Pts',(3.78882987196794,-2.34414980590083,4.35535203168288));
#20372=CARTESIAN_POINT('Ctrl Pts',(3.74933478455633,-2.5283468513898,4.34423824262608));
#20373=CARTESIAN_POINT('Ctrl Pts',(3.57315729153603,-2.59509221614966,4.33312445356927));
#20374=CARTESIAN_POINT('Ctrl Pts',(3.42153838470822,-2.4832160988167,4.32201066451247));
#20375=CARTESIAN_POINT('Ctrl Pts',(3.43328918604681,-2.2952742544727,4.31089687545567));
#20376=CARTESIAN_POINT('Ctrl Pts',(3.59758810222901,-2.20298223652265,4.29978308639886));
#20377=CARTESIAN_POINT('Ctrl Pts',(3.76418972838082,-2.29144636425406,4.28866929734206));
#20378=CARTESIAN_POINT('Ctrl Pts',(3.77483953817107,-2.41599017382994,4.28126010463752));
#20379=CARTESIAN_POINT('Ctrl Pts',(3.75264423560529,-2.46674801372684,4.27755550828525));
#20380=CARTESIAN_POINT('Ctrl Pts',(3.73677806246588,-2.28366876301903,5.20748149723825));
#20381=CARTESIAN_POINT('Ctrl Pts',(3.77546096639785,-2.32915072287504,5.20377690088598));
#20382=CARTESIAN_POINT('Ctrl Pts',(3.80318414917118,-2.46098821950194,5.19636770818144));
#20383=CARTESIAN_POINT('Ctrl Pts',(3.65875260676202,-2.60406867439235,5.18525391912464));
#20384=CARTESIAN_POINT('Ctrl Pts',(3.46051059194224,-2.55989610579284,5.17414013006784));
#20385=CARTESIAN_POINT('Ctrl Pts',(3.38996351094031,-2.36959600381834,5.16302634101104));
#20386=CARTESIAN_POINT('Ctrl Pts',(3.51165568485162,-2.20701205459222,5.15191255195423));
#20387=CARTESIAN_POINT('Ctrl Pts',(3.71421518223977,-2.22112853978274,5.14079876289742));
#20388=CARTESIAN_POINT('Ctrl Pts',(3.81222984505367,-2.39893994924713,5.12968497384063));
#20389=CARTESIAN_POINT('Ctrl Pts',(3.71598931391495,-2.57773569329255,5.11857118478381));
#20390=CARTESIAN_POINT('Ctrl Pts',(3.51358185404256,-2.59384092135901,5.10745739572702));
#20391=CARTESIAN_POINT('Ctrl Pts',(3.3902741999918,-2.43252486153385,5.0963436066702));
#20392=CARTESIAN_POINT('Ctrl Pts',(3.45893080093723,-2.2414366764148,5.08522981761341));
#20393=CARTESIAN_POINT('Ctrl Pts',(3.65670971362751,-2.19548417384656,5.07411602855659));
#20394=CARTESIAN_POINT('Ctrl Pts',(3.80258154534432,-2.33672688974895,5.0630022394998));
#20395=CARTESIAN_POINT('Ctrl Pts',(3.76302820963254,-2.53588441904446,5.05188845044299));
#20396=CARTESIAN_POINT('Ctrl Pts',(3.57425329556196,-2.61066528968353,5.04077466138618));
#20397=CARTESIAN_POINT('Ctrl Pts',(3.40904463665349,-2.49262188593578,5.02966087232938));
#20398=CARTESIAN_POINT('Ctrl Pts',(3.41861958509882,-2.28980059243768,5.01854708327258));
#20399=CARTESIAN_POINT('Ctrl Pts',(3.59421408544476,-2.18784607998553,5.00743329421577));
#20400=CARTESIAN_POINT('Ctrl Pts',(3.77510449842668,-2.28007844974125,4.99631950515897));
#20401=CARTESIAN_POINT('Ctrl Pts',(3.79571977846481,-2.48207637783269,4.98520571610217));
#20402=CARTESIAN_POINT('Ctrl Pts',(3.63719052551791,-2.60894886479604,4.97409192704536));
#20403=CARTESIAN_POINT('Ctrl Pts',(3.4446203628666,-2.54456808701342,4.96297813798855));
#20404=CARTESIAN_POINT('Ctrl Pts',(3.39427094417278,-2.34786249925276,4.95186434893176));
#20405=CARTESIAN_POINT('Ctrl Pts',(3.53222766342159,-2.19887895741578,4.94075055987495));
#20406=CARTESIAN_POINT('Ctrl Pts',(3.73221717092231,-2.23398378661889,4.92963677081814));
#20407=CARTESIAN_POINT('Ctrl Pts',(3.81118680243757,-2.42104513873408,4.91852298176134));
#20408=CARTESIAN_POINT('Ctrl Pts',(3.69685475865827,-2.58884363667168,4.90740919270454));
#20409=CARTESIAN_POINT('Ctrl Pts',(3.4938704558725,-2.58379141234426,4.89629540364773));
#20410=CARTESIAN_POINT('Ctrl Pts',(3.38802772841696,-2.41051282395524,4.88518161459093));
#20411=CARTESIAN_POINT('Ctrl Pts',(3.47620562507071,-2.22761172857971,4.87406782553412));
#20412=CARTESIAN_POINT('Ctrl Pts',(3.67769391702081,-2.20249957304951,4.86295403647733));
#20413=CARTESIAN_POINT('Ctrl Pts',(3.80806808561287,-2.35816179811509,4.85184024742051));
#20414=CARTESIAN_POINT('Ctrl Pts',(3.74799517579086,-2.552119003843,4.84072645836372));
#20415=CARTESIAN_POINT('Ctrl Pts',(3.55246060318804,-2.60683996020677,4.8296126693069));
#20416=CARTESIAN_POINT('Ctrl Pts',(3.40043937962063,-2.4722379552685,4.8184988802501));
#20417=CARTESIAN_POINT('Ctrl Pts',(3.43107825505782,-2.27151573063888,4.8073850911933));
#20418=CARTESIAN_POINT('Ctrl Pts',(3.61633311934347,-2.18839661486619,4.79627130213649));
#20419=CARTESIAN_POINT('Ctrl Pts',(3.78663809426387,-2.29896047725209,4.78515751307969));
#20420=CARTESIAN_POINT('Ctrl Pts',(3.7861111048846,-2.50200696067527,4.77404372402288));
#20421=CARTESIAN_POINT('Ctrl Pts',(3.61523451056097,-2.61168531615476,4.76292993496608));
#20422=CARTESIAN_POINT('Ctrl Pts',(3.43041359594979,-2.52760570108303,4.75181614590928));
#20423=CARTESIAN_POINT('Ctrl Pts',(3.40081704020639,-2.32672714066293,4.74070235685248));
#20424=CARTESIAN_POINT('Ctrl Pts',(3.55353490645048,-2.19291605936479,4.72958856779566));
#20425=CARTESIAN_POINT('Ctrl Pts',(3.74878279977045,-2.24865125742167,4.71847477873887));
#20426=CARTESIAN_POINT('Ctrl Pts',(3.80784810914882,-2.44291767597198,4.70736098968206));
#20427=CARTESIAN_POINT('Ctrl Pts',(3.67666768706539,-2.59790105898559,4.69624720062525));
#20428=CARTESIAN_POINT('Ctrl Pts',(3.47531246154031,-2.57174335835902,4.68513341156846));
#20429=CARTESIAN_POINT('Ctrl Pts',(3.38808515402025,-2.38838701412431,4.67401962251165));
#20430=CARTESIAN_POINT('Ctrl Pts',(3.49482590830325,-2.21566016756178,4.66290583345484));
#20431=CARTESIAN_POINT('Ctrl Pts',(3.69783370147164,-2.21166166018595,4.65179204439804));
#20432=CARTESIAN_POINT('Ctrl Pts',(3.81129319817336,-2.38005137114376,4.64067825534124));
#20433=CARTESIAN_POINT('Ctrl Pts',(3.73135363435924,-2.56670028832692,4.62956446628443));
#20434=CARTESIAN_POINT('Ctrl Pts',(3.53118459936441,-2.60076654109381,4.61845067722763));
#20435=CARTESIAN_POINT('Ctrl Pts',(3.3940030809914,-2.45106890195169,4.60733688817082));
#20436=CARTESIAN_POINT('Ctrl Pts',(3.44537287875023,-2.25462731768926,4.59622309911402));
#20437=CARTESIAN_POINT('Ctrl Pts',(3.63827463418116,-2.1912469981906,4.58510931005721));
#20438=CARTESIAN_POINT('Ctrl Pts',(3.79614318287948,-2.31894066865531,4.57399552100041));
#20439=CARTESIAN_POINT('Ctrl Pts',(3.77447965187866,-2.52082886440086,4.56288173194361));
#20440=CARTESIAN_POINT('Ctrl Pts',(3.59311291676859,-2.6121210302163,4.55176794288681));
#20441=CARTESIAN_POINT('Ctrl Pts',(3.41805000706685,-2.50925641156176,4.54065415383));
#20442=CARTESIAN_POINT('Ctrl Pts',(3.40952798930647,-2.3063881601463,4.52954036477319));
#20443=CARTESIAN_POINT('Ctrl Pts',(3.57534716312072,-2.18920388779283,4.51842657571639));
#20444=CARTESIAN_POINT('Ctrl Pts',(3.76373135793792,-2.26496368670519,4.50731278665958));
#20445=CARTESIAN_POINT('Ctrl Pts',(3.80225038434475,-2.46432375625011,4.49619899760278));
#20446=CARTESIAN_POINT('Ctrl Pts',(3.65564733958441,-2.60480755889841,4.48508520854597));
#20447=CARTESIAN_POINT('Ctrl Pts',(3.45810965522258,-2.55782868685937,4.47397141948917));
#20448=CARTESIAN_POINT('Ctrl Pts',(3.39044580977021,-2.36638741452612,4.46285763043237));
#20449=CARTESIAN_POINT('Ctrl Pts',(3.51458929677089,-2.20571214952866,4.45174384137556));
#20450=CARTESIAN_POINT('Ctrl Pts',(3.71691015778721,-2.22287070405714,4.44063005231876));
#20451=CARTESIAN_POINT('Ctrl Pts',(3.81222184810419,-2.40215781884775,4.42951626326195));
#20452=CARTESIAN_POINT('Ctrl Pts',(3.71328442888611,-2.57946964350242,4.41840247420515));
#20453=CARTESIAN_POINT('Ctrl Pts',(3.51065657770066,-2.59251129681771,4.40728868514835));
#20454=CARTESIAN_POINT('Ctrl Pts',(3.38980559289267,-2.42934431849055,4.39617489609154));
#20455=CARTESIAN_POINT('Ctrl Pts',(3.46134829568354,-2.23931987168859,4.38506110703474));
#20456=CARTESIAN_POINT('Ctrl Pts',(3.65979974892982,-2.19636432620836,4.37394731797793));
#20457=CARTESIAN_POINT('Ctrl Pts',(3.80351726947246,-2.33980571567353,4.36283352892113));
#20458=CARTESIAN_POINT('Ctrl Pts',(3.76095021022585,-2.5383298122697,4.35171973986433));
#20459=CARTESIAN_POINT('Ctrl Pts',(3.57106943581066,-2.61026670575114,4.34060595080752));
#20460=CARTESIAN_POINT('Ctrl Pts',(3.4076574417421,-2.48968873955599,4.32949216175071));
#20461=CARTESIAN_POINT('Ctrl Pts',(3.42032223348093,-2.28712856948396,4.31837837269392));
#20462=CARTESIAN_POINT('Ctrl Pts',(3.59740050213728,-2.18765797570795,4.30726458363711));
#20463=CARTESIAN_POINT('Ctrl Pts',(3.77696058810632,-2.28300294170579,4.29615079458031));
#20464=CARTESIAN_POINT('Ctrl Pts',(3.78843875194939,-2.41723390733862,4.28874160187577));
#20465=CARTESIAN_POINT('Ctrl Pts',(3.76451707405898,-2.471939748488,4.2850370055235));
#20466=CARTESIAN_POINT('Ctrl Pts',(3.74664903694653,-2.2752733913429,5.2149629944765));
#20467=CARTESIAN_POINT('Ctrl Pts',(3.78812360169505,-2.32403768505403,5.21125839812423));
#20468=CARTESIAN_POINT('Ctrl Pts',(3.81784750611002,-2.46538960629943,5.20384920541969));
#20469=CARTESIAN_POINT('Ctrl Pts',(3.66299265426352,-2.61879586558741,5.19273541636289));
#20470=CARTESIAN_POINT('Ctrl Pts',(3.45044394556317,-2.57143545904423,5.18162162730609));
#20471=CARTESIAN_POINT('Ctrl Pts',(3.37480563557539,-2.36740181371937,5.17050783824928));
#20472=CARTESIAN_POINT('Ctrl Pts',(3.50528006828989,-2.19308453544296,5.15939404919248));
#20473=CARTESIAN_POINT('Ctrl Pts',(3.72245784285994,-2.20821977658425,5.14828026013567));
#20474=CARTESIAN_POINT('Ctrl Pts',(3.82754601013736,-2.39886344769606,5.13716647107887));
#20475=CARTESIAN_POINT('Ctrl Pts',(3.72436000974907,-2.59056249066898,5.12605268202206));
#20476=CARTESIAN_POINT('Ctrl Pts',(3.50734524491072,-2.60782999792249,5.11493889296526));
#20477=CARTESIAN_POINT('Ctrl Pts',(3.37513874637818,-2.43487210986008,5.10382510390845));
#20478=CARTESIAN_POINT('Ctrl Pts',(3.44875014448657,-2.22999350714877,5.09271131485166));
#20479=CARTESIAN_POINT('Ctrl Pts',(3.66080232998667,-2.18072471268405,5.08159752579485));
#20480=CARTESIAN_POINT('Ctrl Pts',(3.81720141367915,-2.33216060736901,5.07048373673804));
#20481=CARTESIAN_POINT('Ctrl Pts',(3.77479359998752,-2.54569090122825,5.05936994768124));
#20482=CARTESIAN_POINT('Ctrl Pts',(3.57239521205144,-2.62586854421817,5.04825615862443));
#20483=CARTESIAN_POINT('Ctrl Pts',(3.39526380451891,-2.49930620545266,5.03714236956763));
#20484=CARTESIAN_POINT('Ctrl Pts',(3.40552975611236,-2.28184774151832,5.02602858051083));
#20485=CARTESIAN_POINT('Ctrl Pts',(3.59379652860931,-2.17253539424633,5.01491479145402));
#20486=CARTESIAN_POINT('Ctrl Pts',(3.78774140820779,-2.27142397298568,5.00380100239722));
#20487=CARTESIAN_POINT('Ctrl Pts',(3.80984444804818,-2.48799965102756,4.99268721334042));
#20488=CARTESIAN_POINT('Ctrl Pts',(3.63987448463892,-2.62402824868975,4.98157342428361));
#20489=CARTESIAN_POINT('Ctrl Pts',(3.43340695330878,-2.55500125057707,4.9704596352268));
#20490=CARTESIAN_POINT('Ctrl Pts',(3.37942392687054,-2.34409984952602,4.95934584617001));
#20491=CARTESIAN_POINT('Ctrl Pts',(3.52733668168959,-2.18436449038006,4.94823205711319));
#20492=CARTESIAN_POINT('Ctrl Pts',(3.74175899580671,-2.22200275854966,4.9371182680564));
#20493=CARTESIAN_POINT('Ctrl Pts',(3.82642769341035,-2.42256392050098,4.92600447899958));
#20494=CARTESIAN_POINT('Ctrl Pts',(3.70384455536842,-2.60247207009742,4.91489068994279));
#20495=CARTESIAN_POINT('Ctrl Pts',(3.48621131812161,-2.59705523775825,4.90377690088598));
#20496=CARTESIAN_POINT('Ctrl Pts',(3.37273015184892,-2.41127151153357,4.89266311182918));
#20497=CARTESIAN_POINT('Ctrl Pts',(3.46727165500458,-2.21517084297807,4.88154932277238));
#20498=CARTESIAN_POINT('Ctrl Pts',(3.68330091757622,-2.1882463979482,4.87043553371556));
#20499=CARTESIAN_POINT('Ctrl Pts',(3.82308390559375,-2.3551424263264,4.85932174465877));
#20500=CARTESIAN_POINT('Ctrl Pts',(3.75867566487773,-2.56309710060709,4.84820795560196));
#20501=CARTESIAN_POINT('Ctrl Pts',(3.54902978859471,-2.62176714905541,4.83709416654515));
#20502=CARTESIAN_POINT('Ctrl Pts',(3.38603752485245,-2.47745121096268,4.82598037748835));
#20503=CARTESIAN_POINT('Ctrl Pts',(3.41888754111225,-2.26224330111939,4.81486658843154));
#20504=CARTESIAN_POINT('Ctrl Pts',(3.61751184494699,-2.17312566002871,4.80375279937474));
#20505=CARTESIAN_POINT('Ctrl Pts',(3.80010735850391,-2.29166867524379,4.79263901031795));
#20506=CARTESIAN_POINT('Ctrl Pts',(3.79954233745042,-2.50936858056899,4.78152522126113));
#20507=CARTESIAN_POINT('Ctrl Pts',(3.61633395196453,-2.62696218377534,4.77041143220433));
#20508=CARTESIAN_POINT('Ctrl Pts',(3.4181749150059,-2.53681472624589,4.75929764314752));
#20509=CARTESIAN_POINT('Ctrl Pts',(3.38644244037908,-2.32143919819905,4.74818385409072));
#20510=CARTESIAN_POINT('Ctrl Pts',(3.55018162198074,-2.1779712629807,4.73707006503392));
#20511=CARTESIAN_POINT('Ctrl Pts',(3.75952012996226,-2.23772874873326,4.72595627597711));
#20512=CARTESIAN_POINT('Ctrl Pts',(3.82284805390801,-2.44601495105141,4.71484248692031));
#20513=CARTESIAN_POINT('Ctrl Pts',(3.68220062684293,-2.61218314682717,4.7037286978635));
#20514=CARTESIAN_POINT('Ctrl Pts',(3.46631403381001,-2.58413770199147,4.69261490880671));
#20515=CARTESIAN_POINT('Ctrl Pts',(3.37279172173275,-2.38754893025942,4.68150111974989));
#20516=CARTESIAN_POINT('Ctrl Pts',(3.48723572347063,-2.20235676386561,4.6703873306931));
#20517=CARTESIAN_POINT('Ctrl Pts',(3.70489414634973,-2.19806969293246,4.65927354163628));
#20518=CARTESIAN_POINT('Ctrl Pts',(3.82654176749436,-2.37861172210345,4.64815975257949));
#20519=CARTESIAN_POINT('Ctrl Pts',(3.7408331396931,-2.57873068459315,4.63704596352267));
#20520=CARTESIAN_POINT('Ctrl Pts',(3.52621834197413,-2.61525542453006,4.62593217446588));
#20521=CARTESIAN_POINT('Ctrl Pts',(3.37913673258752,-2.45475443323377,4.61481838540907));
#20522=CARTESIAN_POINT('Ctrl Pts',(3.43421377662264,-2.24413608823767,4.60370459635227));
#20523=CARTESIAN_POINT('Ctrl Pts',(3.64103683106015,-2.17618174930149,4.59259080729546));
#20524=CARTESIAN_POINT('Ctrl Pts',(3.81029840863609,-2.31309079348749,4.58147701823866));
#20525=CARTESIAN_POINT('Ctrl Pts',(3.78707146784707,-2.52954882003939,4.57036322918186));
#20526=CARTESIAN_POINT('Ctrl Pts',(3.59261589099123,-2.62742934237049,4.55924944012505));
#20527=CARTESIAN_POINT('Ctrl Pts',(3.40491907287596,-2.51714120851626,4.54813565106824));
#20528=CARTESIAN_POINT('Ctrl Pts',(3.39578203967876,-2.29963239781408,4.53702186201144));
#20529=CARTESIAN_POINT('Ctrl Pts',(3.57356802164639,-2.17399119208196,4.52590807295464));
#20530=CARTESIAN_POINT('Ctrl Pts',(3.77554749297266,-2.2552184104638,4.51479428389784));
#20531=CARTESIAN_POINT('Ctrl Pts',(3.81684635351243,-2.46896586146052,4.50368049484103));
#20532=CARTESIAN_POINT('Ctrl Pts',(3.65966328672572,-2.61958807377691,4.49256670578423));
#20533=CARTESIAN_POINT('Ctrl Pts',(3.44786973847645,-2.56921883899499,4.48145291672742));
#20534=CARTESIAN_POINT('Ctrl Pts',(3.37532274086005,-2.36396166753528,4.47033912767061));
#20535=CARTESIAN_POINT('Ctrl Pts',(3.5084253925837,-2.19169081906581,4.45922533861382));
#20536=CARTESIAN_POINT('Ctrl Pts',(3.7253473089154,-2.21008766905501,4.44811154955701));
#20537=CARTESIAN_POINT('Ctrl Pts',(3.82753743606548,-2.40231354392819,4.43699776050021));
#20538=CARTESIAN_POINT('Ctrl Pts',(3.72145991906655,-2.59242157628407,4.4258839714434));
#20539=CARTESIAN_POINT('Ctrl Pts',(3.5042088577547,-2.60640441727771,4.41477018238659));
#20540=CARTESIAN_POINT('Ctrl Pts',(3.37463632092665,-2.43146203396151,4.4036563933298));
#20541=CARTESIAN_POINT('Ctrl Pts',(3.45134210455661,-2.22772393724184,4.39254260427299));
#20542=CARTESIAN_POINT('Ctrl Pts',(3.66411536639796,-2.18166838372235,4.38142881521618));
#20543=CARTESIAN_POINT('Ctrl Pts',(3.81820466697696,-2.33546162544623,4.37031502615938));
#20544=CARTESIAN_POINT('Ctrl Pts',(3.77256563589538,-2.54831277314961,4.35920123710258));
#20545=CARTESIAN_POINT('Ctrl Pts',(3.5689815800853,-2.62544119535262,4.34808744804577));
#20546=CARTESIAN_POINT('Ctrl Pts',(3.39377649877598,-2.49616138029528,4.33697365898897));
#20547=CARTESIAN_POINT('Ctrl Pts',(3.40735528091504,-2.27898288449522,4.32585986993216));
#20548=CARTESIAN_POINT('Ctrl Pts',(3.59721290204555,-2.17233371489326,4.31474608087536));
#20549=CARTESIAN_POINT('Ctrl Pts',(3.78973144783182,-2.27455951915752,4.30363229181856));
#20550=CARTESIAN_POINT('Ctrl Pts',(3.8020379657277,-2.4184776408473,4.29622309911402));
#20551=CARTESIAN_POINT('Ctrl Pts',(3.77638991251267,-2.47713148324917,4.29251850276175));
#20552=CARTESIAN_POINT('Ctrl Pts',(3.75652001142717,-2.26687801966678,5.22244449171475));
#20553=CARTESIAN_POINT('Ctrl Pts',(3.80078623699225,-2.31892464723302,5.21873989536248));
#20554=CARTESIAN_POINT('Ctrl Pts',(3.83251086304886,-2.46979099309691,5.21133070265794));
#20555=CARTESIAN_POINT('Ctrl Pts',(3.66723270176503,-2.63352305678248,5.20021691360114));
#20556=CARTESIAN_POINT('Ctrl Pts',(3.4403772991841,-2.58297481229563,5.18910312454433));
#20557=CARTESIAN_POINT('Ctrl Pts',(3.35964776021048,-2.3652076236204,5.17798933548753));
#20558=CARTESIAN_POINT('Ctrl Pts',(3.49890445172815,-2.1791570162937,5.16687554643073));
#20559=CARTESIAN_POINT('Ctrl Pts',(3.73070050348011,-2.19531101338576,5.15576175737392));
#20560=CARTESIAN_POINT('Ctrl Pts',(3.84286217522106,-2.398786946145,5.14464796831712));
#20561=CARTESIAN_POINT('Ctrl Pts',(3.73273070558319,-2.60338928804541,5.13353417926031));
#20562=CARTESIAN_POINT('Ctrl Pts',(3.50110863577888,-2.62181907448596,5.12242039020351));
#20563=CARTESIAN_POINT('Ctrl Pts',(3.36000329276455,-2.4372193581863,5.1113066011467));
#20564=CARTESIAN_POINT('Ctrl Pts',(3.4385694880359,-2.21855033788275,5.10019281208991));
#20565=CARTESIAN_POINT('Ctrl Pts',(3.66489494634582,-2.16596525152154,5.08907902303309));
#20566=CARTESIAN_POINT('Ctrl Pts',(3.83182128201397,-2.32759432498908,5.07796523397629));
#20567=CARTESIAN_POINT('Ctrl Pts',(3.78655899034249,-2.55549738341204,5.06685144491949));
#20568=CARTESIAN_POINT('Ctrl Pts',(3.57053712854092,-2.64107179875281,5.05573765586268));
#20569=CARTESIAN_POINT('Ctrl Pts',(3.38148297238433,-2.50599052496954,5.04462386680588));
#20570=CARTESIAN_POINT('Ctrl Pts',(3.3924399271259,-2.27389489059897,5.03351007774908));
#20571=CARTESIAN_POINT('Ctrl Pts',(3.59337897177386,-2.15722470850713,5.02239628869227));
#20572=CARTESIAN_POINT('Ctrl Pts',(3.8003783179889,-2.26276949623011,5.01128249963547));
#20573=CARTESIAN_POINT('Ctrl Pts',(3.82396911763155,-2.49392292422242,5.00016871057867));
#20574=CARTESIAN_POINT('Ctrl Pts',(3.64255844375993,-2.63910763258347,4.98905492152186));
#20575=CARTESIAN_POINT('Ctrl Pts',(3.42219354375095,-2.56543441414071,4.97794113246505));
#20576=CARTESIAN_POINT('Ctrl Pts',(3.3645769095683,-2.34033719979929,4.96682734340826));
#20577=CARTESIAN_POINT('Ctrl Pts',(3.52244569995759,-2.16985002334435,4.95571355435144));
#20578=CARTESIAN_POINT('Ctrl Pts',(3.75130082069111,-2.21002173048044,4.94459976529465));
#20579=CARTESIAN_POINT('Ctrl Pts',(3.84166858438312,-2.42408270226789,4.93348597623783));
#20580=CARTESIAN_POINT('Ctrl Pts',(3.71083435207858,-2.61610050352316,4.92237218718104));
#20581=CARTESIAN_POINT('Ctrl Pts',(3.47855218037073,-2.61031906317225,4.91125839812423));
#20582=CARTESIAN_POINT('Ctrl Pts',(3.35743257528088,-2.4120301991119,4.90014460906743));
#20583=CARTESIAN_POINT('Ctrl Pts',(3.45833768493844,-2.20272995737643,4.88903082001062));
#20584=CARTESIAN_POINT('Ctrl Pts',(3.68890791813162,-2.17399322284688,4.87791703095382));
#20585=CARTESIAN_POINT('Ctrl Pts',(3.83809972557463,-2.3521230545377,4.86680324189701));
#20586=CARTESIAN_POINT('Ctrl Pts',(3.76935615396461,-2.57407519737118,4.85568945284021));
#20587=CARTESIAN_POINT('Ctrl Pts',(3.54559897400137,-2.63669433790405,4.8445756637834));
#20588=CARTESIAN_POINT('Ctrl Pts',(3.37163567008428,-2.48266446665686,4.8334618747266));
#20589=CARTESIAN_POINT('Ctrl Pts',(3.40669682716669,-2.25297087159989,4.8223480856698));
#20590=CARTESIAN_POINT('Ctrl Pts',(3.61869057055051,-2.15785470519124,4.81123429661299));
#20591=CARTESIAN_POINT('Ctrl Pts',(3.81357662274397,-2.28437687323548,4.80012050755619));
#20592=CARTESIAN_POINT('Ctrl Pts',(3.81297357001622,-2.51673020046272,4.78900671849938));
#20593=CARTESIAN_POINT('Ctrl Pts',(3.61743339336808,-2.64223905139592,4.77789292944258));
#20594=CARTESIAN_POINT('Ctrl Pts',(3.405936234062,-2.54602375140875,4.76677914038577));
#20595=CARTESIAN_POINT('Ctrl Pts',(3.37206784055177,-2.31615125573517,4.75566535132898));
#20596=CARTESIAN_POINT('Ctrl Pts',(3.546828337511,-2.16302646659663,4.74455156227216));
#20597=CARTESIAN_POINT('Ctrl Pts',(3.77025746015408,-2.22680624004484,4.73343777321537));
#20598=CARTESIAN_POINT('Ctrl Pts',(3.83784799866721,-2.44911222613084,4.72232398415856));
#20599=CARTESIAN_POINT('Ctrl Pts',(3.68773356662048,-2.62646523466876,4.71121019510175));
#20600=CARTESIAN_POINT('Ctrl Pts',(3.4573156060797,-2.59653204562391,4.70009640604496));
#20601=CARTESIAN_POINT('Ctrl Pts',(3.35749828944527,-2.38671084639454,4.68898261698814));
#20602=CARTESIAN_POINT('Ctrl Pts',(3.47964553863801,-2.18905336016944,4.67786882793135));
#20603=CARTESIAN_POINT('Ctrl Pts',(3.71195459122784,-2.18447772567898,4.66675503887453));
#20604=CARTESIAN_POINT('Ctrl Pts',(3.84179033681535,-2.37717207306315,4.65564124981774));
#20605=CARTESIAN_POINT('Ctrl Pts',(3.75031264502696,-2.59076108085938,4.64452746076093));
#20606=CARTESIAN_POINT('Ctrl Pts',(3.52125208458385,-2.6297443079663,4.63341367170413));
#20607=CARTESIAN_POINT('Ctrl Pts',(3.36427038418365,-2.45843996451585,4.62229988264732));
#20608=CARTESIAN_POINT('Ctrl Pts',(3.42305467449503,-2.23364485878609,4.61118609359052));
#20609=CARTESIAN_POINT('Ctrl Pts',(3.64379902793915,-2.16111650041238,4.60007230453371));
#20610=CARTESIAN_POINT('Ctrl Pts',(3.82445363439269,-2.30724091831967,4.58895851547691));
#20611=CARTESIAN_POINT('Ctrl Pts',(3.79966328381548,-2.53826877567792,4.57784472642011));
#20612=CARTESIAN_POINT('Ctrl Pts',(3.59211886521387,-2.64273765452468,4.5667309373633));
#20613=CARTESIAN_POINT('Ctrl Pts',(3.39178813868507,-2.52502600547076,4.5556171483065));
#20614=CARTESIAN_POINT('Ctrl Pts',(3.38203609005104,-2.29287663548185,4.54450335924969));
#20615=CARTESIAN_POINT('Ctrl Pts',(3.57178888017207,-2.15877849637109,4.53338957019289));
#20616=CARTESIAN_POINT('Ctrl Pts',(3.78736362800739,-2.2454731342224,4.52227578113608));
#20617=CARTESIAN_POINT('Ctrl Pts',(3.83144232268012,-2.47360796667095,4.51116199207928));
#20618=CARTESIAN_POINT('Ctrl Pts',(3.66367923386702,-2.6343685886554,4.50004820302247));
#20619=CARTESIAN_POINT('Ctrl Pts',(3.43762982173032,-2.58060899113062,4.48893441396567));
#20620=CARTESIAN_POINT('Ctrl Pts',(3.36019967194989,-2.36153592054442,4.47782062490886));
#20621=CARTESIAN_POINT('Ctrl Pts',(3.50226148839652,-2.17766948860297,4.46670683585206));
#20622=CARTESIAN_POINT('Ctrl Pts',(3.73378446004359,-2.19730463405286,4.45559304679526));
#20623=CARTESIAN_POINT('Ctrl Pts',(3.84285302402677,-2.40246926900864,4.44447925773845));
#20624=CARTESIAN_POINT('Ctrl Pts',(3.72963540924699,-2.60537350906572,4.43336546868165));
#20625=CARTESIAN_POINT('Ctrl Pts',(3.49776113780875,-2.62029753773771,4.42225167962485));
#20626=CARTESIAN_POINT('Ctrl Pts',(3.35946704896063,-2.43357974943247,4.41113789056804));
#20627=CARTESIAN_POINT('Ctrl Pts',(3.44133591342967,-2.21612800279508,4.40002410151124));
#20628=CARTESIAN_POINT('Ctrl Pts',(3.66843098386609,-2.16697244123634,4.38891031245443));
#20629=CARTESIAN_POINT('Ctrl Pts',(3.83289206448147,-2.33111753521892,4.37779652339763));
#20630=CARTESIAN_POINT('Ctrl Pts',(3.7841810615649,-2.55829573402952,4.36668273434082));
#20631=CARTESIAN_POINT('Ctrl Pts',(3.56689372435994,-2.6406156849541,4.35556894528403));
#20632=CARTESIAN_POINT('Ctrl Pts',(3.37989555580985,-2.50263402103458,4.34445515622721));
#20633=CARTESIAN_POINT('Ctrl Pts',(3.39438832834916,-2.27083719950648,4.33334136717041));
#20634=CARTESIAN_POINT('Ctrl Pts',(3.59702530195382,-2.15700945407857,4.32222757811361));
#20635=CARTESIAN_POINT('Ctrl Pts',(3.80250230755732,-2.26611609660926,4.31111378905681));
#20636=CARTESIAN_POINT('Ctrl Pts',(3.81563717950601,-2.41972137435598,4.30370459635227));
#20637=CARTESIAN_POINT('Ctrl Pts',(3.78826275096636,-2.48232321801033,4.3));
#20638=CARTESIAN_POINT('Ctrl Pts',(3.72690708798524,-2.29206413469515,5.2));
#20639=CARTESIAN_POINT('Ctrl Pts',(3.73511889692415,-2.29972488088976,5.2));
#20640=CARTESIAN_POINT('Ctrl Pts',(3.74243606331987,-2.3082260358574,5.2));
#20641=CARTESIAN_POINT('Ctrl Pts',(3.74885415883116,-2.3173733937361,5.2));
#20642=CARTESIAN_POINT('Ctrl Pts',(3.75362492547366,-2.32417290455016,5.2));
#20643=CARTESIAN_POINT('Ctrl Pts',(3.75789857922842,-2.33133076203089,5.2));
#20644=CARTESIAN_POINT('Ctrl Pts',(3.7616631192462,-2.3387816278666,5.2));
#20645=CARTESIAN_POINT('Ctrl Pts',(3.76388041855661,-2.34317015863036,5.2));
#20646=CARTESIAN_POINT('Ctrl Pts',(3.76592248852987,-2.34766555277529,5.2));
#20647=CARTESIAN_POINT('Ctrl Pts',(3.76777441807103,-2.35222602465318,5.2));
#20648=CARTESIAN_POINT('Ctrl Pts',(3.77233274722043,-2.36345114495818,5.2));
#20649=CARTESIAN_POINT('Ctrl Pts',(3.77575806540191,-2.37509440908006,5.2));
#20650=CARTESIAN_POINT('Ctrl Pts',(3.77802228391775,-2.38695732035888,5.2));
#20651=CARTESIAN_POINT('Ctrl Pts',(3.77946116292117,-2.39449603353478,5.2));
#20652=CARTESIAN_POINT('Ctrl Pts',(3.78043041033378,-2.40212433051409,5.2));
#20653=CARTESIAN_POINT('Ctrl Pts',(3.78091325285907,-2.40979638894873,5.2));
#20654=CARTESIAN_POINT('Ctrl Pts',(3.78113857897669,-2.41337667662164,5.2));
#20655=CARTESIAN_POINT('Ctrl Pts',(3.78125743502661,-2.41696304534708,5.2));
#20656=CARTESIAN_POINT('Ctrl Pts',(3.78126867486757,-2.42054069500775,5.2));
#20657=CARTESIAN_POINT('Ctrl Pts',(3.78130372190818,-2.4316961938677,5.2));
#20658=CARTESIAN_POINT('Ctrl Pts',(3.78029682789473,-2.44279407568189,5.2));
#20659=CARTESIAN_POINT('Ctrl Pts',(3.77821427386403,-2.45369318996624,5.2));
#20660=CARTESIAN_POINT('Ctrl Pts',(3.77705389172366,-2.45976608765585,5.2));
#20661=CARTESIAN_POINT('Ctrl Pts',(3.77555901526444,-2.46577751393184,5.2));
#20662=CARTESIAN_POINT('Ctrl Pts',(3.77374837416276,-2.47171132791926,5.2));
#20663=CARTESIAN_POINT('Ctrl Pts',(3.77261573055045,-2.47542321566067,5.2));
#20664=CARTESIAN_POINT('Ctrl Pts',(3.77135887218697,-2.47910625090944,5.2));
#20665=CARTESIAN_POINT('Ctrl Pts',(3.76998349987259,-2.48275161867489,5.2));
#20666=CARTESIAN_POINT('Ctrl Pts',(3.76560171320323,-2.49436536406777,5.2));
#20667=CARTESIAN_POINT('Ctrl Pts',(3.76005261276,-2.50551619028979,5.2));
#20668=CARTESIAN_POINT('Ctrl Pts',(3.75350161664164,-2.51608155564839,5.2));
#20669=CARTESIAN_POINT('Ctrl Pts',(3.74916064083137,-2.52308262764107,5.2));
#20670=CARTESIAN_POINT('Ctrl Pts',(3.7443785440277,-2.5298267716061,5.2));
#20671=CARTESIAN_POINT('Ctrl Pts',(3.73919190918146,-2.53627611456138,5.2));
#20672=CARTESIAN_POINT('Ctrl Pts',(3.73648178297727,-2.53964603241007,5.2));
#20673=CARTESIAN_POINT('Ctrl Pts',(3.73365980796544,-2.54293677988309,5.2));
#20674=CARTESIAN_POINT('Ctrl Pts',(3.73073436285314,-2.54613815029323,5.2));
#20675=CARTESIAN_POINT('Ctrl Pts',(3.72446793550896,-2.55299562131278,5.2));
#20676=CARTESIAN_POINT('Ctrl Pts',(3.71775196798206,-2.55941733778444,5.2));
#20677=CARTESIAN_POINT('Ctrl Pts',(3.71064054370859,-2.56535254658103,5.2));
#20678=CARTESIAN_POINT('Ctrl Pts',(3.70611395375814,-2.56913044752735,5.2));
#20679=CARTESIAN_POINT('Ctrl Pts',(3.70142688925274,-2.57271116046832,5.2));
#20680=CARTESIAN_POINT('Ctrl Pts',(3.69659110235036,-2.57608017868915,5.2));
#20681=CARTESIAN_POINT('Ctrl Pts',(3.69251867261816,-2.57891737773199,5.2));
#20682=CARTESIAN_POINT('Ctrl Pts',(3.68834776817108,-2.58159940125718,5.2));
#20683=CARTESIAN_POINT('Ctrl Pts',(3.68408920348942,-2.58411662981112,5.2));
#20684=CARTESIAN_POINT('Ctrl Pts',(3.67536613625436,-2.58927281635833,5.2));
#20685=CARTESIAN_POINT('Ctrl Pts',(3.6662720325658,-2.59374119323572,5.2));
#20686=CARTESIAN_POINT('Ctrl Pts',(3.65686566045376,-2.59744798255001,5.2));
#20687=CARTESIAN_POINT('Ctrl Pts',(3.6556263522049,-2.59793635942042,5.2));
#20688=CARTESIAN_POINT('Ctrl Pts',(3.65438160822106,-2.59841149615413,5.2));
#20689=CARTESIAN_POINT('Ctrl Pts',(3.65313161981588,-2.59887345085171,5.2));
#20690=CARTESIAN_POINT('Ctrl Pts',(3.43326718206005,-2.40013003210005,5.08714803633902));
#20691=CARTESIAN_POINT('Ctrl Pts',(3.4331940296057,-2.4086546125631,5.08771939403667));
#20692=CARTESIAN_POINT('Ctrl Pts',(3.43379133726061,-2.41716890764345,5.08829075173431));
#20693=CARTESIAN_POINT('Ctrl Pts',(3.43509475583067,-2.42557369055115,5.08886210943196));
#20694=CARTESIAN_POINT('Ctrl Pts',(3.44354592346175,-2.48006902373693,5.09256670578423));
#20695=CARTESIAN_POINT('Ctrl Pts',(3.48168219331808,-2.52996043426623,5.0962713021365));
#20696=CARTESIAN_POINT('Ctrl Pts',(3.53205035406398,-2.55241564805098,5.09997589848876));
#20697=CARTESIAN_POINT('Ctrl Pts',(3.58241851480988,-2.57487086183573,5.10368049484103));
#20698=CARTESIAN_POINT('Ctrl Pts',(3.64501856644536,-2.56988987887593,5.1073850911933));
#20699=CARTESIAN_POINT('Ctrl Pts',(3.69120110257795,-2.53975064654304,5.11108968754557));
#20700=CARTESIAN_POINT('Ctrl Pts',(3.73738363871054,-2.50961141421015,5.11479428389783));
#20701=CARTESIAN_POINT('Ctrl Pts',(3.76714865934026,-2.45431393250417,5.1184988802501));
#20702=CARTESIAN_POINT('Ctrl Pts',(3.76687430993005,-2.39916866701502,5.12220347660237));
#20703=CARTESIAN_POINT('Ctrl Pts',(3.76659996051984,-2.34402340152587,5.12590807295464));
#20704=CARTESIAN_POINT('Ctrl Pts',(3.73628624106972,-2.28903035225355,5.12961266930691));
#20705=CARTESIAN_POINT('Ctrl Pts',(3.68980584464362,-2.2593508727441,5.13331726565917));
#20706=CARTESIAN_POINT('Ctrl Pts',(3.64332544821752,-2.22967139323465,5.13702186201144));
#20707=CARTESIAN_POINT('Ctrl Pts',(3.58067837481544,-2.22530548348806,5.14072645836371));
#20708=CARTESIAN_POINT('Ctrl Pts',(3.53053651892971,-2.24826429864408,5.14443105471598));
#20709=CARTESIAN_POINT('Ctrl Pts',(3.48039466304398,-2.27122311380009,5.14813565106825));
#20710=CARTESIAN_POINT('Ctrl Pts',(3.4427580246746,-2.3215066538587,5.15184024742052));
#20711=CARTESIAN_POINT('Ctrl Pts',(3.43484901415926,-2.37607618365869,5.15554484377278));
#20712=CARTESIAN_POINT('Ctrl Pts',(3.4337081191144,-2.3839479782439,5.15607924129486));
#20713=CARTESIAN_POINT('Ctrl Pts',(3.43318582039731,-2.39190895914184,5.15661363881694));
#20714=CARTESIAN_POINT('Ctrl Pts',(3.43325215766083,-2.39987843114813,5.15714803633902));
#20715=CARTESIAN_POINT('Ctrl Pts',(3.54698297828114,-2.59851743256717,5.2));
#20716=CARTESIAN_POINT('Ctrl Pts',(3.48097120902544,-2.58088801151799,5.19629540364773));
#20717=CARTESIAN_POINT('Ctrl Pts',(3.36906717021742,-2.4748477879482,5.1888862109432));
#20718=CARTESIAN_POINT('Ctrl Pts',(3.41187708350278,-2.24617201703375,5.17777242188639));
#20719=CARTESIAN_POINT('Ctrl Pts',(3.62721323091929,-2.15871475485289,5.16665863282959));
#20720=CARTESIAN_POINT('Ctrl Pts',(3.81747535364037,-2.29190664293025,5.15554484377279));
#20721=CARTESIAN_POINT('Ctrl Pts',(3.80876232171537,-2.52413791100821,5.14443105471598));
#20722=CARTESIAN_POINT('Ctrl Pts',(3.60892556988421,-2.64269428158759,5.13331726565918));
#20723=CARTESIAN_POINT('Ctrl Pts',(3.40093972078443,-2.539134825312,5.12220347660237));
#20724=CARTESIAN_POINT('Ctrl Pts',(3.37514572416652,-2.30821119768585,5.11108968754557));
#20725=CARTESIAN_POINT('Ctrl Pts',(3.55516853033383,-2.16130913937078,5.09997589848876));
#20726=CARTESIAN_POINT('Ctrl Pts',(3.77622352465696,-2.23288041708187,5.08886210943196));
#20727=CARTESIAN_POINT('Ctrl Pts',(3.83598040928192,-2.457419700552,5.07774832037515));
#20728=CARTESIAN_POINT('Ctrl Pts',(3.67974110927284,-2.62940130358481,5.06663453131835));
#20729=CARTESIAN_POINT('Ctrl Pts',(3.45051418720664,-2.59140968013522,5.05552074226155));
#20730=CARTESIAN_POINT('Ctrl Pts',(3.35811316524308,-2.37821841178234,5.04440695320474));
#20731=CARTESIAN_POINT('Ctrl Pts',(3.48711398605093,-2.18496417501817,5.03329316414794));
#20732=CARTESIAN_POINT('Ctrl Pts',(3.71944061581356,-2.18853461914439,5.02217937509113));
#20733=CARTESIAN_POINT('Ctrl Pts',(3.84244191526684,-2.38566174871763,5.01106558603433));
#20734=CARTESIAN_POINT('Ctrl Pts',(3.74353337026135,-2.59591283022398,4.99995179697752));
#20735=CARTESIAN_POINT('Ctrl Pts',(3.51324710863985,-2.62684268245385,4.98883800792072));
#20736=CARTESIAN_POINT('Ctrl Pts',(3.36236674984584,-2.4501408518507,4.97772421886391));
#20737=CARTESIAN_POINT('Ctrl Pts',(3.42899480110061,-2.22754453241715,4.96661042980712));
#20738=CARTESIAN_POINT('Ctrl Pts',(3.65214584962031,-2.16279865748873,4.9554966407503));
#20739=CARTESIAN_POINT('Ctrl Pts',(3.82756721091734,-2.31516586178242,4.94438285169351));
#20740=CARTESIAN_POINT('Ctrl Pts',(3.79469372311971,-2.54518271468373,4.9332690626367));
#20741=CARTESIAN_POINT('Ctrl Pts',(3.58361486265069,-2.64231218244471,4.9221552735799));
#20742=CARTESIAN_POINT('Ctrl Pts',(3.38753350417909,-2.51765056156021,4.91104148452309));
#20743=CARTESIAN_POINT('Ctrl Pts',(3.38592513888554,-2.28530204745491,4.89992769546629));
#20744=CARTESIAN_POINT('Ctrl Pts',(3.5802619217345,-2.1579378700657,4.88881390640948));
#20745=CARTESIAN_POINT('Ctrl Pts',(3.7926651914697,-2.25213590538246,4.87770011735268));
#20746=CARTESIAN_POINT('Ctrl Pts',(3.8287198264784,-2.48167562339262,4.86658632829587));
#20747=CARTESIAN_POINT('Ctrl Pts',(3.65542461045338,-2.63645671704841,4.85547253923907));
#20748=CARTESIAN_POINT('Ctrl Pts',(3.43139861992193,-2.5748062959875,4.84435875018227));
#20749=CARTESIAN_POINT('Ctrl Pts',(3.36169538464595,-2.35315368977137,4.83324496112546));
#20750=CARTESIAN_POINT('Ctrl Pts',(3.51011506636152,-2.17438004258061,4.82213117206865));
#20751=CARTESIAN_POINT('Ctrl Pts',(3.74080744720095,-2.20211890112026,4.81101738301186));
#20752=CARTESIAN_POINT('Ctrl Pts',(3.84261717475225,-2.41098057358878,4.79990359395505));
#20753=CARTESIAN_POINT('Ctrl Pts',(3.72235665078693,-2.60979160252334,4.78878980489825));
#20754=CARTESIAN_POINT('Ctrl Pts',(3.49010169673754,-2.61657799846968,4.77767601584144));
#20755=CARTESIAN_POINT('Ctrl Pts',(3.3584379059958,-2.42512809625518,4.76656222678464));
#20756=CARTESIAN_POINT('Ctrl Pts',(3.44787863939658,-2.21067816256631,4.75544843772783));
#20757=CARTESIAN_POINT('Ctrl Pts',(3.67655777933124,-2.16951665373617,4.74433464867103));
#20758=CARTESIAN_POINT('Ctrl Pts',(3.83516271561975,-2.33931916560024,4.73322085961422));
#20759=CARTESIAN_POINT('Ctrl Pts',(3.77852055137491,-2.56466353335787,4.72210707055742));
#20760=CARTESIAN_POINT('Ctrl Pts',(3.55847650189588,-2.63928950162157,4.71099328150062));
#20761=CARTESIAN_POINT('Ctrl Pts',(3.37643938114003,-2.49489107532353,4.69987949244381));
#20762=CARTESIAN_POINT('Ctrl Pts',(3.39902983017658,-2.26363777164387,4.68876570338701));
#20763=CARTESIAN_POINT('Ctrl Pts',(3.60557055480924,-2.15719836203143,4.6776519143302));
#20764=CARTESIAN_POINT('Ctrl Pts',(3.8070124874506,-2.27299804520947,4.6665381252734));
#20765=CARTESIAN_POINT('Ctrl Pts',(3.81897354264718,-2.50504405790744,4.65542433621659));
#20766=CARTESIAN_POINT('Ctrl Pts',(3.63050563092984,-2.64094205312202,4.64431054715979));
#20767=CARTESIAN_POINT('Ctrl Pts',(3.4141155692652,-2.55630305464544,4.63319675810298));
#20768=CARTESIAN_POINT('Ctrl Pts',(3.3678676351246,-2.32859809765437,4.62208296904619));
#20769=CARTESIAN_POINT('Ctrl Pts',(3.53409308711521,-2.16624811163355,4.61096917998937));
#20770=CARTESIAN_POINT('Ctrl Pts',(3.76064388390312,-2.21785387995996,4.59985539093258));
#20771=CARTESIAN_POINT('Ctrl Pts',(3.8401555119317,-2.4361800576391,4.58874160187577));
#20772=CARTESIAN_POINT('Ctrl Pts',(3.69985007633495,-2.62139021824623,4.57762781281896));
#20773=CARTESIAN_POINT('Ctrl Pts',(3.46815073350293,-2.60395940136712,4.56651402376216));
#20774=CARTESIAN_POINT('Ctrl Pts',(3.35713451954606,-2.39984223133897,4.55540023470536));
#20775=CARTESIAN_POINT('Ctrl Pts',(3.46841583417461,-2.19586946879708,4.54428644564855));
#20776=CARTESIAN_POINT('Ctrl Pts',(3.70013762796088,-2.17873969637961,4.53317265659175));
#20777=CARTESIAN_POINT('Ctrl Pts',(3.84020231541317,-2.36413198929513,4.52205886753494));
#20778=CARTESIAN_POINT('Ctrl Pts',(3.7604070991348,-2.58235467884591,4.51094507847814));
#20779=CARTESIAN_POINT('Ctrl Pts',(3.53378944658573,-2.63366606347461,4.49983128942134));
#20780=CARTESIAN_POINT('Ctrl Pts',(3.36777506303883,-2.47110024891367,4.48871750036453));
#20781=CARTESIAN_POINT('Ctrl Pts',(3.41431880073856,-2.24345557286895,4.47760371130772));
#20782=CARTESIAN_POINT('Ctrl Pts',(3.63081864021225,-2.15909778094929,4.46648992225093));
#20783=CARTESIAN_POINT('Ctrl Pts',(3.81910984016012,-2.29524053287965,4.45537613319411));
#20784=CARTESIAN_POINT('Ctrl Pts',(3.80684729577664,-2.52727079162485,4.44426234413733));
#20785=CARTESIAN_POINT('Ctrl Pts',(3.60525512132335,-2.64280869447754,4.4331485550805));
#20786=CARTESIAN_POINT('Ctrl Pts',(3.39885278350865,-2.53610095948868,4.42203476602371));
#20787=CARTESIAN_POINT('Ctrl Pts',(3.37656295673162,-2.30481864526098,4.4109209769669));
#20788=CARTESIAN_POINT('Ctrl Pts',(3.55878722400007,-2.16065655916503,4.3998071879101));
#20789=CARTESIAN_POINT('Ctrl Pts',(3.77873474447839,-2.23556893008468,4.38869339885329));
#20790=CARTESIAN_POINT('Ctrl Pts',(3.83508286096032,-2.4609855401145,4.37757960979649));
#20791=CARTESIAN_POINT('Ctrl Pts',(3.67625990251943,-2.63058416437082,4.36646582073969));
#20792=CARTESIAN_POINT('Ctrl Pts',(3.44762951704948,-2.58912094093836,4.35535203168288));
#20793=CARTESIAN_POINT('Ctrl Pts',(3.35847732135144,-2.37456428079453,4.34423824262607));
#20794=CARTESIAN_POINT('Ctrl Pts',(3.49037003077072,-2.18326698967564,4.33312445356928));
#20795=CARTESIAN_POINT('Ctrl Pts',(3.72265543153543,-2.19039239422561,4.32201066451247));
#20796=CARTESIAN_POINT('Ctrl Pts',(3.84257847294968,-2.38928487404799,4.31089687545567));
#20797=CARTESIAN_POINT('Ctrl Pts',(3.74065691978671,-2.59816384879942,4.29978308639886));
#20798=CARTESIAN_POINT('Ctrl Pts',(3.50959628368763,-2.62529831625878,4.28866929734206));
#20799=CARTESIAN_POINT('Ctrl Pts',(3.41142456563631,-2.50643134569449,4.28126010463752));
#20800=CARTESIAN_POINT('Ctrl Pts',(3.39833241385534,-2.439372075429,4.27755550828525));
#20801=CARTESIAN_POINT('Ctrl Pts',(3.55032651029123,-2.58599788000028,5.20748149723825));
#20802=CARTESIAN_POINT('Ctrl Pts',(3.48847779011663,-2.5694802628904,5.20377690088598));
#20803=CARTESIAN_POINT('Ctrl Pts',(3.38363100808545,-2.4701274930924,5.19636770818144));
#20804=CARTESIAN_POINT('Ctrl Pts',(3.42374110325997,-2.25587321805223,5.18525391912464));
#20805=CARTESIAN_POINT('Ctrl Pts',(3.62549702156375,-2.17393147043888,5.17414013006783));
#20806=CARTESIAN_POINT('Ctrl Pts',(3.80376021494099,-2.29872357809039,5.16302634101103));
#20807=CARTESIAN_POINT('Ctrl Pts',(3.79559667259879,-2.51630912195772,5.15191255195423));
#20808=CARTESIAN_POINT('Ctrl Pts',(3.60836267654075,-2.62738870475875,5.14079876289742));
#20809=CARTESIAN_POINT('Ctrl Pts',(3.41349350811379,-2.53036025203219,5.12968497384062));
#20810=CARTESIAN_POINT('Ctrl Pts',(3.38932621647788,-2.31399988193773,5.11857118478382));
#20811=CARTESIAN_POINT('Ctrl Pts',(3.55799583841393,-2.17636223943479,5.10745739572701));
#20812=CARTESIAN_POINT('Ctrl Pts',(3.76510994308412,-2.24341985624469,5.09634360667021));
#20813=CARTESIAN_POINT('Ctrl Pts',(3.8210982445241,-2.45379851247728,5.0852298176134));
#20814=CARTESIAN_POINT('Ctrl Pts',(3.67471221585842,-2.61493405180745,5.0741160285566));
#20815=CARTESIAN_POINT('Ctrl Pts',(3.4599415481546,-2.57933837979007,5.0630022394998));
#20816=CARTESIAN_POINT('Ctrl Pts',(3.3733678202314,-2.37959207320419,5.05188845044299));
#20817=CARTESIAN_POINT('Ctrl Pts',(3.49423317134075,-2.19852546421989,5.04077466138618));
#20818=CARTESIAN_POINT('Ctrl Pts',(3.71190806288376,-2.20187073737575,5.02966087232939));
#20819=CARTESIAN_POINT('Ctrl Pts',(3.82715225398445,-2.38656599419535,5.01854708327258));
#20820=CARTESIAN_POINT('Ctrl Pts',(3.73448140162136,-2.58355753756882,5.00743329421578));
#20821=CARTESIAN_POINT('Ctrl Pts',(3.51871820188173,-2.61253679077134,4.99631950515897));
#20822=CARTESIAN_POINT('Ctrl Pts',(3.37735315143523,-2.44697870622763,4.98520571610217));
#20823=CARTESIAN_POINT('Ctrl Pts',(3.4397792876273,-2.23842048050862,4.97409192704536));
#20824=CARTESIAN_POINT('Ctrl Pts',(3.64885725830102,-2.17775782071235,4.96297813798855));
#20825=CARTESIAN_POINT('Ctrl Pts',(3.81321562666231,-2.3205159483675,4.95186434893175));
#20826=CARTESIAN_POINT('Ctrl Pts',(3.78241531376532,-2.53602672971665,4.94075055987495));
#20827=CARTESIAN_POINT('Ctrl Pts',(3.5846481955208,-2.62703070279587,4.92963677081815));
#20828=CARTESIAN_POINT('Ctrl Pts',(3.40093275798132,-2.51023089885891,4.91852298176134));
#20829=CARTESIAN_POINT('Ctrl Pts',(3.39942582465563,-2.29253550311487,4.90740919270454));
#20830=CARTESIAN_POINT('Ctrl Pts',(3.5815067086795,-2.17320358008914,4.89629540364773));
#20831=CARTESIAN_POINT('Ctrl Pts',(3.78051471198171,-2.26146099225962,4.88518161459093));
#20832=CARTESIAN_POINT('Ctrl Pts',(3.81429555222874,-2.47652472935135,4.87406782553412));
#20833=CARTESIAN_POINT('Ctrl Pts',(3.65192924324508,-2.6215445138197,4.86295403647732));
#20834=CARTESIAN_POINT('Ctrl Pts',(3.44203150900096,-2.56378209230252,4.85184024742051));
#20835=CARTESIAN_POINT('Ctrl Pts',(3.37672412605308,-2.35610806428593,4.84072645836371));
#20836=CARTESIAN_POINT('Ctrl Pts',(3.5157836826493,-2.18860882279666,4.8296126693069));
#20837=CARTESIAN_POINT('Ctrl Pts',(3.73192738959469,-2.2145983231407,4.8184988802501));
#20838=CARTESIAN_POINT('Ctrl Pts',(3.82731646068567,-2.41028808091203,4.8073850911933));
#20839=CARTESIAN_POINT('Ctrl Pts',(3.71464019736706,-2.59656104154983,4.79627130213649));
#20840=CARTESIAN_POINT('Ctrl Pts',(3.49703246129012,-2.60291945170324,4.78515751307969));
#20841=CARTESIAN_POINT('Ctrl Pts',(3.37367208112564,-2.42354338644957,4.77404372402289));
#20842=CARTESIAN_POINT('Ctrl Pts',(3.45747221184004,-2.22261779257846,4.76292993496608));
#20843=CARTESIAN_POINT('Ctrl Pts',(3.6717296434323,-2.18405214481133,4.75181614590928));
#20844=CARTESIAN_POINT('Ctrl Pts',(3.8203321189215,-2.34314601791364,4.74070235685247));
#20845=CARTESIAN_POINT('Ctrl Pts',(3.76726210722566,-2.55427898558761,4.72958856779567));
#20846=CARTESIAN_POINT('Ctrl Pts',(3.56109519190488,-2.62419864811054,4.71847477873887));
#20847=CARTESIAN_POINT('Ctrl Pts',(3.39053828864408,-2.4889067454323,4.70736098968206));
#20848=CARTESIAN_POINT('Ctrl Pts',(3.41170406524473,-2.2722374903888,4.69624720062525));
#20849=CARTESIAN_POINT('Ctrl Pts',(3.60521924634802,-2.17251070931785,4.68513341156845));
#20850=CARTESIAN_POINT('Ctrl Pts',(3.79395719207867,-2.28100745591228,4.67401962251165));
#20851=CARTESIAN_POINT('Ctrl Pts',(3.80516392027559,-2.49841942757747,4.66290583345484));
#20852=CARTESIAN_POINT('Ctrl Pts',(3.62858178552708,-2.6257469810287,4.65179204439804));
#20853=CARTESIAN_POINT('Ctrl Pts',(3.4258384183463,-2.54644576259963,4.64067825534124));
#20854=CARTESIAN_POINT('Ctrl Pts',(3.3825071219795,-2.3331010768549,4.62956446628443));
#20855=CARTESIAN_POINT('Ctrl Pts',(3.53824952340251,-2.18098973415088,4.61845067722763));
#20856=CARTESIAN_POINT('Ctrl Pts',(3.75051283635195,-2.22934097152269,4.60733688817082));
#20857=CARTESIAN_POINT('Ctrl Pts',(3.82501004325936,-2.43389835306723,4.59622309911402));
#20858=CARTESIAN_POINT('Ctrl Pts',(3.69355300577889,-2.607428187611,4.58510931005722));
#20859=CARTESIAN_POINT('Ctrl Pts',(3.47646584115605,-2.59109664964851,4.57399552100041));
#20860=CARTESIAN_POINT('Ctrl Pts',(3.37245089307511,-2.39985218105986,4.56288173194361));
#20861=CARTESIAN_POINT('Ctrl Pts',(3.47671422318619,-2.20874301286248,4.5517679428868));
#20862=CARTESIAN_POINT('Ctrl Pts',(3.69382242288812,-2.1926935339158,4.54065415383));
#20863=CARTESIAN_POINT('Ctrl Pts',(3.82505389506733,-2.36639401454743,4.52954036477319));
#20864=CARTESIAN_POINT('Ctrl Pts',(3.75029098447549,-2.57085443446884,4.51842657571639));
#20865=CARTESIAN_POINT('Ctrl Pts',(3.53796503204054,-2.61892985352599,4.50731278665959));
#20866=CARTESIAN_POINT('Ctrl Pts',(3.38242038797595,-2.46661629356384,4.49619899760278));
#20867=CARTESIAN_POINT('Ctrl Pts',(3.42602883297491,-2.25332808713219,4.48508520854598));
#20868=CARTESIAN_POINT('Ctrl Pts',(3.62887505479918,-2.17429034089672,4.47397141948917));
#20869=CARTESIAN_POINT('Ctrl Pts',(3.80529162215107,-2.30184721541898,4.46285763043237));
#20870=CARTESIAN_POINT('Ctrl Pts',(3.7938024182598,-2.51924442665844,4.45174384137557));
#20871=CARTESIAN_POINT('Ctrl Pts',(3.60492370575545,-2.62749590217058,4.44063005231876));
#20872=CARTESIAN_POINT('Ctrl Pts',(3.41153818407012,-2.52751771773158,4.42951626326196));
#20873=CARTESIAN_POINT('Ctrl Pts',(3.39065407090943,-2.31082128169766,4.41840247420515));
#20874=CARTESIAN_POINT('Ctrl Pts',(3.56138631824024,-2.17575081436632,4.40728868514835));
#20875=CARTESIAN_POINT('Ctrl Pts',(3.76746279218639,-2.24593881748859,4.39617489609154));
#20876=CARTESIAN_POINT('Ctrl Pts',(3.82025730031655,-2.4571394714574,4.38506110703474));
#20877=CARTESIAN_POINT('Ctrl Pts',(3.67145055229768,-2.61604231517601,4.37394731797793));
#20878=CARTESIAN_POINT('Ctrl Pts',(3.45723880045736,-2.57719398051498,4.36283352892113));
#20879=CARTESIAN_POINT('Ctrl Pts',(3.37370901074182,-2.37616839092003,4.35171973986433));
#20880=CARTESIAN_POINT('Ctrl Pts',(3.49728387276899,-2.19693531230428,4.34060595080752));
#20881=CARTESIAN_POINT('Ctrl Pts',(3.71492013543138,-2.20361135139717,4.32949216175072));
#20882=CARTESIAN_POINT('Ctrl Pts',(3.82728019962215,-2.38996062620176,4.31837837269391));
#20883=CARTESIAN_POINT('Ctrl Pts',(3.73178635523027,-2.58566659508311,4.30726458363711));
#20884=CARTESIAN_POINT('Ctrl Pts',(3.51529761713718,-2.61108982042464,4.29615079458031));
#20885=CARTESIAN_POINT('Ctrl Pts',(3.42331712354828,-2.49971922570605,4.28874160187577));
#20886=CARTESIAN_POINT('Ctrl Pts',(3.41105063166184,-2.43688906544027,4.2850370055235));
#20887=CARTESIAN_POINT('Ctrl Pts',(3.55367004230132,-2.57347832743338,5.2149629944765));
#20888=CARTESIAN_POINT('Ctrl Pts',(3.49598437120782,-2.55807251426281,5.21125839812423));
#20889=CARTESIAN_POINT('Ctrl Pts',(3.39819484595347,-2.4654071982366,5.2038492054197));
#20890=CARTESIAN_POINT('Ctrl Pts',(3.43560512301717,-2.2655744190707,5.19273541636288));
#20891=CARTESIAN_POINT('Ctrl Pts',(3.62378081220822,-2.18914818602487,5.18162162730609));
#20892=CARTESIAN_POINT('Ctrl Pts',(3.7900450762416,-2.30554051325052,5.17050783824928));
#20893=CARTESIAN_POINT('Ctrl Pts',(3.78243102348222,-2.50848033290724,5.15939404919248));
#20894=CARTESIAN_POINT('Ctrl Pts',(3.60779978319727,-2.6120831279299,5.14828026013567));
#20895=CARTESIAN_POINT('Ctrl Pts',(3.42604729544316,-2.52158567875239,5.13716647107887));
#20896=CARTESIAN_POINT('Ctrl Pts',(3.40350670878923,-2.3197885661896,5.12605268202206));
#20897=CARTESIAN_POINT('Ctrl Pts',(3.56082314649402,-2.19141533949881,5.11493889296526));
#20898=CARTESIAN_POINT('Ctrl Pts',(3.75399636151128,-2.25395929540751,5.10382510390846));
#20899=CARTESIAN_POINT('Ctrl Pts',(3.80621607976629,-2.45017732440257,5.09271131485166));
#20900=CARTESIAN_POINT('Ctrl Pts',(3.66968332244401,-2.60046680003009,5.08159752579485));
#20901=CARTESIAN_POINT('Ctrl Pts',(3.46936890910255,-2.56726707944493,5.07048373673804));
#20902=CARTESIAN_POINT('Ctrl Pts',(3.38862247521972,-2.38096573462603,5.05936994768124));
#20903=CARTESIAN_POINT('Ctrl Pts',(3.50135235663055,-2.21208675342161,5.04825615862443));
#20904=CARTESIAN_POINT('Ctrl Pts',(3.70437550995396,-2.2152068556071,5.03714236956763));
#20905=CARTESIAN_POINT('Ctrl Pts',(3.81186259270206,-2.38747023967307,5.02602858051083));
#20906=CARTESIAN_POINT('Ctrl Pts',(3.72542943298136,-2.57120224491366,5.01491479145402));
#20907=CARTESIAN_POINT('Ctrl Pts',(3.52418929512361,-2.59823089908883,5.00380100239722));
#20908=CARTESIAN_POINT('Ctrl Pts',(3.39233955302463,-2.44381656060457,4.99268721334042));
#20909=CARTESIAN_POINT('Ctrl Pts',(3.45056377415398,-2.24929642860009,4.98157342428361));
#20910=CARTESIAN_POINT('Ctrl Pts',(3.64556866698174,-2.19271698393598,4.97045963522681));
#20911=CARTESIAN_POINT('Ctrl Pts',(3.79886404240727,-2.32586603495258,4.95934584617));
#20912=CARTESIAN_POINT('Ctrl Pts',(3.77013690441093,-2.52687074474958,4.9482320571132));
#20913=CARTESIAN_POINT('Ctrl Pts',(3.58568152839091,-2.61174922314702,4.93711826805639));
#20914=CARTESIAN_POINT('Ctrl Pts',(3.41433201178354,-2.5028112361576,4.92600447899959));
#20915=CARTESIAN_POINT('Ctrl Pts',(3.41292651042572,-2.29976895877483,4.91489068994279));
#20916=CARTESIAN_POINT('Ctrl Pts',(3.58275149562449,-2.18846929011257,4.90377690088598));
#20917=CARTESIAN_POINT('Ctrl Pts',(3.76836423249372,-2.27078607913679,4.89266311182918));
#20918=CARTESIAN_POINT('Ctrl Pts',(3.79987127797908,-2.47137383531008,4.88154932277237));
#20919=CARTESIAN_POINT('Ctrl Pts',(3.64843387603678,-2.60663231059099,4.87043553371557));
#20920=CARTESIAN_POINT('Ctrl Pts',(3.45266439807998,-2.55275788861754,4.85932174465877));
#20921=CARTESIAN_POINT('Ctrl Pts',(3.39175286746021,-2.35906243880049,4.84820795560196));
#20922=CARTESIAN_POINT('Ctrl Pts',(3.52145229893708,-2.20283760301271,4.83709416654516));
#20923=CARTESIAN_POINT('Ctrl Pts',(3.72304733198844,-2.22707774516114,4.82598037748835));
#20924=CARTESIAN_POINT('Ctrl Pts',(3.81201574661908,-2.40959558823528,4.81486658843155));
#20925=CARTESIAN_POINT('Ctrl Pts',(3.7069237439472,-2.58333048057632,4.80375279937474));
#20926=CARTESIAN_POINT('Ctrl Pts',(3.50396322584271,-2.58926090493679,4.79263901031794));
#20927=CARTESIAN_POINT('Ctrl Pts',(3.38890625625548,-2.42195867664397,4.78152522126113));
#20928=CARTESIAN_POINT('Ctrl Pts',(3.46706578428349,-2.2345574225906,4.77041143220433));
#20929=CARTESIAN_POINT('Ctrl Pts',(3.66690150753336,-2.19858763588649,4.75929764314752));
#20930=CARTESIAN_POINT('Ctrl Pts',(3.80550152222325,-2.34697287022705,4.74818385409073));
#20931=CARTESIAN_POINT('Ctrl Pts',(3.75600366307642,-2.54389443781734,4.73707006503391));
#20932=CARTESIAN_POINT('Ctrl Pts',(3.56371388191388,-2.60910779459951,4.72595627597711));
#20933=CARTESIAN_POINT('Ctrl Pts',(3.40463719614813,-2.48292241554106,4.71484248692031));
#20934=CARTESIAN_POINT('Ctrl Pts',(3.42437830031288,-2.28083720913373,4.7037286978635));
#20935=CARTESIAN_POINT('Ctrl Pts',(3.60486793788679,-2.18782305660426,4.6926149088067));
#20936=CARTESIAN_POINT('Ctrl Pts',(3.78090189670674,-2.28901686661509,4.6815011197499));
#20937=CARTESIAN_POINT('Ctrl Pts',(3.79135429790399,-2.4917947972475,4.67038733069309));
#20938=CARTESIAN_POINT('Ctrl Pts',(3.62665794012432,-2.6105519089354,4.65927354163629));
#20939=CARTESIAN_POINT('Ctrl Pts',(3.43756126742739,-2.53658847055381,4.64815975257948));
#20940=CARTESIAN_POINT('Ctrl Pts',(3.3971466088344,-2.33760405605543,4.63704596352268));
#20941=CARTESIAN_POINT('Ctrl Pts',(3.54240595968981,-2.19573135666821,4.62593217446587));
#20942=CARTESIAN_POINT('Ctrl Pts',(3.74038178880077,-2.24082806308542,4.61481838540907));
#20943=CARTESIAN_POINT('Ctrl Pts',(3.80986457458702,-2.43161664849535,4.60370459635227));
#20944=CARTESIAN_POINT('Ctrl Pts',(3.68725593522283,-2.59346615697577,4.59259080729546));
#20945=CARTESIAN_POINT('Ctrl Pts',(3.48478094880917,-2.57823389792989,4.58147701823866));
#20946=CARTESIAN_POINT('Ctrl Pts',(3.38776726660417,-2.39986213078074,4.57036322918185));
#20947=CARTESIAN_POINT('Ctrl Pts',(3.48501261219776,-2.22161655692788,4.55924944012505));
#20948=CARTESIAN_POINT('Ctrl Pts',(3.68750721781536,-2.20664737145198,4.54813565106824));
#20949=CARTESIAN_POINT('Ctrl Pts',(3.80990547472148,-2.36865603979974,4.53702186201144));
#20950=CARTESIAN_POINT('Ctrl Pts',(3.74017486981618,-2.55935419009178,4.52590807295464));
#20951=CARTESIAN_POINT('Ctrl Pts',(3.54214061749534,-2.60419364357738,4.51479428389783));
#20952=CARTESIAN_POINT('Ctrl Pts',(3.39706571291307,-2.46213233821401,4.50368049484103));
#20953=CARTESIAN_POINT('Ctrl Pts',(3.43773886521125,-2.26320060139544,4.49256670578422));
#20954=CARTESIAN_POINT('Ctrl Pts',(3.62693146938611,-2.18948290084415,4.48145291672742));
#20955=CARTESIAN_POINT('Ctrl Pts',(3.79147340414203,-2.30845389795831,4.47033912767061));
#20956=CARTESIAN_POINT('Ctrl Pts',(3.78075754074296,-2.51121806169204,4.45922533861382));
#20957=CARTESIAN_POINT('Ctrl Pts',(3.60459229018754,-2.61218310986363,4.44811154955701));
#20958=CARTESIAN_POINT('Ctrl Pts',(3.42422358463158,-2.51893447597448,4.4369977605002));
#20959=CARTESIAN_POINT('Ctrl Pts',(3.40474518508724,-2.31682391813433,4.4258839714434));
#20960=CARTESIAN_POINT('Ctrl Pts',(3.56398541248042,-2.19084506956762,4.41477018238659));
#20961=CARTESIAN_POINT('Ctrl Pts',(3.75619083989438,-2.25630870489251,4.40365639332979));
#20962=CARTESIAN_POINT('Ctrl Pts',(3.80543173967279,-2.4532934028003,4.39254260427299));
#20963=CARTESIAN_POINT('Ctrl Pts',(3.66664120207593,-2.60150046598119,4.38142881521619));
#20964=CARTESIAN_POINT('Ctrl Pts',(3.46684808386524,-2.5652670200916,4.37031502615938));
#20965=CARTESIAN_POINT('Ctrl Pts',(3.3889407001322,-2.37777250104553,4.35920123710258));
#20966=CARTESIAN_POINT('Ctrl Pts',(3.50419771476727,-2.21060363493292,4.34808744804577));
#20967=CARTESIAN_POINT('Ctrl Pts',(3.70718483932733,-2.21683030856873,4.33697365898897));
#20968=CARTESIAN_POINT('Ctrl Pts',(3.81198192629463,-2.39063637835552,4.32585986993216));
#20969=CARTESIAN_POINT('Ctrl Pts',(3.72291579067381,-2.5731693413668,4.31474608087536));
#20970=CARTESIAN_POINT('Ctrl Pts',(3.52099895058674,-2.5968813245905,4.30363229181856));
#20971=CARTESIAN_POINT('Ctrl Pts',(3.43520968146025,-2.49300710571762,4.29622309911402));
#20972=CARTESIAN_POINT('Ctrl Pts',(3.42376884946835,-2.43440605545154,4.29251850276175));
#20973=CARTESIAN_POINT('Ctrl Pts',(3.55701357431141,-2.56095877486649,5.22244449171475));
#20974=CARTESIAN_POINT('Ctrl Pts',(3.50349095229901,-2.54666476563522,5.21873989536248));
#20975=CARTESIAN_POINT('Ctrl Pts',(3.41275868382149,-2.4606869033808,5.21133070265794));
#20976=CARTESIAN_POINT('Ctrl Pts',(3.44746914277437,-2.27527562008917,5.20021691360114));
#20977=CARTESIAN_POINT('Ctrl Pts',(3.62206460285268,-2.20436490161086,5.18910312454433));
#20978=CARTESIAN_POINT('Ctrl Pts',(3.77632993754221,-2.31235744841065,5.17798933548754));
#20979=CARTESIAN_POINT('Ctrl Pts',(3.76926537436564,-2.50065154385676,5.16687554643072));
#20980=CARTESIAN_POINT('Ctrl Pts',(3.6072368898538,-2.59677755110107,5.15576175737393));
#20981=CARTESIAN_POINT('Ctrl Pts',(3.43860108277253,-2.51281110547259,5.14464796831712));
#20982=CARTESIAN_POINT('Ctrl Pts',(3.41768720110058,-2.32557725044148,5.13353417926032));
#20983=CARTESIAN_POINT('Ctrl Pts',(3.56365045457412,-2.20646843956283,5.12242039020351));
#20984=CARTESIAN_POINT('Ctrl Pts',(3.74288277993844,-2.26449873457034,5.11130660114671));
#20985=CARTESIAN_POINT('Ctrl Pts',(3.79133391500848,-2.44655613632785,5.1001928120899));
#20986=CARTESIAN_POINT('Ctrl Pts',(3.66465442902959,-2.58599954825273,5.0890790230331));
#20987=CARTESIAN_POINT('Ctrl Pts',(3.4787962700505,-2.55519577909978,5.0779652339763));
#20988=CARTESIAN_POINT('Ctrl Pts',(3.40387713020803,-2.38233939604788,5.06685144491948));
#20989=CARTESIAN_POINT('Ctrl Pts',(3.50847154192036,-2.22564804262333,5.05573765586269));
#20990=CARTESIAN_POINT('Ctrl Pts',(3.69684295702416,-2.22854297383845,5.04462386680588));
#20991=CARTESIAN_POINT('Ctrl Pts',(3.79657293141967,-2.38837448515078,5.03351007774908));
#20992=CARTESIAN_POINT('Ctrl Pts',(3.71637746434136,-2.5588469522585,5.02239628869228));
#20993=CARTESIAN_POINT('Ctrl Pts',(3.52966038836549,-2.58392500740631,5.01128249963547));
#20994=CARTESIAN_POINT('Ctrl Pts',(3.40732595461402,-2.44065441498151,5.00016871057866));
#20995=CARTESIAN_POINT('Ctrl Pts',(3.46134826068067,-2.26017237669156,4.98905492152187));
#20996=CARTESIAN_POINT('Ctrl Pts',(3.64228007566245,-2.20767614715961,4.97794113246505));
#20997=CARTESIAN_POINT('Ctrl Pts',(3.78451245815223,-2.33121612153766,4.96682734340826));
#20998=CARTESIAN_POINT('Ctrl Pts',(3.75785849505654,-2.5177147597825,4.95571355435145));
#20999=CARTESIAN_POINT('Ctrl Pts',(3.58671486126101,-2.59646774349818,4.94459976529464));
#21000=CARTESIAN_POINT('Ctrl Pts',(3.42773126558577,-2.49539157345629,4.93348597623784));
#21001=CARTESIAN_POINT('Ctrl Pts',(3.4264271961958,-2.30700241443478,4.92237218718104));
#21002=CARTESIAN_POINT('Ctrl Pts',(3.5839962825695,-2.20373500013601,4.91125839812423));
#21003=CARTESIAN_POINT('Ctrl Pts',(3.75621375300573,-2.28011116601395,4.90014460906743));
#21004=CARTESIAN_POINT('Ctrl Pts',(3.78544700372942,-2.46622294126882,4.88903082001062));
#21005=CARTESIAN_POINT('Ctrl Pts',(3.64493850882848,-2.59172010736228,4.87791703095382));
#21006=CARTESIAN_POINT('Ctrl Pts',(3.463297287159,-2.54173368493256,4.86680324189701));
#21007=CARTESIAN_POINT('Ctrl Pts',(3.40678160886734,-2.36201681331505,4.85568945284021));
#21008=CARTESIAN_POINT('Ctrl Pts',(3.52712091522486,-2.21706638322876,4.8445756637834));
#21009=CARTESIAN_POINT('Ctrl Pts',(3.71416727438218,-2.23955716718158,4.8334618747266));
#21010=CARTESIAN_POINT('Ctrl Pts',(3.7967150325525,-2.40890309555853,4.8223480856698));
#21011=CARTESIAN_POINT('Ctrl Pts',(3.69920729052733,-2.57009991960281,4.81123429661299));
#21012=CARTESIAN_POINT('Ctrl Pts',(3.5108939903953,-2.57560235817033,4.80012050755619));
#21013=CARTESIAN_POINT('Ctrl Pts',(3.40414043138533,-2.42037396683837,4.78900671849938));
#21014=CARTESIAN_POINT('Ctrl Pts',(3.47665935672695,-2.24649705260274,4.77789292944258));
#21015=CARTESIAN_POINT('Ctrl Pts',(3.66207337163443,-2.21312312696165,4.76677914038577));
#21016=CARTESIAN_POINT('Ctrl Pts',(3.790670925525,-2.35079972254045,4.75566535132897));
#21017=CARTESIAN_POINT('Ctrl Pts',(3.74474521892717,-2.53350989004707,4.74455156227217));
#21018=CARTESIAN_POINT('Ctrl Pts',(3.56633257192288,-2.59401694108847,4.73343777321536));
#21019=CARTESIAN_POINT('Ctrl Pts',(3.41873610365217,-2.47693808564983,4.72232398415856));
#21020=CARTESIAN_POINT('Ctrl Pts',(3.43705253538103,-2.28943692787866,4.71121019510175));
#21021=CARTESIAN_POINT('Ctrl Pts',(3.60451662942557,-2.20313540389068,4.70009640604496));
#21022=CARTESIAN_POINT('Ctrl Pts',(3.76784660133481,-2.29702627731791,4.68898261698814));
#21023=CARTESIAN_POINT('Ctrl Pts',(3.7775446755324,-2.48517016691753,4.67786882793135));
#21024=CARTESIAN_POINT('Ctrl Pts',(3.62473409472155,-2.59535683684209,4.66675503887453));
#21025=CARTESIAN_POINT('Ctrl Pts',(3.44928411650849,-2.526731178508,4.65564124981774));
#21026=CARTESIAN_POINT('Ctrl Pts',(3.4117860956893,-2.34210703525596,4.64452746076092));
#21027=CARTESIAN_POINT('Ctrl Pts',(3.5465623959771,-2.21047297918554,4.63341367170413));
#21028=CARTESIAN_POINT('Ctrl Pts',(3.73025074124959,-2.25231515464815,4.62229988264732));
#21029=CARTESIAN_POINT('Ctrl Pts',(3.79471910591469,-2.42933494392347,4.61118609359052));
#21030=CARTESIAN_POINT('Ctrl Pts',(3.68095886466676,-2.57950412634054,4.60007230453372));
#21031=CARTESIAN_POINT('Ctrl Pts',(3.49309605646229,-2.56537114621128,4.5889585154769));
#21032=CARTESIAN_POINT('Ctrl Pts',(3.40308364013322,-2.39987208050163,4.57784472642011));
#21033=CARTESIAN_POINT('Ctrl Pts',(3.49331100120934,-2.23449010099328,4.56673093736329));
#21034=CARTESIAN_POINT('Ctrl Pts',(3.68119201274259,-2.22060120898816,4.5556171483065));
#21035=CARTESIAN_POINT('Ctrl Pts',(3.79475705437564,-2.37091806505204,4.54450335924969));
#21036=CARTESIAN_POINT('Ctrl Pts',(3.73005875515687,-2.5478539457147,4.53338957019289));
#21037=CARTESIAN_POINT('Ctrl Pts',(3.54631620295015,-2.58945743362876,4.52227578113609));
#21038=CARTESIAN_POINT('Ctrl Pts',(3.4117110378502,-2.45764838286418,4.51116199207927));
#21039=CARTESIAN_POINT('Ctrl Pts',(3.4494488974476,-2.27307311565868,4.50004820302248));
#21040=CARTESIAN_POINT('Ctrl Pts',(3.62498788397304,-2.20467546079158,4.48893441396567));
#21041=CARTESIAN_POINT('Ctrl Pts',(3.77765518613299,-2.31506058049763,4.47782062490887));
#21042=CARTESIAN_POINT('Ctrl Pts',(3.76771266322612,-2.50319169672563,4.46670683585206));
#21043=CARTESIAN_POINT('Ctrl Pts',(3.60426087461964,-2.59687031755667,4.45559304679526));
#21044=CARTESIAN_POINT('Ctrl Pts',(3.43690898519305,-2.51035123421737,4.44447925773846));
#21045=CARTESIAN_POINT('Ctrl Pts',(3.41883629926506,-2.32282655457101,4.43336546868165));
#21046=CARTESIAN_POINT('Ctrl Pts',(3.56658450672058,-2.20593932476892,4.42225167962485));
#21047=CARTESIAN_POINT('Ctrl Pts',(3.74491888760239,-2.26667859229642,4.41113789056804));
#21048=CARTESIAN_POINT('Ctrl Pts',(3.79060617902903,-2.4494473341432,4.40002410151123));
#21049=CARTESIAN_POINT('Ctrl Pts',(3.66183185185417,-2.58695861678637,4.38891031245443));
#21050=CARTESIAN_POINT('Ctrl Pts',(3.47645736727312,-2.55334005966823,4.37779652339763));
#21051=CARTESIAN_POINT('Ctrl Pts',(3.40417238952257,-2.37937661117104,4.36668273434082));
#21052=CARTESIAN_POINT('Ctrl Pts',(3.51111155676555,-2.22427195756156,4.35556894528402));
#21053=CARTESIAN_POINT('Ctrl Pts',(3.69944954322327,-2.2300492657403,4.34445515622722));
#21054=CARTESIAN_POINT('Ctrl Pts',(3.79668365296711,-2.39131213050928,4.33334136717041));
#21055=CARTESIAN_POINT('Ctrl Pts',(3.71404522611737,-2.56067208765049,4.32222757811361));
#21056=CARTESIAN_POINT('Ctrl Pts',(3.5267002840363,-2.58267282875636,4.31111378905681));
#21057=CARTESIAN_POINT('Ctrl Pts',(3.44710223937223,-2.48629498572918,4.30370459635227));
#21058=CARTESIAN_POINT('Ctrl Pts',(3.43648706727485,-2.43192304546281,4.3));
#21059=CARTESIAN_POINT('Ctrl Pts',(3.43361559198215,-2.39990578567643,5.13785196366098));
#21060=CARTESIAN_POINT('Ctrl Pts',(3.43350388051965,-2.378317282854,5.13641270219409));
#21061=CARTESIAN_POINT('Ctrl Pts',(3.43740296507651,-2.35676746744261,5.1349734407272));
#21062=CARTESIAN_POINT('Ctrl Pts',(3.44550005695817,-2.33693142446689,5.13353417926032));
#21063=CARTESIAN_POINT('Ctrl Pts',(3.4663416189251,-2.28587431348193,5.12982958290805));
#21064=CARTESIAN_POINT('Ctrl Pts',(3.51499603674961,-2.24617137652238,5.12612498655578));
#21065=CARTESIAN_POINT('Ctrl Pts',(3.56919529988925,-2.23599162387719,5.12242039020351));
#21066=CARTESIAN_POINT('Ctrl Pts',(3.62339456302889,-2.225811871232,5.11871579385124));
#21067=CARTESIAN_POINT('Ctrl Pts',(3.68313867148366,-2.24515530290117,5.11501119749898));
#21068=CARTESIAN_POINT('Ctrl Pts',(3.72108591488939,-2.28516991902867,5.11130660114671));
#21069=CARTESIAN_POINT('Ctrl Pts',(3.75903315829512,-2.32518453515617,5.10760200479444));
#21070=CARTESIAN_POINT('Ctrl Pts',(3.7751835366518,-2.38587033574201,5.10389740844217));
#21071=CARTESIAN_POINT('Ctrl Pts',(3.76214547816699,-2.43945380468907,5.1001928120899));
#21072=CARTESIAN_POINT('Ctrl Pts',(3.74910741968218,-2.49303727363614,5.09648821573763));
#21073=CARTESIAN_POINT('Ctrl Pts',(3.70688092435589,-2.53951841094443,5.09278361938536));
#21074=CARTESIAN_POINT('Ctrl Pts',(3.65479131686289,-2.55762501807309,5.0890790230331));
#21075=CARTESIAN_POINT('Ctrl Pts',(3.60270170936989,-2.57573162520175,5.08537442668083));
#21076=CARTESIAN_POINT('Ctrl Pts',(3.5407489897102,-2.56546370215076,5.08166983032856));
#21077=CARTESIAN_POINT('Ctrl Pts',(3.49728610657327,-2.53152034344996,5.0779652339763));
#21078=CARTESIAN_POINT('Ctrl Pts',(3.45773596902793,-2.50063273525474,5.07459414387119));
#21079=CARTESIAN_POINT('Ctrl Pts',(3.43349642418942,-2.45014057555659,5.07122305376608));
#21080=CARTESIAN_POINT('Ctrl Pts',(3.43317939237559,-2.39991359865598,5.06785196366098));
#21081=CARTESIAN_POINT('Ctrl Pts',(3.54698297828114,-2.59851743256717,5.2));
#21082=CARTESIAN_POINT('Ctrl Pts',(3.53457951946873,-2.59392489162072,5.2));
#21083=CARTESIAN_POINT('Ctrl Pts',(3.52273021669441,-2.5880656264448,5.2));
#21084=CARTESIAN_POINT('Ctrl Pts',(3.51155282078554,-2.58110287559691,5.2));
#21085=CARTESIAN_POINT('Ctrl Pts',(3.50588661273558,-2.57757321670087,5.2));
#21086=CARTESIAN_POINT('Ctrl Pts',(3.50039351027032,-2.5737592340707,5.2));
#21087=CARTESIAN_POINT('Ctrl Pts',(3.49509228904167,-2.56967861696227,5.2));
#21088=CARTESIAN_POINT('Ctrl Pts',(3.4905050126104,-2.5661475591401,5.2));
#21089=CARTESIAN_POINT('Ctrl Pts',(3.48606143928385,-2.56241679614242,5.2));
#21090=CARTESIAN_POINT('Ctrl Pts',(3.48177554227615,-2.55849690369355,5.2));
#21091=CARTESIAN_POINT('Ctrl Pts',(3.47866533036506,-2.55565229586402,5.2));
#21092=CARTESIAN_POINT('Ctrl Pts',(3.47564434245519,-2.5527135073757,5.2));
#21093=CARTESIAN_POINT('Ctrl Pts',(3.47272197556915,-2.54969075241385,5.2));
#21094=CARTESIAN_POINT('Ctrl Pts',(3.4637769959157,-2.54043849809891,5.2));
#21095=CARTESIAN_POINT('Ctrl Pts',(3.45573629551605,-2.5303863939551,5.2));
#21096=CARTESIAN_POINT('Ctrl Pts',(3.44873891503949,-2.51966547725229,5.2));
#21097=CARTESIAN_POINT('Ctrl Pts',(3.44420807340926,-2.51272362581603,5.2));
#21098=CARTESIAN_POINT('Ctrl Pts',(3.44011549441187,-2.50550078770205,5.2));
#21099=CARTESIAN_POINT('Ctrl Pts',(3.43651065828778,-2.49802988469159,5.2));
#21100=CARTESIAN_POINT('Ctrl Pts',(3.43484392828386,-2.49457564217533,5.2));
#21101=CARTESIAN_POINT('Ctrl Pts',(3.43328559790363,-2.49107645830187,5.2));
#21102=CARTESIAN_POINT('Ctrl Pts',(3.43184079842385,-2.48753928615204,5.2));
#21103=CARTESIAN_POINT('Ctrl Pts',(3.4278386851231,-2.47774127341323,5.2));
#21104=CARTESIAN_POINT('Ctrl Pts',(3.42470153714545,-2.46764377419319,5.2));
#21105=CARTESIAN_POINT('Ctrl Pts',(3.42252346903458,-2.4573201729425,5.2));
#21106=CARTESIAN_POINT('Ctrl Pts',(3.42066967900374,-2.44853358404506,5.2));
#21107=CARTESIAN_POINT('Ctrl Pts',(3.41951138514856,-2.43958272486992,5.2));
#21108=CARTESIAN_POINT('Ctrl Pts',(3.4190359581172,-2.43054589510015,5.2));
#21109=CARTESIAN_POINT('Ctrl Pts',(3.41886681623208,-2.42733087718605,5.2));
#21110=CARTESIAN_POINT('Ctrl Pts',(3.41878446710974,-2.42410641682356,5.2));
#21111=CARTESIAN_POINT('Ctrl Pts',(3.4187879805801,-2.42088574908536,5.2));
#21112=CARTESIAN_POINT('Ctrl Pts',(3.41880075373106,-2.40917707615745,5.2));
#21113=CARTESIAN_POINT('Ctrl Pts',(3.41994281751926,-2.39748218187535,5.2));
#21114=CARTESIAN_POINT('Ctrl Pts',(3.42216878576612,-2.38597338048412,5.2));
#21115=CARTESIAN_POINT('Ctrl Pts',(3.42331180295367,-2.38006370148633,5.2));
#21116=CARTESIAN_POINT('Ctrl Pts',(3.4247413109463,-2.37420327369848,5.2));
#21117=CARTESIAN_POINT('Ctrl Pts',(3.42645509270942,-2.36841769265549,5.2));
#21118=CARTESIAN_POINT('Ctrl Pts',(3.42814232412983,-2.36272174330468,5.2));
#21119=CARTESIAN_POINT('Ctrl Pts',(3.430107844827,-2.35709290248798,5.2));
#21120=CARTESIAN_POINT('Ctrl Pts',(3.43233768211765,-2.35158848883877,5.2));
#21121=CARTESIAN_POINT('Ctrl Pts',(3.43579440103488,-2.34305548471816,5.2));
#21122=CARTESIAN_POINT('Ctrl Pts',(3.4398879741905,-2.33480787202203,5.2));
#21123=CARTESIAN_POINT('Ctrl Pts',(3.44460905895211,-2.32694151527758,5.2));
#21124=CARTESIAN_POINT('Ctrl Pts',(3.44702307993388,-2.32291922989401,5.2));
#21125=CARTESIAN_POINT('Ctrl Pts',(3.44960209197192,-2.31899653386197,5.2));
#21126=CARTESIAN_POINT('Ctrl Pts',(3.45233605539852,-2.31519993624376,5.2));
#21127=CARTESIAN_POINT('Ctrl Pts',(3.45777066118573,-2.30765301327221,5.2));
#21128=CARTESIAN_POINT('Ctrl Pts',(3.46382416246759,-2.30058959612096,5.2));
#21129=CARTESIAN_POINT('Ctrl Pts',(3.47049190863519,-2.29412081302041,5.2));
#21130=CARTESIAN_POINT('Ctrl Pts',(3.47127037804276,-2.29336557285059,5.2));
#21131=CARTESIAN_POINT('Ctrl Pts',(3.472057234472,-2.29261846360327,5.2));
#21132=CARTESIAN_POINT('Ctrl Pts',(3.47285232078577,-2.29187955100915,5.2));
#21133=CARTESIAN_POINT('Origin',(3.6,-2.4,4.7));
#21134=CARTESIAN_POINT('Origin',(-3.6,-2.4,4.3));
#21135=CARTESIAN_POINT('Ctrl Pts',(-3.76351293272515,-2.4319230454628,4.3));
#21136=CARTESIAN_POINT('Ctrl Pts',(-3.76286871316703,-2.44021936733959,
4.3));
#21137=CARTESIAN_POINT('Ctrl Pts',(-3.76155560816075,-2.4484297641735,4.3));
#21138=CARTESIAN_POINT('Ctrl Pts',(-3.75963220162413,-2.45650290122813,
4.3));
#21139=CARTESIAN_POINT('Ctrl Pts',(-3.75857027465495,-2.46096013988305,
4.3));
#21140=CARTESIAN_POINT('Ctrl Pts',(-3.75732202640333,-2.4653756041272,4.3));
#21141=CARTESIAN_POINT('Ctrl Pts',(-3.75589532148576,-2.46974082414556,
4.3));
#21142=CARTESIAN_POINT('Ctrl Pts',(-3.75435560354459,-2.47445182464518,
4.3));
#21143=CARTESIAN_POINT('Ctrl Pts',(-3.75261043098936,-2.47909640157799,
4.3));
#21144=CARTESIAN_POINT('Ctrl Pts',(-3.75067343320617,-2.48365784346818,
4.3));
#21145=CARTESIAN_POINT('Ctrl Pts',(-3.74745266086646,-2.49124244991258,
4.3));
#21146=CARTESIAN_POINT('Ctrl Pts',(-3.74370038620747,-2.49860287239871,
4.3));
#21147=CARTESIAN_POINT('Ctrl Pts',(-3.73945960595045,-2.50569089060563,
4.3));
#21148=CARTESIAN_POINT('Ctrl Pts',(-3.73760643937826,-2.50878826363795,
4.3));
#21149=CARTESIAN_POINT('Ctrl Pts',(-3.73566012601582,-2.511832700902,4.3));
#21150=CARTESIAN_POINT('Ctrl Pts',(-3.73363013483138,-2.51481171247594,
4.3));
#21151=CARTESIAN_POINT('Ctrl Pts',(-3.72675413466501,-2.52490224106299,
4.3));
#21152=CARTESIAN_POINT('Ctrl Pts',(-3.71890630233768,-2.53427022723708,
4.3));
#21153=CARTESIAN_POINT('Ctrl Pts',(-3.710220437496,-2.54276718643201,4.3));
#21154=CARTESIAN_POINT('Ctrl Pts',(-3.70599062580354,-2.54690500552178,
4.3));
#21155=CARTESIAN_POINT('Ctrl Pts',(-3.70156129932866,-2.55083607679561,
4.3));
#21156=CARTESIAN_POINT('Ctrl Pts',(-3.69694397352711,-2.55454119955382,
4.3));
#21157=CARTESIAN_POINT('Ctrl Pts',(-3.69303800092373,-2.55767550469228,
4.3));
#21158=CARTESIAN_POINT('Ctrl Pts',(-3.68899293859581,-2.56065058734466,
4.3));
#21159=CARTESIAN_POINT('Ctrl Pts',(-3.68484116924407,-2.56343733372212,
4.3));
#21160=CARTESIAN_POINT('Ctrl Pts',(-3.67976588279258,-2.56684396230261,
4.3));
#21161=CARTESIAN_POINT('Ctrl Pts',(-3.67452566755957,-2.56997445255576,
4.3));
#21162=CARTESIAN_POINT('Ctrl Pts',(-3.66913578324553,-2.57281068802155,
4.3));
#21163=CARTESIAN_POINT('Ctrl Pts',(-3.66156268589167,-2.57679576192101,
4.3));
#21164=CARTESIAN_POINT('Ctrl Pts',(-3.6536944302201,-2.58020053259861,4.3));
#21165=CARTESIAN_POINT('Ctrl Pts',(-3.64559780863821,-2.58304072868827,
4.3));
#21166=CARTESIAN_POINT('Ctrl Pts',(-3.63968764062526,-2.58511394353595,
4.3));
#21167=CARTESIAN_POINT('Ctrl Pts',(-3.633655561192,-2.58688612240617,4.3));
#21168=CARTESIAN_POINT('Ctrl Pts',(-3.6275253141649,-2.58835973744293,4.3));
#21169=CARTESIAN_POINT('Ctrl Pts',(-3.62399736219549,-2.58920780164787,
4.3));
#21170=CARTESIAN_POINT('Ctrl Pts',(-3.62044138799033,-2.58995568069818,
4.3));
#21171=CARTESIAN_POINT('Ctrl Pts',(-3.61687019594187,-2.59060310935882,
4.3));
#21172=CARTESIAN_POINT('Ctrl Pts',(-3.6053532973959,-2.59269103129053,4.3));
#21173=CARTESIAN_POINT('Ctrl Pts',(-3.5936552916365,-2.5937426794922,4.3));
#21174=CARTESIAN_POINT('Ctrl Pts',(-3.58193296271379,-2.5937913460953,4.3));
#21175=CARTESIAN_POINT('Ctrl Pts',(-3.57526861453522,-2.59381901390686,
4.3));
#21176=CARTESIAN_POINT('Ctrl Pts',(-3.56859601622939,-2.59352191446421,
4.3));
#21177=CARTESIAN_POINT('Ctrl Pts',(-3.56194230797419,-2.5929013482942,4.3));
#21178=CARTESIAN_POINT('Ctrl Pts',(-3.55784543918526,-2.59251924885793,
4.3));
#21179=CARTESIAN_POINT('Ctrl Pts',(-3.55375366053793,-2.59201412364595,
4.3));
#21180=CARTESIAN_POINT('Ctrl Pts',(-3.54967980921583,-2.59138661988454,
4.3));
#21181=CARTESIAN_POINT('Ctrl Pts',(-3.53642388866962,-2.5893447829725,4.3));
#21182=CARTESIAN_POINT('Ctrl Pts',(-3.52344434481125,-2.58602557270852,
4.3));
#21183=CARTESIAN_POINT('Ctrl Pts',(-3.51095537008143,-2.58146161840675,
4.3));
#21184=CARTESIAN_POINT('Ctrl Pts',(-3.50062243383895,-2.57768556394,4.3));
#21185=CARTESIAN_POINT('Ctrl Pts',(-3.49062430896861,-2.57305657702062,
4.3));
#21186=CARTESIAN_POINT('Ctrl Pts',(-3.48108410771908,-2.56756616374223,
4.3));
#21187=CARTESIAN_POINT('Ctrl Pts',(-3.47992982857924,-2.56690187277492,
4.3));
#21188=CARTESIAN_POINT('Ctrl Pts',(-3.47878226433178,-2.56622494144235,
4.3));
#21189=CARTESIAN_POINT('Ctrl Pts',(-3.47764149510761,-2.56553553810743,
4.3));
#21190=CARTESIAN_POINT('Ctrl Pts',(-3.41173724903364,-2.48232321801034,
4.3));
#21191=CARTESIAN_POINT('Ctrl Pts',(-3.40908132671273,-2.474270631223,4.3));
#21192=CARTESIAN_POINT('Ctrl Pts',(-3.40697195813618,-2.46606039521676,
4.3));
#21193=CARTESIAN_POINT('Ctrl Pts',(-3.40539675699364,-2.45774386680553,
4.3));
#21194=CARTESIAN_POINT('Ctrl Pts',(-3.40421043018009,-2.45148046311471,
4.3));
#21195=CARTESIAN_POINT('Ctrl Pts',(-3.40332727350005,-2.44515671203471,
4.3));
#21196=CARTESIAN_POINT('Ctrl Pts',(-3.40274510705531,-2.43879482091291,
4.3));
#21197=CARTESIAN_POINT('Ctrl Pts',(-3.40230912033401,-2.4340303758362,4.3));
#21198=CARTESIAN_POINT('Ctrl Pts',(-3.40204240567473,-2.42924590842869,
4.3));
#21199=CARTESIAN_POINT('Ctrl Pts',(-3.40194407560279,-2.42446300988855,
4.3));
#21200=CARTESIAN_POINT('Ctrl Pts',(-3.4017383892304,-2.41445816568562,4.3));
#21201=CARTESIAN_POINT('Ctrl Pts',(-3.40226690961593,-2.40444523502109,
4.3));
#21202=CARTESIAN_POINT('Ctrl Pts',(-3.40352193796024,-2.39451254861871,
4.3));
#21203=CARTESIAN_POINT('Ctrl Pts',(-3.40417749889618,-2.3893242345667,4.3));
#21204=CARTESIAN_POINT('Ctrl Pts',(-3.4050325722576,-2.38415490381948,4.3));
#21205=CARTESIAN_POINT('Ctrl Pts',(-3.40608153527603,-2.37904223030681,
4.3));
#21206=CARTESIAN_POINT('Ctrl Pts',(-3.40864847953637,-2.36653087604773,
4.3));
#21207=CARTESIAN_POINT('Ctrl Pts',(-3.41237572714265,-2.35432631626979,
4.3));
#21208=CARTESIAN_POINT('Ctrl Pts',(-3.41724961050618,-2.34261710559519,
4.3));
#21209=CARTESIAN_POINT('Ctrl Pts',(-3.41948718042203,-2.33724147889476,
4.3));
#21210=CARTESIAN_POINT('Ctrl Pts',(-3.42196704076708,-2.33197060519316,
4.3));
#21211=CARTESIAN_POINT('Ctrl Pts',(-3.42469079211682,-2.32682518779718,
4.3));
#21212=CARTESIAN_POINT('Ctrl Pts',(-3.42647141933207,-2.32346141883567,
4.3));
#21213=CARTESIAN_POINT('Ctrl Pts',(-3.42835738874669,-2.3201495667824,4.3));
#21214=CARTESIAN_POINT('Ctrl Pts',(-3.430346105223,-2.31690145647487,4.3));
#21215=CARTESIAN_POINT('Ctrl Pts',(-3.43461852095602,-2.30992344943073,
4.3));
#21216=CARTESIAN_POINT('Ctrl Pts',(-3.43934738846969,-2.3032660957291,4.3));
#21217=CARTESIAN_POINT('Ctrl Pts',(-3.44453058590951,-2.29698173842211,
4.3));
#21218=CARTESIAN_POINT('Ctrl Pts',(-3.4502359337428,-2.29006430092116,4.3));
#21219=CARTESIAN_POINT('Ctrl Pts',(-3.45649195144988,-2.28359849259699,
4.3));
#21220=CARTESIAN_POINT('Ctrl Pts',(-3.4632263722909,-2.27761731307503,4.3));
#21221=CARTESIAN_POINT('Ctrl Pts',(-3.46747035511976,-2.27384801742411,
4.3));
#21222=CARTESIAN_POINT('Ctrl Pts',(-3.47190450284819,-2.27027143263625,
4.3));
#21223=CARTESIAN_POINT('Ctrl Pts',(-3.47651159455371,-2.26689859050011,
4.3));
#21224=CARTESIAN_POINT('Ctrl Pts',(-3.4793251060266,-2.26483882467541,4.3));
#21225=CARTESIAN_POINT('Ctrl Pts',(-3.48219970787858,-2.26285776645565,
4.3));
#21226=CARTESIAN_POINT('Ctrl Pts',(-3.48512436737332,-2.26096157786103,
4.3));
#21227=CARTESIAN_POINT('Ctrl Pts',(-3.49373619954507,-2.25537813884111,
4.3));
#21228=CARTESIAN_POINT('Ctrl Pts',(-3.50279847994849,-2.25051611152294,
4.3));
#21229=CARTESIAN_POINT('Ctrl Pts',(-3.51220227087042,-2.24642657080492,
4.3));
#21230=CARTESIAN_POINT('Ctrl Pts',(-3.5210281717619,-2.24258834413989,4.3));
#21231=CARTESIAN_POINT('Ctrl Pts',(-3.53015556945347,-2.23943063412497,
4.3));
#21232=CARTESIAN_POINT('Ctrl Pts',(-3.53949489532435,-2.23701751505981,
4.3));
#21233=CARTESIAN_POINT('Ctrl Pts',(-3.54298225084135,-2.23611644316218,
4.3));
#21234=CARTESIAN_POINT('Ctrl Pts',(-3.54649061678302,-2.23532167500438,
4.3));
#21235=CARTESIAN_POINT('Ctrl Pts',(-3.5500119948057,-2.23463615769257,4.3));
#21236=CARTESIAN_POINT('Ctrl Pts',(-3.5610932074021,-2.23247894451586,4.3));
#21237=CARTESIAN_POINT('Ctrl Pts',(-3.57231428638466,-2.23139729676061,
4.3));
#21238=CARTESIAN_POINT('Ctrl Pts',(-3.58352462409827,-2.2314877485142,4.3));
#21239=CARTESIAN_POINT('Ctrl Pts',(-3.58970653876345,-2.23153762792339,
4.3));
#21240=CARTESIAN_POINT('Ctrl Pts',(-3.59588508216706,-2.23194477463139,
4.3));
#21241=CARTESIAN_POINT('Ctrl Pts',(-3.60203269161667,-2.23273189903069,
4.3));
#21242=CARTESIAN_POINT('Ctrl Pts',(-3.60310835631345,-2.23286962442383,
4.3));
#21243=CARTESIAN_POINT('Ctrl Pts',(-3.60418306761235,-2.23301899515145,
4.3));
#21244=CARTESIAN_POINT('Ctrl Pts',(-3.60525667255607,-2.23317994016621,
4.3));
#21245=CARTESIAN_POINT('Origin',(-3.6,-2.4,5.35459252805377));
#21246=CARTESIAN_POINT('Ctrl Pts',(-3.80565733457988,-2.39985006589818,
5.17959252805377));
#21247=CARTESIAN_POINT('Ctrl Pts',(-3.8057391516022,-2.39002097154438,5.17905813053169));
#21248=CARTESIAN_POINT('Ctrl Pts',(-3.80062938506941,-2.31213685567809,
5.17481913665734));
#21249=CARTESIAN_POINT('Ctrl Pts',(-3.70109554203788,-2.17915701647198,
5.16687554643073));
#21250=CARTESIAN_POINT('Ctrl Pts',(-3.46929950206046,-2.19531102353728,
5.15576175737392));
#21251=CARTESIAN_POINT('Ctrl Pts',(-3.35713783153282,-2.39878694399818,
5.14464796831711));
#21252=CARTESIAN_POINT('Ctrl Pts',(-3.46726929886284,-2.60338928299931,
5.13353417926032));
#21253=CARTESIAN_POINT('Ctrl Pts',(-3.69889136100131,-2.62181906697108,
5.12242039020351));
#21254=CARTESIAN_POINT('Ctrl Pts',(-3.80021578451737,-2.48926235936684,
5.11443983980133));
#21255=CARTESIAN_POINT('Ctrl Pts',(-3.80572902589707,-2.41067410853188,
5.11016388575141));
#21256=CARTESIAN_POINT('Ctrl Pts',(-3.8056388038084,-2.40016037433918,5.10959252805377));
#21257=CARTESIAN_POINT('Ctrl Pts',(-3.80526708169851,-2.40022955265959,
5.18540747194623));
#21258=CARTESIAN_POINT('Ctrl Pts',(-3.80491230300414,-2.3532097525552,5.18286245525962));
#21259=CARTESIAN_POINT('Ctrl Pts',(-3.76565541968849,-2.23704708335906,
5.17661284222073));
#21260=CARTESIAN_POINT('Ctrl Pts',(-3.5727867642971,-2.15871465280967,5.16665863282959));
#21261=CARTESIAN_POINT('Ctrl Pts',(-3.38252461999799,-2.29190667528476,
5.15554484377278));
#21262=CARTESIAN_POINT('Ctrl Pts',(-3.39123766053156,-2.52413789941101,
5.14443105471598));
#21263=CARTESIAN_POINT('Ctrl Pts',(-3.59107442597796,-2.64269432067786,
5.13331726565918));
#21264=CARTESIAN_POINT('Ctrl Pts',(-3.77212564872883,-2.55254602634109,
5.12364273806926));
#21265=CARTESIAN_POINT('Ctrl Pts',(-3.80499226553068,-2.44179202539712,
5.11767280683161));
#21266=CARTESIAN_POINT('Ctrl Pts',(-3.80520912268496,-2.39988380060309,
5.11540747194623));
#21267=CARTESIAN_POINT('Ctrl Pts',(-3.47309291201476,-2.29206413469515,
5.2));
#21268=CARTESIAN_POINT('Ctrl Pts',(-3.43720166889934,-2.33426376069605,
5.19629540364773));
#21269=CARTESIAN_POINT('Ctrl Pts',(-3.4114791580674,-2.45658678033172,5.1888862109432));
#21270=CARTESIAN_POINT('Ctrl Pts',(-3.54548746492724,-2.5893415011903,5.17777242188639));
#21271=CARTESIAN_POINT('Ctrl Pts',(-3.72942274690437,-2.54835673318009,
5.16665863282959));
#21272=CARTESIAN_POINT('Ctrl Pts',(-3.79487861290014,-2.37179020383286,
5.15554484377278));
#21273=CARTESIAN_POINT('Ctrl Pts',(-3.68196869353212,-2.22093957388603,
5.14443105471598));
#21274=CARTESIAN_POINT('Ctrl Pts',(-3.49402748287272,-2.23403731121212,
5.13331726565918));
#21275=CARTESIAN_POINT('Ctrl Pts',(-3.40308632550611,-2.39901644905753,
5.12220347660237));
#21276=CARTESIAN_POINT('Ctrl Pts',(-3.49238138552402,-2.56490889182472,
5.11108968754557));
#21277=CARTESIAN_POINT('Ctrl Pts',(-3.68018153421496,-2.57985183870243,
5.09997589848876));
#21278=CARTESIAN_POINT('Ctrl Pts',(-3.79459034046341,-2.43017761257843,
5.08886210943196));
#21279=CARTESIAN_POINT('Ctrl Pts',(-3.73088853854501,-2.25287985005212,
5.07774832037516));
#21280=CARTESIAN_POINT('Ctrl Pts',(-3.5473829043692,-2.21024364094684,5.06663453131835));
#21281=CARTESIAN_POINT('Ctrl Pts',(-3.41203832877697,-2.34129317389102,
5.05552074226154));
#21282=CARTESIAN_POINT('Ctrl Pts',(-3.44873718538878,-2.52607793299967,
5.04440695320475));
#21283=CARTESIAN_POINT('Ctrl Pts',(-3.62388862018941,-2.59546202911018,
5.03329316414794));
#21284=CARTESIAN_POINT('Ctrl Pts',(-3.77717452575129,-2.48593756377701,
5.02217937509113));
#21285=CARTESIAN_POINT('Ctrl Pts',(-3.76829058072669,-2.29775344650504,
5.01106558603433));
#21286=CARTESIAN_POINT('Ctrl Pts',(-3.6053683575545,-2.20315677179449,4.99995179697753));
#21287=CARTESIAN_POINT('Ctrl Pts',(-3.43753241636245,-2.28873292992563,
4.98883800792072));
#21288=CARTESIAN_POINT('Ctrl Pts',(-3.41840489671633,-2.47615310229093,
4.97772421886392));
#21289=CARTESIAN_POINT('Ctrl Pts',(-3.56549343466676,-2.59386947492594,
4.96661042980711));
#21290=CARTESIAN_POINT('Ctrl Pts',(-3.74416622313161,-2.53413491931517,
4.95549664075031));
#21291=CARTESIAN_POINT('Ctrl Pts',(-3.79088203264097,-2.35162515047058,
4.9443828516935));
#21292=CARTESIAN_POINT('Ctrl Pts',(-3.66288135290806,-2.21339343020375,
4.9332690626367));
#21293=CARTESIAN_POINT('Ctrl Pts',(-3.47732465774361,-2.24596481943629,
4.9221552735799));
#21294=CARTESIAN_POINT('Ctrl Pts',(-3.40405409457531,-2.41952635636528,
4.91104148452309));
#21295=CARTESIAN_POINT('Ctrl Pts',(-3.51013504082201,-2.57521519784486,
4.89992769546629));
#21296=CARTESIAN_POINT('Ctrl Pts',(-3.69847040334124,-2.57052758167369,
4.88881390640948));
#21297=CARTESIAN_POINT('Ctrl Pts',(-3.79667468895243,-2.40975413607622,
4.87770011735268));
#21298=CARTESIAN_POINT('Ctrl Pts',(-3.71486040132253,-2.24005261911178,
4.86658632829587));
#21299=CARTESIAN_POINT('Ctrl Pts',(-3.5279130857567,-2.2167527537995,4.85547253923907));
#21300=CARTESIAN_POINT('Ctrl Pts',(-3.40694774031892,-2.3611811711004,4.84435875018227));
#21301=CARTESIAN_POINT('Ctrl Pts',(-3.46268531752878,-2.5411409027282,4.83324496112546));
#21302=CARTESIAN_POINT('Ctrl Pts',(-3.64410858085897,-2.59191276544236,
4.82213117206866));
#21303=CARTESIAN_POINT('Ctrl Pts',(-3.7851587599036,-2.46702469750825,4.81101738301185));
#21304=CARTESIAN_POINT('Ctrl Pts',(-3.75673102616532,-2.28078816383312,
4.79990359395505));
#21305=CARTESIAN_POINT('Ctrl Pts',(-3.58484560672719,-2.20366757575568,
4.78878980489824));
#21306=CARTESIAN_POINT('Ctrl Pts',(-3.42683117531417,-2.30625228215021,
4.77767601584145));
#21307=CARTESIAN_POINT('Ctrl Pts',(-3.42732013300413,-2.49464533786407,
4.76656222678464));
#21308=CARTESIAN_POINT('Ctrl Pts',(-3.5858649312783,-2.59640844247982,4.75544843772783));
#21309=CARTESIAN_POINT('Ctrl Pts',(-3.75734771825602,-2.51839667227055,
4.74433464867103));
#21310=CARTESIAN_POINT('Ctrl Pts',(-3.78480835426951,-2.33201508522246,
4.73322085961423));
#21311=CARTESIAN_POINT('Ctrl Pts',(-3.64311180775084,-2.20786086167162,
4.72210707055742));
#21312=CARTESIAN_POINT('Ctrl Pts',(-3.46195453467666,-2.25957377043879,
4.71099328150062));
#21313=CARTESIAN_POINT('Ctrl Pts',(-3.407151841555,-2.43982039966509,4.69987949244381));
#21314=CARTESIAN_POINT('Ctrl Pts',(-3.52886525490491,-2.58361896548389,
4.68876570338701));
#21315=CARTESIAN_POINT('Ctrl Pts',(-3.71568910716324,-2.55934900981458,
4.6776519143302));
#21316=CARTESIAN_POINT('Ctrl Pts',(-3.79662140763134,-2.38922509832133,
4.6665381252734));
#21317=CARTESIAN_POINT('Ctrl Pts',(-3.69758390385606,-2.22896357653021,
4.65542433621659));
#21318=CARTESIAN_POINT('Ctrl Pts',(-3.50922674620458,-2.22525363282606,
4.64431054715979));
#21319=CARTESIAN_POINT('Ctrl Pts',(-3.40395537719079,-2.38149102075462,
4.63319675810299));
#21320=CARTESIAN_POINT('Ctrl Pts',(-3.47812587473144,-2.55466988729295,
4.62208296904618));
#21321=CARTESIAN_POINT('Ctrl Pts',(-3.66384914127714,-2.58627765191548,
4.61096917998938));
#21322=CARTESIAN_POINT('Ctrl Pts',(-3.79113056471305,-2.447383369209,4.59985539093257));
#21323=CARTESIAN_POINT('Ctrl Pts',(-3.74346801469971,-2.26511855129859,
4.58874160187577));
#21324=CARTESIAN_POINT('Ctrl Pts',(-3.56448756379251,-2.20631225305021,
4.57762781281896));
#21325=CARTESIAN_POINT('Ctrl Pts',(-3.41801204848697,-2.32479054614148,
4.56651402376216));
#21326=CARTESIAN_POINT('Ctrl Pts',(-3.43811216908,-2.51210890530657,4.55540023470536));
#21327=CARTESIAN_POINT('Ctrl Pts',(-3.60639005725709,-2.59681271199525,
4.54428644564855));
#21328=CARTESIAN_POINT('Ctrl Pts',(-3.76881905353834,-2.50137161148251,
4.53317265659175));
#21329=CARTESIAN_POINT('Ctrl Pts',(-3.77672605561821,-2.31314392515575,
4.52205886753495));
#21330=CARTESIAN_POINT('Ctrl Pts',(-3.62287369469976,-2.2044165895329,4.51094507847814));
#21331=CARTESIAN_POINT('Ctrl Pts',(-3.44808478177985,-2.27470896680823,
4.49983128942134));
#21332=CARTESIAN_POINT('Ctrl Pts',(-3.41234559060706,-2.45968164920097,
4.48871750036453));
#21333=CARTESIAN_POINT('Ctrl Pts',(-3.54836860914922,-2.5900270381604,4.47760371130773));
#21334=CARTESIAN_POINT('Ctrl Pts',(-3.73165042397165,-2.54643853021323,
4.46648992225092));
#21335=CARTESIAN_POINT('Ctrl Pts',(-3.79443111532907,-2.36881316247168,
4.45537613319412));
#21336=CARTESIAN_POINT('Ctrl Pts',(-3.67924679659355,-2.21973348556073,
4.44426234413731));
#21337=CARTESIAN_POINT('Ctrl Pts',(-3.49152699669547,-2.23565374410205,
4.43314855508051));
#21338=CARTESIAN_POINT('Ctrl Pts',(-3.40309374590592,-2.40200209374894,
4.4220347660237));
#21339=CARTESIAN_POINT('Ctrl Pts',(-3.49489106457482,-2.5665177055076,4.41092097696691));
#21340=CARTESIAN_POINT('Ctrl Pts',(-3.68289569971986,-2.57861817099917,
4.39980718791009));
#21341=CARTESIAN_POINT('Ctrl Pts',(-3.79502512928071,-2.42722660191142,
4.3886933988533));
#21342=CARTESIAN_POINT('Ctrl Pts',(-3.72864550893249,-2.25091581121659,
4.37757960979648));
#21343=CARTESIAN_POINT('Ctrl Pts',(-3.54451587080997,-2.21106027365159,
4.36646582073969));
#21344=CARTESIAN_POINT('Ctrl Pts',(-3.41117013277341,-2.34414980914689,
4.35535203168287));
#21345=CARTESIAN_POINT('Ctrl Pts',(-3.45066522211898,-2.5283468448043,4.34423824262609));
#21346=CARTESIAN_POINT('Ctrl Pts',(-3.62684270366593,-2.59509221455348,
4.33312445356927));
#21347=CARTESIAN_POINT('Ctrl Pts',(-3.77846161739066,-2.4832160890933,4.32201066451248));
#21348=CARTESIAN_POINT('Ctrl Pts',(-3.76671079422265,-2.29527426875025,
4.31089687545566));
#21349=CARTESIAN_POINT('Ctrl Pts',(-3.60241192612029,-2.2029822262702,4.29978308639886));
#21350=CARTESIAN_POINT('Ctrl Pts',(-3.43581020892599,-2.29144640006724,
4.28866929734205));
#21351=CARTESIAN_POINT('Ctrl Pts',(-3.42516046182893,-2.41599017382995,
4.28126010463752));
#21352=CARTESIAN_POINT('Ctrl Pts',(-3.44735576439472,-2.46674801372685,
4.27755550828525));
#21353=CARTESIAN_POINT('Ctrl Pts',(-3.46322193753412,-2.28366876301903,
5.20748149723825));
#21354=CARTESIAN_POINT('Ctrl Pts',(-3.42453903360214,-2.32915072287504,
5.20377690088598));
#21355=CARTESIAN_POINT('Ctrl Pts',(-3.39681579726281,-2.4609881630556,5.19636770818145));
#21356=CARTESIAN_POINT('Ctrl Pts',(-3.54124741930709,-2.60406869378488,
5.18525391912464));
#21357=CARTESIAN_POINT('Ctrl Pts',(-3.73948939213428,-2.55989608492554,
5.17414013006784));
#21358=CARTESIAN_POINT('Ctrl Pts',(-3.81003648820324,-2.36959601450513,
5.16302634101103));
#21359=CARTESIAN_POINT('Ctrl Pts',(-3.68834430970071,-2.20701205474802,
5.15191255195423));
#21360=CARTESIAN_POINT('Ctrl Pts',(-3.48578482260197,-2.22112854865384,
5.14079876289742));
#21361=CARTESIAN_POINT('Ctrl Pts',(-3.38777016084835,-2.39893994737108,
5.12968497384062));
#21362=CARTESIAN_POINT('Ctrl Pts',(-3.4840106899703,-2.57773568888292,5.11857118478382));
#21363=CARTESIAN_POINT('Ctrl Pts',(-3.68641814314374,-2.59384091479198,
5.10745739572701));
#21364=CARTESIAN_POINT('Ctrl Pts',(-3.8097257936157,-2.43252486085572,5.0963436066702));
#21365=CARTESIAN_POINT('Ctrl Pts',(-3.74106919467933,-2.2414366811261,5.08522981761341));
#21366=CARTESIAN_POINT('Ctrl Pts',(-3.54329028813742,-2.19548418024617,
5.0741160285566));
#21367=CARTESIAN_POINT('Ctrl Pts',(-3.39741846089223,-2.33672689164815,
5.06300223949979));
#21368=CARTESIAN_POINT('Ctrl Pts',(-3.43697179539676,-2.53588441488314,
5.051888450443));
#21369=CARTESIAN_POINT('Ctrl Pts',(-3.62574670364252,-2.61066528317513,
5.04077466138618));
#21370=CARTESIAN_POINT('Ctrl Pts',(-3.79095535746114,-2.4926218830884,5.02966087232938));
#21371=CARTESIAN_POINT('Ctrl Pts',(-3.78138040930963,-2.28980059583054,
5.01854708327258));
#21372=CARTESIAN_POINT('Ctrl Pts',(-3.60578591437709,-2.1878460865274,5.00743329421578));
#21373=CARTESIAN_POINT('Ctrl Pts',(-3.42489550697087,-2.28007845343676,
4.99631950515897));
#21374=CARTESIAN_POINT('Ctrl Pts',(-3.40428022756837,-2.48207637530325,
4.98520571610216));
#21375=CARTESIAN_POINT('Ctrl Pts',(-3.56280947562848,-2.60894885835481,
4.97409192704536));
#21376=CARTESIAN_POINT('Ctrl Pts',(-3.75537963234378,-2.54456808255722,
4.96297813798856));
#21377=CARTESIAN_POINT('Ctrl Pts',(-3.80572904948554,-2.34786250085983,
4.95186434893175));
#21378=CARTESIAN_POINT('Ctrl Pts',(-3.6677723344893,-2.19887896361545,4.94075055987495));
#21379=CARTESIAN_POINT('Ctrl Pts',(-3.46778283315333,-2.23398379173638,
4.92963677081814));
#21380=CARTESIAN_POINT('Ctrl Pts',(-3.38881320407234,-2.42104513808537,
4.91852298176134));
#21381=CARTESIAN_POINT('Ctrl Pts',(-3.50314524432732,-2.5888436308505,4.90740919270454));
#21382=CARTESIAN_POINT('Ctrl Pts',(-3.70612954085602,-2.58379140667882,
4.89629540364773));
#21383=CARTESIAN_POINT('Ctrl Pts',(-3.81197226504892,-2.41051282363117,
4.88518161459093));
#21384=CARTESIAN_POINT('Ctrl Pts',(-3.72379437111327,-2.22761173389364,
4.87406782553412));
#21385=CARTESIAN_POINT('Ctrl Pts',(-3.52230608537413,-2.20249957913754,
4.86295403647732));
#21386=CARTESIAN_POINT('Ctrl Pts',(-3.3919319208009,-2.35816179940478,4.85184024742052));
#21387=CARTESIAN_POINT('Ctrl Pts',(-3.45200482877115,-2.55211899915388,
4.84072645836371));
#21388=CARTESIAN_POINT('Ctrl Pts',(-3.64753939534654,-2.60683995383086,
4.82961266930691));
#21389=CARTESIAN_POINT('Ctrl Pts',(-3.79956061422784,-2.47223795304173,
4.8184988802501));
#21390=CARTESIAN_POINT('Ctrl Pts',(-3.7689217397351,-2.27151573459945,4.8073850911933));
#21391=CARTESIAN_POINT('Ctrl Pts',(-3.58366688116,-2.18839662138894,4.79627130213649));
#21392=CARTESIAN_POINT('Ctrl Pts',(-3.41336191148932,-2.29896048036668,
4.78515751307969));
#21393=CARTESIAN_POINT('Ctrl Pts',(-3.41388890085234,-2.50200695753087,
4.77404372402289));
#21394=CARTESIAN_POINT('Ctrl Pts',(-3.58476548990864,-2.61168530962949,
4.76292993496608));
#21395=CARTESIAN_POINT('Ctrl Pts',(-3.76958639882265,-2.52760569714953,
4.75181614590928));
#21396=CARTESIAN_POINT('Ctrl Pts',(-3.79918295365372,-2.32672714292159,
4.74070235685248));
#21397=CARTESIAN_POINT('Ctrl Pts',(-3.64646509211721,-2.19291606574822,
4.72958856779567));
#21398=CARTESIAN_POINT('Ctrl Pts',(-3.45121720481583,-2.24865126208706,
4.71847477873887));
#21399=CARTESIAN_POINT('Ctrl Pts',(-3.39215189725818,-2.44291767464904,
4.70736098968205));
#21400=CARTESIAN_POINT('Ctrl Pts',(-3.52333231529793,-2.59790105288522,
4.69624720062526));
#21401=CARTESIAN_POINT('Ctrl Pts',(-3.72468753461616,-2.57174335306496,
4.68513341156845));
#21402=CARTESIAN_POINT('Ctrl Pts',(-3.8119148394474,-2.38838701448227,4.67401962251165));
#21403=CARTESIAN_POINT('Ctrl Pts',(-3.70517408845471,-2.21566017324412,
4.66290583345485));
#21404=CARTESIAN_POINT('Ctrl Pts',(-3.50216630154411,-2.21166166599155,
4.65179204439804));
#21405=CARTESIAN_POINT('Ctrl Pts',(-3.38870680833984,-2.38005137175869,
4.64067825534123));
#21406=CARTESIAN_POINT('Ctrl Pts',(-3.46864636968979,-2.56670028318833,
4.62956446628443));
#21407=CARTESIAN_POINT('Ctrl Pts',(-3.66881539851434,-2.6007665349051,4.61845067722763));
#21408=CARTESIAN_POINT('Ctrl Pts',(-3.80599691265867,-2.45106890037747,
4.60733688817082));
#21409=CARTESIAN_POINT('Ctrl Pts',(-3.75462711648332,-2.25462732217041,
4.59622309911401));
#21410=CARTESIAN_POINT('Ctrl Pts',(-3.56172536699866,-2.1912470046255,4.58510931005722));
#21411=CARTESIAN_POINT('Ctrl Pts',(-3.4038568231667,-2.31894067115399,4.57399552100041));
#21412=CARTESIAN_POINT('Ctrl Pts',(-3.42552035349974,-2.5208288606763,4.56288173194361));
#21413=CARTESIAN_POINT('Ctrl Pts',(-3.60688708301913,-2.61212102367755,
4.5517679428868));
#21414=CARTESIAN_POINT('Ctrl Pts',(-3.78194998732446,-2.50925640819396,
4.54065415383));
#21415=CARTESIAN_POINT('Ctrl Pts',(-3.79047200482221,-2.30638816303176,
4.52954036477319));
#21416=CARTESIAN_POINT('Ctrl Pts',(-3.62465283611923,-2.18920389429099,
4.51842657571639));
#21417=CARTESIAN_POINT('Ctrl Pts',(-3.43626864710937,-2.2649636908672,4.50731278665958));
#21418=CARTESIAN_POINT('Ctrl Pts',(-3.39774962188927,-2.46432375426836,
4.49619899760278));
#21419=CARTESIAN_POINT('Ctrl Pts',(-3.54435266213177,-2.60480755258314,
4.48508520854598));
#21420=CARTESIAN_POINT('Ctrl Pts',(-3.74189034040202,-2.55782868199802,
4.47397141948917));
#21421=CARTESIAN_POINT('Ctrl Pts',(-3.80955418377328,-2.36638741555509,
4.46285763043236));
#21422=CARTESIAN_POINT('Ctrl Pts',(-3.68541070059029,-2.20571215553106,
4.45174384137557));
#21423=CARTESIAN_POINT('Ctrl Pts',(-3.4830898458282,-2.22287070949214,4.44063005231875));
#21424=CARTESIAN_POINT('Ctrl Pts',(-3.3877781584151,-2.40215781882795,4.42951626326196));
#21425=CARTESIAN_POINT('Ctrl Pts',(-3.48671557464955,-2.57946963788377,
4.41840247420515));
#21426=CARTESIAN_POINT('Ctrl Pts',(-3.68934341946097,-2.59251129104238,
4.40728868514835));
#21427=CARTESIAN_POINT('Ctrl Pts',(-3.81019440079089,-2.42934431729619,
4.39617489609154));
#21428=CARTESIAN_POINT('Ctrl Pts',(-3.73865169972831,-2.23931987716506,
4.38506110703474));
#21429=CARTESIAN_POINT('Ctrl Pts',(-3.54020025351852,-2.19636433155117,
4.37394731797794));
#21430=CARTESIAN_POINT('Ctrl Pts',(-3.39648273563768,-2.33980571917207,
4.36283352892113));
#21431=CARTESIAN_POINT('Ctrl Pts',(-3.43904979696867,-2.53832980517198,
4.35171973986433));
#21432=CARTESIAN_POINT('Ctrl Pts',(-3.6289305590181,-2.6102667040308,4.34060595080752));
#21433=CARTESIAN_POINT('Ctrl Pts',(-3.79234256052004,-2.48968872907629,
4.32949216175072));
#21434=CARTESIAN_POINT('Ctrl Pts',(-3.77967774525388,-2.28712858487203,
4.31837837269391));
#21435=CARTESIAN_POINT('Ctrl Pts',(-3.60259952841706,-2.18765796465806,
4.30726458363711));
#21436=CARTESIAN_POINT('Ctrl Pts',(-3.42303934432415,-2.28300298030457,
4.29615079458031));
#21437=CARTESIAN_POINT('Ctrl Pts',(-3.41156124805061,-2.41723390733863,
4.28874160187577));
#21438=CARTESIAN_POINT('Ctrl Pts',(-3.43548292594103,-2.47193974848801,
4.2850370055235));
#21439=CARTESIAN_POINT('Ctrl Pts',(-3.45335096305347,-2.2752733913429,5.2149629944765));
#21440=CARTESIAN_POINT('Ctrl Pts',(-3.41187639830495,-2.32403768505403,
5.21125839812423));
#21441=CARTESIAN_POINT('Ctrl Pts',(-3.38215243645823,-2.46538954577948,
5.20384920541969));
#21442=CARTESIAN_POINT('Ctrl Pts',(-3.53700737368693,-2.61879588637947,
5.19273541636289));
#21443=CARTESIAN_POINT('Ctrl Pts',(-3.74955603736419,-2.571435436671,5.18162162730609));
#21444=CARTESIAN_POINT('Ctrl Pts',(-3.82519436350635,-2.3674018251774,5.17050783824928));
#21445=CARTESIAN_POINT('Ctrl Pts',(-3.69471992586929,-2.19308453561,5.15939404919247));
#21446=CARTESIAN_POINT('Ctrl Pts',(-3.47754216233122,-2.20821978609556,
5.14828026013568));
#21447=CARTESIAN_POINT('Ctrl Pts',(-3.37245399619058,-2.39886344568463,
5.13716647107886));
#21448=CARTESIAN_POINT('Ctrl Pts',(-3.47563999441657,-2.59056248594111,
5.12605268202207));
#21449=CARTESIAN_POINT('Ctrl Pts',(-3.69265475207253,-2.60782999088153,
5.11493889296526));
#21450=CARTESIAN_POINT('Ctrl Pts',(-3.82486124676799,-2.434872109133,5.10382510390846));
#21451=CARTESIAN_POINT('Ctrl Pts',(-3.75124985081366,-2.22999351220008,
5.09271131485165));
#21452=CARTESIAN_POINT('Ctrl Pts',(-3.53919767190563,-2.18072471954551,
5.08159752579485));
#21453=CARTESIAN_POINT('Ctrl Pts',(-3.38279859300748,-2.33216060940528,
5.07048373673804));
#21454=CARTESIAN_POINT('Ctrl Pts',(-3.42520640540474,-2.54569089676662,
5.05936994768124));
#21455=CARTESIAN_POINT('Ctrl Pts',(-3.62760478709563,-2.62586853724007,
5.04825615862444));
#21456=CARTESIAN_POINT('Ctrl Pts',(-3.80473618917098,-2.49930620239979,
5.03714236956763));
#21457=CARTESIAN_POINT('Ctrl Pts',(-3.79447023789256,-2.28184774515603,
5.02602858051083));
#21458=CARTESIAN_POINT('Ctrl Pts',(-3.60620347119968,-2.17253540126032,
5.01491479145402));
#21459=CARTESIAN_POINT('Ctrl Pts',(-3.4122585975793,-2.27142397694788,5.00380100239722));
#21460=CARTESIAN_POINT('Ctrl Pts',(-3.39015555842041,-2.48799964831557,
4.99268721334041));
#21461=CARTESIAN_POINT('Ctrl Pts',(-3.56012551659021,-2.62402824178367,
4.98157342428361));
#21462=CARTESIAN_POINT('Ctrl Pts',(-3.76659304155595,-2.55500124579927,
4.97045963522681));
#21463=CARTESIAN_POINT('Ctrl Pts',(-3.82057606633011,-2.34409985124907,
4.95934584617));
#21464=CARTESIAN_POINT('Ctrl Pts',(-3.67266331607053,-2.18436449702716,
4.9482320571132));
#21465=CARTESIAN_POINT('Ctrl Pts',(-3.45824100856306,-2.22200276403647,
4.93711826805639));
#21466=CARTESIAN_POINT('Ctrl Pts',(-3.37357231356937,-2.42256391980546,
4.92600447899959));
#21467=CARTESIAN_POINT('Ctrl Pts',(-3.49615544783263,-2.60247206385614,
4.91489068994279));
#21468=CARTESIAN_POINT('Ctrl Pts',(-3.71378867837081,-2.59705523168396,
4.90377690088598));
#21469=CARTESIAN_POINT('Ctrl Pts',(-3.82726984114541,-2.41127151118611,
4.89266311182918));
#21470=CARTESIAN_POINT('Ctrl Pts',(-3.73272834090401,-2.21517084867549,
4.88154932277237));
#21471=CARTESIAN_POINT('Ctrl Pts',(-3.51669908499156,-2.18824640447558,
4.87043553371557));
#21472=CARTESIAN_POINT('Ctrl Pts',(-3.37691610128289,-2.35514242770916,
4.85932174465877));
#21473=CARTESIAN_POINT('Ctrl Pts',(-3.44132434001351,-2.56309709557957,
4.84820795560196));
#21474=CARTESIAN_POINT('Ctrl Pts',(-3.65097020983412,-2.62176714221935,
4.83709416654516));
#21475=CARTESIAN_POINT('Ctrl Pts',(-3.81396246855208,-2.47745120857521,
4.82598037748835));
#21476=CARTESIAN_POINT('Ctrl Pts',(-3.78111245330488,-2.26224330536578,
4.81486658843155));
#21477=CARTESIAN_POINT('Ctrl Pts',(-3.58248815559281,-2.1731256670222,4.80375279937474));
#21478=CARTESIAN_POINT('Ctrl Pts',(-3.39989264766446,-2.29166867858314,
4.79263901031794));
#21479=CARTESIAN_POINT('Ctrl Pts',(-3.40045766870055,-2.50936857719767,
4.78152522126113));
#21480=CARTESIAN_POINT('Ctrl Pts',(-3.58366604853898,-2.62696217677915,
4.77041143220433));
#21481=CARTESIAN_POINT('Ctrl Pts',(-3.78182507938928,-2.53681472202852,
4.75929764314753));
#21482=CARTESIAN_POINT('Ctrl Pts',(-3.81355755303793,-2.32143920062071,
4.74818385409072));
#21483=CARTESIAN_POINT('Ctrl Pts',(-3.64981837648358,-2.17797126982482,
4.73707006503392));
#21484=CARTESIAN_POINT('Ctrl Pts',(-3.440479874955,-2.23772875373533,4.72595627597712));
#21485=CARTESIAN_POINT('Ctrl Pts',(-3.37715195296136,-2.44601494963299,
4.71484248692031));
#21486=CARTESIAN_POINT('Ctrl Pts',(-3.51779937569094,-2.61218314028655,
4.7037286978635));
#21487=CARTESIAN_POINT('Ctrl Pts',(-3.73368596206909,-2.58413769631535,
4.69261490880671));
#21488=CARTESIAN_POINT('Ctrl Pts',(-3.82720827126346,-2.38754893064322,
4.68150111974989));
#21489=CARTESIAN_POINT('Ctrl Pts',(-3.71276427305336,-2.20235676995803,
4.6703873306931));
#21490=CARTESIAN_POINT('Ctrl Pts',(-3.49510585688365,-2.19806969915704,
4.65927354163628));
#21491=CARTESIAN_POINT('Ctrl Pts',(-3.37345823948888,-2.37861172276277,
4.64815975257949));
#21492=CARTESIAN_POINT('Ctrl Pts',(-3.45916686464814,-2.57873067908372,
4.63704596352267));
#21493=CARTESIAN_POINT('Ctrl Pts',(-3.67378165575153,-2.61525541789472,
4.62593217446588));
#21494=CARTESIAN_POINT('Ctrl Pts',(-3.82086326060429,-2.45475443154594,
4.61481838540906));
#21495=CARTESIAN_POINT('Ctrl Pts',(-3.76578621826694,-2.24413609304223,
4.60370459635227));
#21496=CARTESIAN_POINT('Ctrl Pts',(-3.55896317020481,-2.17618175620078,
4.59259080729546));
#21497=CARTESIAN_POINT('Ctrl Pts',(-3.38970159784644,-2.3130907961665,4.58147701823866));
#21498=CARTESIAN_POINT('Ctrl Pts',(-3.41292853791948,-2.52954881604603,
4.57036322918185));
#21499=CARTESIAN_POINT('Ctrl Pts',(-3.60738410878117,-2.62742933535986,
4.55924944012506));
#21500=CARTESIAN_POINT('Ctrl Pts',(-3.79508092111058,-2.51714120490541,
4.54813565106824));
#21501=CARTESIAN_POINT('Ctrl Pts',(-3.8042179540262,-2.29963240090777,4.53702186201145));
#21502=CARTESIAN_POINT('Ctrl Pts',(-3.62643197753871,-2.17399119904908,
4.52590807295463));
#21503=CARTESIAN_POINT('Ctrl Pts',(-3.42445251243888,-2.25521841492616,
4.51479428389784));
#21504=CARTESIAN_POINT('Ctrl Pts',(-3.38315365317149,-2.46896585933577,
4.50368049484102));
#21505=CARTESIAN_POINT('Ctrl Pts',(-3.54033671511431,-2.61958806700588,
4.49256670578423));
#21506=CARTESIAN_POINT('Ctrl Pts',(-3.75213025683239,-2.56921883378282,
4.48145291672742));
#21507=CARTESIAN_POINT('Ctrl Pts',(-3.82467725221749,-2.3639616686385,4.47033912767062));
#21508=CARTESIAN_POINT('Ctrl Pts',(-3.69157460458704,-2.1916908255014,4.45922533861381));
#21509=CARTESIAN_POINT('Ctrl Pts',(-3.47465269496093,-2.21008767488223,
4.44811154955701));
#21510=CARTESIAN_POINT('Ctrl Pts',(-3.37246257092429,-2.40231354390696,
4.4369977605002));
#21511=CARTESIAN_POINT('Ctrl Pts',(-3.47854008472427,-2.59242157025994,
4.4258839714434));
#21512=CARTESIAN_POINT('Ctrl Pts',(-3.69579113920209,-2.60640441108558,
4.41477018238659));
#21513=CARTESIAN_POINT('Ctrl Pts',(-3.82536367230107,-2.43146203268096,
4.4036563933298));
#21514=CARTESIAN_POINT('Ctrl Pts',(-3.74865789052413,-2.22772394311352,
4.39254260427298));
#21515=CARTESIAN_POINT('Ctrl Pts',(-3.53588463622708,-2.18166838945074,
4.38142881521619));
#21516=CARTESIAN_POINT('Ctrl Pts',(-3.38179533850196,-2.33546162919725,
4.37031502615938));
#21517=CARTESIAN_POINT('Ctrl Pts',(-3.42743437181836,-2.54831276553967,
4.35920123710258));
#21518=CARTESIAN_POINT('Ctrl Pts',(-3.63101841437027,-2.62544119350812,
4.34808744804577));
#21519=CARTESIAN_POINT('Ctrl Pts',(-3.80622350364941,-2.49616136905929,
4.33697365898897));
#21520=CARTESIAN_POINT('Ctrl Pts',(-3.7926446962851,-2.27898290099381,4.32585986993216));
#21521=CARTESIAN_POINT('Ctrl Pts',(-3.60278713071383,-2.17233370304593,
4.31474608087535));
#21522=CARTESIAN_POINT('Ctrl Pts',(-3.4102684797223,-2.27455956054189,4.30363229181856));
#21523=CARTESIAN_POINT('Ctrl Pts',(-3.3979620342723,-2.41847764084731,4.29622309911402));
#21524=CARTESIAN_POINT('Ctrl Pts',(-3.42361008748733,-2.47713148324918,
4.29251850276175));
#21525=CARTESIAN_POINT('Ctrl Pts',(-3.44347998857283,-2.26687801966678,
5.22244449171475));
#21526=CARTESIAN_POINT('Ctrl Pts',(-3.39921376300775,-2.31892464723302,
5.21873989536248));
#21527=CARTESIAN_POINT('Ctrl Pts',(-3.36748907565365,-2.46979092850336,
5.21133070265795));
#21528=CARTESIAN_POINT('Ctrl Pts',(-3.53276732806678,-2.63352307897406,
5.20021691360113));
#21529=CARTESIAN_POINT('Ctrl Pts',(-3.75962268259409,-2.58297478841644,
5.18910312454434));
#21530=CARTESIAN_POINT('Ctrl Pts',(-3.84035223880946,-2.36520763584968,
5.17798933548753));
#21531=CARTESIAN_POINT('Ctrl Pts',(-3.70109554203788,-2.17915701647198,
5.16687554643073));
#21532=CARTESIAN_POINT('Ctrl Pts',(-3.46929950206046,-2.19531102353728,
5.15576175737392));
#21533=CARTESIAN_POINT('Ctrl Pts',(-3.35713783153282,-2.39878694399818,
5.14464796831711));
#21534=CARTESIAN_POINT('Ctrl Pts',(-3.46726929886284,-2.60338928299931,
5.13353417926032));
#21535=CARTESIAN_POINT('Ctrl Pts',(-3.69889136100131,-2.62181906697108,
5.12242039020351));
#21536=CARTESIAN_POINT('Ctrl Pts',(-3.83999669992028,-2.43721935741029,
5.1113066011467));
#21537=CARTESIAN_POINT('Ctrl Pts',(-3.76143050694799,-2.21855034327406,
5.10019281208991));
#21538=CARTESIAN_POINT('Ctrl Pts',(-3.53510505567384,-2.16596525884485,
5.0890790230331));
#21539=CARTESIAN_POINT('Ctrl Pts',(-3.36817872512274,-2.32759432716241,
5.07796523397629));
#21540=CARTESIAN_POINT('Ctrl Pts',(-3.41344101541272,-2.5554973786501,5.06685144491949));
#21541=CARTESIAN_POINT('Ctrl Pts',(-3.62946287054873,-2.64107179130501,
5.05573765586269));
#21542=CARTESIAN_POINT('Ctrl Pts',(-3.81851702088083,-2.50599052171118,
5.04462386680588));
#21543=CARTESIAN_POINT('Ctrl Pts',(-3.8075600664755,-2.27389489448153,5.03351007774907));
#21544=CARTESIAN_POINT('Ctrl Pts',(-3.60662102802227,-2.15722471599323,
5.02239628869228));
#21545=CARTESIAN_POINT('Ctrl Pts',(-3.39962168818772,-2.262769500459,5.01128249963546));
#21546=CARTESIAN_POINT('Ctrl Pts',(-3.37603088927244,-2.49392292132789,
5.00016871057867));
#21547=CARTESIAN_POINT('Ctrl Pts',(-3.55744155755193,-2.63910762521254,
4.98905492152185));
#21548=CARTESIAN_POINT('Ctrl Pts',(-3.77780645076812,-2.56543440904132,
4.97794113246506));
#21549=CARTESIAN_POINT('Ctrl Pts',(-3.83542308317469,-2.34033720163832,
4.96682734340825));
#21550=CARTESIAN_POINT('Ctrl Pts',(-3.67755429765177,-2.16985003043886,
4.95571355435145));
#21551=CARTESIAN_POINT('Ctrl Pts',(-3.44869918397279,-2.21002173633656,
4.94459976529464));
#21552=CARTESIAN_POINT('Ctrl Pts',(-3.3583314230664,-2.42408270152555,4.93348597623784));
#21553=CARTESIAN_POINT('Ctrl Pts',(-3.48916565133794,-2.61610049686178,
4.92237218718103));
#21554=CARTESIAN_POINT('Ctrl Pts',(-3.7214478158856,-2.61031905668909,4.91125839812423));
#21555=CARTESIAN_POINT('Ctrl Pts',(-3.8425674172419,-2.41203019874106,4.90014460906743));
#21556=CARTESIAN_POINT('Ctrl Pts',(-3.74166231069475,-2.20272996345734,
4.88903082001062));
#21557=CARTESIAN_POINT('Ctrl Pts',(-3.511092084609,-2.17399322981363,4.87791703095382));
#21558=CARTESIAN_POINT('Ctrl Pts',(-3.36190028176488,-2.35212305601353,
4.86680324189701));
#21559=CARTESIAN_POINT('Ctrl Pts',(-3.43064385125587,-2.57407519200526,
4.85568945284021));
#21560=CARTESIAN_POINT('Ctrl Pts',(-3.6544010243217,-2.63669433060785,4.84457566378341));
#21561=CARTESIAN_POINT('Ctrl Pts',(-3.82836432287631,-2.48266446410869,
4.8334618747266));
#21562=CARTESIAN_POINT('Ctrl Pts',(-3.79330316687467,-2.25297087613211,
4.8223480856698));
#21563=CARTESIAN_POINT('Ctrl Pts',(-3.58130943002562,-2.15785471265546,
4.81123429661298));
#21564=CARTESIAN_POINT('Ctrl Pts',(-3.38642338383962,-2.28437687679961,
4.8001205075562));
#21565=CARTESIAN_POINT('Ctrl Pts',(-3.38702643654876,-2.51673019686447,
4.78900671849938));
#21566=CARTESIAN_POINT('Ctrl Pts',(-3.58256660716932,-2.64223904392882,
4.77789292944258));
#21567=CARTESIAN_POINT('Ctrl Pts',(-3.79406375995591,-2.54602374690751,
4.76677914038577));
#21568=CARTESIAN_POINT('Ctrl Pts',(-3.82793215242214,-2.31615125831984,
4.75566535132897));
#21569=CARTESIAN_POINT('Ctrl Pts',(-3.65317166084996,-2.16302647390142,
4.74455156227217));
#21570=CARTESIAN_POINT('Ctrl Pts',(-3.42974254509416,-2.22680624538361,
4.73343777321536));
#21571=CARTESIAN_POINT('Ctrl Pts',(-3.36215200866455,-2.44911222461694,
4.72232398415856));
#21572=CARTESIAN_POINT('Ctrl Pts',(-3.51226643608395,-2.62646522768789,
4.71121019510176));
#21573=CARTESIAN_POINT('Ctrl Pts',(-3.74268438952201,-2.59653203956573,
4.70009640604495));
#21574=CARTESIAN_POINT('Ctrl Pts',(-3.84250170307953,-2.38671084680417,
4.68898261698815));
#21575=CARTESIAN_POINT('Ctrl Pts',(-3.72035445765201,-2.18905336667194,
4.67786882793134));
#21576=CARTESIAN_POINT('Ctrl Pts',(-3.4880454122232,-2.18447773232253,4.66675503887454));
#21577=CARTESIAN_POINT('Ctrl Pts',(-3.35820967063793,-2.37717207376684,
4.65564124981773));
#21578=CARTESIAN_POINT('Ctrl Pts',(-3.4496873596065,-2.5907610749791,4.64452746076093));
#21579=CARTESIAN_POINT('Ctrl Pts',(-3.67874791298872,-2.62974430088435,
4.63341367170412));
#21580=CARTESIAN_POINT('Ctrl Pts',(-3.83572960854991,-2.4584399627144,4.62229988264733));
#21581=CARTESIAN_POINT('Ctrl Pts',(-3.77694532005055,-2.23364486391404,
4.61118609359051));
#21582=CARTESIAN_POINT('Ctrl Pts',(-3.55620097341096,-2.16111650777606,
4.60007230453371));
#21583=CARTESIAN_POINT('Ctrl Pts',(-3.37554637252617,-2.307240921179,4.58895851547691));
#21584=CARTESIAN_POINT('Ctrl Pts',(-3.40033672233922,-2.53826877141577,
4.57784472642011));
#21585=CARTESIAN_POINT('Ctrl Pts',(-3.60788113454322,-2.64273764704216,
4.5667309373633));
#21586=CARTESIAN_POINT('Ctrl Pts',(-3.8082118548967,-2.52502600161686,4.5556171483065));
#21587=CARTESIAN_POINT('Ctrl Pts',(-3.8179639032302,-2.29287663878378,4.54450335924969));
#21588=CARTESIAN_POINT('Ctrl Pts',(-3.62821111895818,-2.15877850380716,
4.53338957019289));
#21589=CARTESIAN_POINT('Ctrl Pts',(-3.4126363777684,-2.24547313898512,4.52227578113608));
#21590=CARTESIAN_POINT('Ctrl Pts',(-3.3685576844537,-2.47360796440317,4.51116199207928));
#21591=CARTESIAN_POINT('Ctrl Pts',(-3.53632076809686,-2.63436858142862,
4.50004820302248));
#21592=CARTESIAN_POINT('Ctrl Pts',(-3.76237017326276,-2.5806089855676,4.48893441396567));
#21593=CARTESIAN_POINT('Ctrl Pts',(-3.83980032066171,-2.36153592172191,
4.47782062490887));
#21594=CARTESIAN_POINT('Ctrl Pts',(-3.69773850858379,-2.17766949547173,
4.46670683585206));
#21595=CARTESIAN_POINT('Ctrl Pts',(-3.46621554409366,-2.19730464027232,
4.45559304679525));
#21596=CARTESIAN_POINT('Ctrl Pts',(-3.35714698343348,-2.40246926898597,
4.44447925773846));
#21597=CARTESIAN_POINT('Ctrl Pts',(-3.47036459479899,-2.60537350263611,
4.43336546868164));
#21598=CARTESIAN_POINT('Ctrl Pts',(-3.70223885894321,-2.62029753112878,
4.42225167962485));
#21599=CARTESIAN_POINT('Ctrl Pts',(-3.84053294381125,-2.43357974806573,
4.41113789056804));
#21600=CARTESIAN_POINT('Ctrl Pts',(-3.75866408131995,-2.21612800906199,
4.40002410151124));
#21601=CARTESIAN_POINT('Ctrl Pts',(-3.53156901893564,-2.16697244735031,
4.38891031245443));
#21602=CARTESIAN_POINT('Ctrl Pts',(-3.36710794136624,-2.33111753922242,
4.37779652339762));
#21603=CARTESIAN_POINT('Ctrl Pts',(-3.41581894666805,-2.55829572590735,
4.36668273434083));
#21604=CARTESIAN_POINT('Ctrl Pts',(-3.63310626972243,-2.64061568298545,
4.35556894528402));
#21605=CARTESIAN_POINT('Ctrl Pts',(-3.82010444677879,-2.50263400904229,
4.34445515622722));
#21606=CARTESIAN_POINT('Ctrl Pts',(-3.80561164731632,-2.27083721711559,
4.33334136717041));
#21607=CARTESIAN_POINT('Ctrl Pts',(-3.60297473301061,-2.15700944143379,
4.32222757811361));
#21608=CARTESIAN_POINT('Ctrl Pts',(-3.39749761512046,-2.26611614077921,
4.3111137890568));
#21609=CARTESIAN_POINT('Ctrl Pts',(-3.38436282049399,-2.419721374356,4.30370459635227));
#21610=CARTESIAN_POINT('Ctrl Pts',(-3.41173724903364,-2.48232321801035,
4.3));
#21611=CARTESIAN_POINT('Ctrl Pts',(-3.47309291201476,-2.29206413469515,
5.2));
#21612=CARTESIAN_POINT('Ctrl Pts',(-3.46488110023315,-2.2997248835417,5.2));
#21613=CARTESIAN_POINT('Ctrl Pts',(-3.45756393061001,-2.3082260406838,5.2));
#21614=CARTESIAN_POINT('Ctrl Pts',(-3.45114583189458,-2.31737340047652,
5.2));
#21615=CARTESIAN_POINT('Ctrl Pts',(-3.44637506584917,-2.32417290846779,
5.2));
#21616=CARTESIAN_POINT('Ctrl Pts',(-3.44210141208336,-2.33133076253531,
5.2));
#21617=CARTESIAN_POINT('Ctrl Pts',(-3.43833687158849,-2.33878162457801,
5.2));
#21618=CARTESIAN_POINT('Ctrl Pts',(-3.43611957198332,-2.34317015313494,
5.2));
#21619=CARTESIAN_POINT('Ctrl Pts',(-3.43407750155671,-2.34766554493455,
5.2));
#21620=CARTESIAN_POINT('Ctrl Pts',(-3.43222557143088,-2.35222601439271,
5.2));
#21621=CARTESIAN_POINT('Ctrl Pts',(-3.42766723914997,-2.36345113290954,
5.2));
#21622=CARTESIAN_POINT('Ctrl Pts',(-3.42424191788099,-2.37509439510727,
5.2));
#21623=CARTESIAN_POINT('Ctrl Pts',(-3.42197769676804,-2.38695730471617,
5.2));
#21624=CARTESIAN_POINT('Ctrl Pts',(-3.42053881602809,-2.39449601728207,
5.2));
#21625=CARTESIAN_POINT('Ctrl Pts',(-3.41956956713255,-2.40212431376417,
5.2));
#21626=CARTESIAN_POINT('Ctrl Pts',(-3.41908672349853,-2.40979637190619,
5.2));
#21627=CARTESIAN_POINT('Ctrl Pts',(-3.4188613967758,-2.41337666083611,5.2));
#21628=CARTESIAN_POINT('Ctrl Pts',(-3.41874254028701,-2.41696303084227,
5.2));
#21629=CARTESIAN_POINT('Ctrl Pts',(-3.4187313001846,-2.42054068183377,5.2));
#21630=CARTESIAN_POINT('Ctrl Pts',(-3.41869625236243,-2.43169617411961,
5.2));
#21631=CARTESIAN_POINT('Ctrl Pts',(-3.41970314531555,-2.44279404991157,
5.2));
#21632=CARTESIAN_POINT('Ctrl Pts',(-3.4217856982914,-2.45369315923086,5.2));
#21633=CARTESIAN_POINT('Ctrl Pts',(-3.42294608022389,-2.45976605614203,
5.2));
#21634=CARTESIAN_POINT('Ctrl Pts',(-3.42444095669484,-2.46577748192705,
5.2));
#21635=CARTESIAN_POINT('Ctrl Pts',(-3.42625159798616,-2.47171129566944,
5.2));
#21636=CARTESIAN_POINT('Ctrl Pts',(-3.42738424188737,-2.4754231838156,5.2));
#21637=CARTESIAN_POINT('Ctrl Pts',(-3.4286411006463,-2.47910621955531,5.2));
#21638=CARTESIAN_POINT('Ctrl Pts',(-3.43001647345192,-2.48275158788973,
5.2));
#21639=CARTESIAN_POINT('Ctrl Pts',(-3.43439826051469,-2.49436533198986,
5.2));
#21640=CARTESIAN_POINT('Ctrl Pts',(-3.43994736167241,-2.50551615790537,
5.2));
#21641=CARTESIAN_POINT('Ctrl Pts',(-3.44649835855225,-2.51608152365555,
5.2));
#21642=CARTESIAN_POINT('Ctrl Pts',(-3.45083933347942,-2.52308259366964,
5.2));
#21643=CARTESIAN_POINT('Ctrl Pts',(-3.45562142913928,-2.5298267361278,5.2));
#21644=CARTESIAN_POINT('Ctrl Pts',(-3.46080806253422,-2.53627607801171,
5.2));
#21645=CARTESIAN_POINT('Ctrl Pts',(-3.46351819008795,-2.53964599792162,
5.2));
#21646=CARTESIAN_POINT('Ctrl Pts',(-3.46634016652161,-2.54293674743321,
5.2));
#21647=CARTESIAN_POINT('Ctrl Pts',(-3.46926561316249,-2.5461381198978,5.2));
#21648=CARTESIAN_POINT('Ctrl Pts',(-3.47553204021621,-2.55299559141714,
5.2));
#21649=CARTESIAN_POINT('Ctrl Pts',(-3.48224800724127,-2.55941730873493,
5.2));
#21650=CARTESIAN_POINT('Ctrl Pts',(-3.48935943070669,-2.56535251864156,
5.2));
#21651=CARTESIAN_POINT('Ctrl Pts',(-3.49388595591638,-2.56913036669094,
5.2));
#21652=CARTESIAN_POINT('Ctrl Pts',(-3.49857295100653,-2.57271103243443,
5.2));
#21653=CARTESIAN_POINT('Ctrl Pts',(-3.50340866428261,-2.5760800097667,5.2));
#21654=CARTESIAN_POINT('Ctrl Pts',(-3.50748115648314,-2.57891726109367,
5.2));
#21655=CARTESIAN_POINT('Ctrl Pts',(-3.51165212725609,-2.58159933242901,
5.2));
#21656=CARTESIAN_POINT('Ctrl Pts',(-3.51591076075252,-2.58411660325874,
5.2));
#21657=CARTESIAN_POINT('Ctrl Pts',(-3.52463384142318,-2.58927280102407,
5.2));
#21658=CARTESIAN_POINT('Ctrl Pts',(-3.53372795938425,-2.593741186929,5.2));
#21659=CARTESIAN_POINT('Ctrl Pts',(-3.54313434616876,-2.59744798259885,
5.2));
#21660=CARTESIAN_POINT('Ctrl Pts',(-3.54437365456163,-2.59793635960157,
5.2));
#21661=CARTESIAN_POINT('Ctrl Pts',(-3.54561839868079,-2.59841149645932,
5.2));
#21662=CARTESIAN_POINT('Ctrl Pts',(-3.54686838721289,-2.59887345127292,
5.2));
#21663=CARTESIAN_POINT('Ctrl Pts',(-3.76673281282141,-2.40013003219325,
5.08714803633902));
#21664=CARTESIAN_POINT('Ctrl Pts',(-3.76680596527292,-2.4086546123928,5.08771939403667));
#21665=CARTESIAN_POINT('Ctrl Pts',(-3.76620865763489,-2.417168907206,5.08829075173431));
#21666=CARTESIAN_POINT('Ctrl Pts',(-3.76490523910227,-2.42557368984471,
5.08886210943196));
#21667=CARTESIAN_POINT('Ctrl Pts',(-3.75645407171393,-2.48006902128643,
5.09256670578423));
#21668=CARTESIAN_POINT('Ctrl Pts',(-3.71831780296444,-2.52996042999443,
5.09627130213649));
#21669=CARTESIAN_POINT('Ctrl Pts',(-3.66794964380788,-2.55241564320215,
5.09997589848876));
#21670=CARTESIAN_POINT('Ctrl Pts',(-3.61758148465131,-2.57487085640986,
5.10368049484103));
#21671=CARTESIAN_POINT('Ctrl Pts',(-3.55498143508767,-2.56988987411729,
5.1073850911933));
#21672=CARTESIAN_POINT('Ctrl Pts',(-3.50879890030286,-2.53975064250981,
5.11108968754557));
#21673=CARTESIAN_POINT('Ctrl Pts',(-3.46261636551805,-2.50961141090233,
5.11479428389784));
#21674=CARTESIAN_POINT('Ctrl Pts',(-3.43285134551208,-2.45431392997993,
5.1184988802501));
#21675=CARTESIAN_POINT('Ctrl Pts',(-3.4331256950702,-2.3991686665445,5.12220347660237));
#21676=CARTESIAN_POINT('Ctrl Pts',(-3.43340004462832,-2.34402340310906,
5.12590807295464));
#21677=CARTESIAN_POINT('Ctrl Pts',(-3.46371376375052,-2.28903035716059,
5.12961266930691));
#21678=CARTESIAN_POINT('Ctrl Pts',(-3.51019415842152,-2.25935087796534,
5.13331726565918));
#21679=CARTESIAN_POINT('Ctrl Pts',(-3.55667455309252,-2.22967139877009,
5.13702186201145));
#21680=CARTESIAN_POINT('Ctrl Pts',(-3.61932162331232,-2.22530548632806,
5.14072645836371));
#21681=CARTESIAN_POINT('Ctrl Pts',(-3.66946347831689,-2.24826430176485,
5.14443105471598));
#21682=CARTESIAN_POINT('Ctrl Pts',(-3.71960533332146,-2.27122311720164,
5.14813565106825));
#21683=CARTESIAN_POINT('Ctrl Pts',(-3.7572419731108,-2.32150666051725,5.15184024742051));
#21684=CARTESIAN_POINT('Ctrl Pts',(-3.76515098200617,-2.37607618706626,
5.15554484377278));
#21685=CARTESIAN_POINT('Ctrl Pts',(-3.76629187681735,-2.3839479811825,5.15607924129486));
#21686=CARTESIAN_POINT('Ctrl Pts',(-3.7668141752375,-2.39190896147606,5.15661363881694));
#21687=CARTESIAN_POINT('Ctrl Pts',(-3.76674783764939,-2.3998784327954,5.15714803633902));
#21688=CARTESIAN_POINT('Ctrl Pts',(-3.65301702171886,-2.59851743256717,
5.2));
#21689=CARTESIAN_POINT('Ctrl Pts',(-3.71902879097456,-2.58088801151799,
5.19629540364773));
#21690=CARTESIAN_POINT('Ctrl Pts',(-3.83093278328674,-2.47484748886485,
5.1888862109432));
#21691=CARTESIAN_POINT('Ctrl Pts',(-3.78812295700318,-2.24617213689742,
5.17777242188639));
#21692=CARTESIAN_POINT('Ctrl Pts',(-3.5727867642971,-2.15871465280967,5.16665863282959));
#21693=CARTESIAN_POINT('Ctrl Pts',(-3.38252461999799,-2.29190667528476,
5.15554484377278));
#21694=CARTESIAN_POINT('Ctrl Pts',(-3.39123766053156,-2.52413789941101,
5.14443105471598));
#21695=CARTESIAN_POINT('Ctrl Pts',(-3.59107442597796,-2.64269432067786,
5.13331726565918));
#21696=CARTESIAN_POINT('Ctrl Pts',(-3.79906030223171,-2.53913483234337,
5.12220347660237));
#21697=CARTESIAN_POINT('Ctrl Pts',(-3.82485429799751,-2.30821119218956,
5.11108968754557));
#21698=CARTESIAN_POINT('Ctrl Pts',(-3.64483147519039,-2.16130911215383,
5.09997589848876));
#21699=CARTESIAN_POINT('Ctrl Pts',(-3.42377645640768,-2.23288040078699,
5.08886210943196));
#21700=CARTESIAN_POINT('Ctrl Pts',(-3.36401956629289,-2.45741970591997,
5.07774832037515));
#21701=CARTESIAN_POINT('Ctrl Pts',(-3.52025888222192,-2.62940132794335,
5.06663453131835));
#21702=CARTESIAN_POINT('Ctrl Pts',(-3.74948582853024,-2.5914096999913,5.05552074226155));
#21703=CARTESIAN_POINT('Ctrl Pts',(-3.84188686003135,-2.37821840959849,
5.04440695320474));
#21704=CARTESIAN_POINT('Ctrl Pts',(-3.71288602579316,-2.18496415245566,
5.03329316414794));
#21705=CARTESIAN_POINT('Ctrl Pts',(-3.4805593716682,-2.1885345970333,5.02217937509112));
#21706=CARTESIAN_POINT('Ctrl Pts',(-3.35755805936012,-2.38566174720256,
5.01106558603434));
#21707=CARTESIAN_POINT('Ctrl Pts',(-3.45646661470834,-2.59591285074103,
4.99995179697752));
#21708=CARTESIAN_POINT('Ctrl Pts',(-3.68675290044432,-2.62684270619768,
4.98883800792072));
#21709=CARTESIAN_POINT('Ctrl Pts',(-3.83763327503031,-2.45014085710183,
4.97772421886392));
#21710=CARTESIAN_POINT('Ctrl Pts',(-3.77100521680217,-2.22754451436212,
4.96661042980711));
#21711=CARTESIAN_POINT('Ctrl Pts',(-3.54785414492032,-2.16279863265717,
4.9554966407503));
#21712=CARTESIAN_POINT('Ctrl Pts',(-3.37243276525931,-2.31516585290104,
4.94438285169351));
#21713=CARTESIAN_POINT('Ctrl Pts',(-3.40530625649813,-2.54518272988275,
4.9332690626367));
#21714=CARTESIAN_POINT('Ctrl Pts',(-3.61638513906469,-2.64231220781178,
4.9221552735799));
#21715=CARTESIAN_POINT('Ctrl Pts',(-3.81246651806354,-2.51765057387683,
4.91104148452309));
#21716=CARTESIAN_POINT('Ctrl Pts',(-3.81407488352551,-2.2853020354474,4.89992769546629));
#21717=CARTESIAN_POINT('Ctrl Pts',(-3.61973808033182,-2.15793784472475,
4.88881390640949));
#21718=CARTESIAN_POINT('Ctrl Pts',(-3.4073347883606,-2.25213588990288,4.87770011735268));
#21719=CARTESIAN_POINT('Ctrl Pts',(-3.37128014957741,-2.48167563194308,
4.86658632829587));
#21720=CARTESIAN_POINT('Ctrl Pts',(-3.54457538374435,-2.63645674180255,
4.85547253923907));
#21721=CARTESIAN_POINT('Ctrl Pts',(-3.76860139772859,-2.57480631428759,
4.84435875018227));
#21722=CARTESIAN_POINT('Ctrl Pts',(-3.83830464030165,-2.35315368486712,
4.83324496112546));
#21723=CARTESIAN_POINT('Ctrl Pts',(-3.68988494304833,-2.17438001896094,
4.82213117206866));
#21724=CARTESIAN_POINT('Ctrl Pts',(-3.45919253805822,-2.20211888040452,
4.81101738301185));
#21725=CARTESIAN_POINT('Ctrl Pts',(-3.35738279984868,-2.41098057473832,
4.79990359395505));
#21726=CARTESIAN_POINT('Ctrl Pts',(-3.47764333640382,-2.60979162448597,
4.78878980489824));
#21727=CARTESIAN_POINT('Ctrl Pts',(-3.7098983147675,-2.61657802114276,4.77767601584144));
#21728=CARTESIAN_POINT('Ctrl Pts',(-3.84156211929281,-2.42512809888577,
4.76656222678463));
#21729=CARTESIAN_POINT('Ctrl Pts',(-3.75212137652867,-2.21067814274661,
4.75544843772783));
#21730=CARTESIAN_POINT('Ctrl Pts',(-3.52344221265408,-2.16951662960737,
4.74433464867103));
#21731=CARTESIAN_POINT('Ctrl Pts',(-3.36483725976158,-2.33931915924769,
4.73322085961422));
#21732=CARTESIAN_POINT('Ctrl Pts',(-3.42147942993616,-2.56466355059616,
4.72210707055742));
#21733=CARTESIAN_POINT('Ctrl Pts',(-3.64152350245114,-2.63928952667227,
4.71099328150061));
#21734=CARTESIAN_POINT('Ctrl Pts',(-3.82356064226404,-2.49489108525746,
4.69987949244381));
#21735=CARTESIAN_POINT('Ctrl Pts',(-3.80097019086255,-2.26363775736839,
4.688765703387));
#21736=CARTESIAN_POINT('Ctrl Pts',(-3.59442944460758,-2.15719833661306,
4.6776519143302));
#21737=CARTESIAN_POINT('Ctrl Pts',(-3.3929874908777,-2.27299803191391,4.6665381252734));
#21738=CARTESIAN_POINT('Ctrl Pts',(-3.38102643442896,-2.50504406890429,
4.65542433621659));
#21739=CARTESIAN_POINT('Ctrl Pts',(-3.5694943658766,-2.64094207834572,4.64431054715979));
#21740=CARTESIAN_POINT('Ctrl Pts',(-3.78588445019465,-2.55630307100846,
4.63319675810299));
#21741=CARTESIAN_POINT('Ctrl Pts',(-3.83213238917682,-2.32859809017945,
4.62208296904618));
#21742=CARTESIAN_POINT('Ctrl Pts',(-3.66590691978443,-2.16624808716256,
4.61096917998938));
#21743=CARTESIAN_POINT('Ctrl Pts',(-3.4393560992794,-2.21785386089149,4.59985539093257));
#21744=CARTESIAN_POINT('Ctrl Pts',(-3.35984446292695,-2.43618006142673,
4.58874160187577));
#21745=CARTESIAN_POINT('Ctrl Pts',(-3.50014991321196,-2.62139024142312,
4.57762781281897));
#21746=CARTESIAN_POINT('Ctrl Pts',(-3.73184928030013,-2.60395942271916,
4.56651402376216));
#21747=CARTESIAN_POINT('Ctrl Pts',(-3.84286550587893,-2.3998422313225,4.55540023470536));
#21748=CARTESIAN_POINT('Ctrl Pts',(-3.73158417960078,-2.19586944742698,
4.54428644564855));
#21749=CARTESIAN_POINT('Ctrl Pts',(-3.49986236155564,-2.17873967321655,
4.53317265659175));
#21750=CARTESIAN_POINT('Ctrl Pts',(-3.35979765944108,-2.36413198553984,
4.52205886753494));
#21751=CARTESIAN_POINT('Ctrl Pts',(-3.43959288407154,-2.58235469793693,
4.51094507847814));
#21752=CARTESIAN_POINT('Ctrl Pts',(-3.66621056034765,-2.6336660879353,4.49983128942134));
#21753=CARTESIAN_POINT('Ctrl Pts',(-3.83222496126862,-2.47110025635944,
4.48871750036453));
#21754=CARTESIAN_POINT('Ctrl Pts',(-3.78568121870704,-2.24345555647604,
4.47760371130773));
#21755=CARTESIAN_POINT('Ctrl Pts',(-3.56918135654791,-2.15909775573836,
4.46648992225092));
#21756=CARTESIAN_POINT('Ctrl Pts',(-3.38089013692747,-2.29524052189659,
4.45537613319412));
#21757=CARTESIAN_POINT('Ctrl Pts',(-3.39315268252002,-2.52727080497827,
4.44426234413731));
#21758=CARTESIAN_POINT('Ctrl Pts',(-3.59474487821944,-2.64280871984201,
4.43314855508051));
#21759=CARTESIAN_POINT('Ctrl Pts',(-3.80114723737323,-2.53610097383652,
4.42203476602371));
#21760=CARTESIAN_POINT('Ctrl Pts',(-3.82343706699101,-2.30481863511631,
4.4109209769669));
#21761=CARTESIAN_POINT('Ctrl Pts',(-3.64121277969171,-2.16065653443092,
4.3998071879101));
#21762=CARTESIAN_POINT('Ctrl Pts',(-3.42126523797479,-2.23556891230323,
4.38869339885329));
#21763=CARTESIAN_POINT('Ctrl Pts',(-3.36491711226222,-2.46098554747977,
4.37757960979649));
#21764=CARTESIAN_POINT('Ctrl Pts',(-3.52374009350676,-2.63058418685777,
4.36646582073969));
#21765=CARTESIAN_POINT('Ctrl Pts',(-3.7523704915333,-2.58912096342209,4.35535203168288));
#21766=CARTESIAN_POINT('Ctrl Pts',(-3.84152271736619,-2.3745642740037,4.34423824262608));
#21767=CARTESIAN_POINT('Ctrl Pts',(-3.70962995644976,-2.18326697275372,
4.33312445356927));
#21768=CARTESIAN_POINT('Ctrl Pts',(-3.47734459894833,-2.19039236572141,
4.32201066451247));
#21769=CARTESIAN_POINT('Ctrl Pts',(-3.35742142491826,-2.38928487622609,
4.31089687545566));
#21770=CARTESIAN_POINT('Ctrl Pts',(-3.45934320255763,-2.59816388104693,
4.29978308639886));
#21771=CARTESIAN_POINT('Ctrl Pts',(-3.69040341475663,-2.62529829024268,
4.28866929734205));
#21772=CARTESIAN_POINT('Ctrl Pts',(-3.7885754343637,-2.50643134569448,4.28126010463752));
#21773=CARTESIAN_POINT('Ctrl Pts',(-3.80166758614466,-2.43937207542898,
4.27755550828525));
#21774=CARTESIAN_POINT('Ctrl Pts',(-3.64967348970877,-2.58599788000028,
5.20748149723825));
#21775=CARTESIAN_POINT('Ctrl Pts',(-3.71152220988337,-2.5694802628904,5.20377690088598));
#21776=CARTESIAN_POINT('Ctrl Pts',(-3.81636894835099,-2.47012721287082,
5.19636770818145));
#21777=CARTESIAN_POINT('Ctrl Pts',(-3.77625893469146,-2.25587333035667,
5.18525391912464));
#21778=CARTESIAN_POINT('Ctrl Pts',(-3.57450297395432,-2.17393137483105,
5.17414013006784));
#21779=CARTESIAN_POINT('Ctrl Pts',(-3.39623976035988,-2.29872360840445,
5.16302634101103));
#21780=CARTESIAN_POINT('Ctrl Pts',(-3.40440331076774,-2.5163091110919,5.15191255195424));
#21781=CARTESIAN_POINT('Ctrl Pts',(-3.59163731958239,-2.62738874138378,
5.14079876289742));
#21782=CARTESIAN_POINT('Ctrl Pts',(-3.78650651345082,-2.53036025862013,
5.12968497384062));
#21783=CARTESIAN_POINT('Ctrl Pts',(-3.81067380428838,-2.31399987678807,
5.11857118478382));
#21784=CARTESIAN_POINT('Ctrl Pts',(-3.64200416676191,-2.17636221393428,
5.10745739572701));
#21785=CARTESIAN_POINT('Ctrl Pts',(-3.43489003917469,-2.24341984097745,
5.09634360667021));
#21786=CARTESIAN_POINT('Ctrl Pts',(-3.37890173259108,-2.45379851750672,
5.08522981761341));
#21787=CARTESIAN_POINT('Ctrl Pts',(-3.52528777617272,-2.61493407462981,
5.07411602855659));
#21788=CARTESIAN_POINT('Ctrl Pts',(-3.74005846658983,-2.57933839839392,
5.0630022394998));
#21789=CARTESIAN_POINT('Ctrl Pts',(-3.82663220344909,-2.37959207115806,
5.05188845044299));
#21790=CARTESIAN_POINT('Ctrl Pts',(-3.7057668397564,-2.19852544308029,5.04077466138619));
#21791=CARTESIAN_POINT('Ctrl Pts',(-3.48809192538747,-2.20187071665909,
5.02966087232937));
#21792=CARTESIAN_POINT('Ctrl Pts',(-3.37284772224266,-2.38656599277582,
5.01854708327259));
#21793=CARTESIAN_POINT('Ctrl Pts',(-3.46551858429622,-2.58355755679196,
5.00743329421577));
#21794=CARTESIAN_POINT('Ctrl Pts',(-3.68128180662955,-2.61253681301776,
4.99631950515897));
#21795=CARTESIAN_POINT('Ctrl Pts',(-3.82264687187209,-2.44697871114761,
4.98520571610216));
#21796=CARTESIAN_POINT('Ctrl Pts',(-3.76022072914644,-2.23842046359223,
4.97409192704536));
#21797=CARTESIAN_POINT('Ctrl Pts',(-3.5511427365839,-2.17775779744681,4.96297813798855));
#21798=CARTESIAN_POINT('Ctrl Pts',(-3.38678435101677,-2.32051594004622,
4.95186434893176));
#21799=CARTESIAN_POINT('Ctrl Pts',(-3.41758466713793,-2.53602674395714,
4.94075055987494));
#21800=CARTESIAN_POINT('Ctrl Pts',(-3.6153518060864,-2.62703072656315,4.92963677081815));
#21801=CARTESIAN_POINT('Ctrl Pts',(-3.79906726285858,-2.51023091039877,
4.91852298176134));
#21802=CARTESIAN_POINT('Ctrl Pts',(-3.80057419634206,-2.29253549186461,
4.90740919270453));
#21803=CARTESIAN_POINT('Ctrl Pts',(-3.61849329325651,-2.17320355634632,
4.89629540364773));
#21804=CARTESIAN_POINT('Ctrl Pts',(-3.41948526912059,-2.26146097775627,
4.88518161459093));
#21805=CARTESIAN_POINT('Ctrl Pts',(-3.38570442533712,-2.47652473736257,
4.87406782553412));
#21806=CARTESIAN_POINT('Ctrl Pts',(-3.54807075131856,-2.62154453701271,
4.86295403647732));
#21807=CARTESIAN_POINT('Ctrl Pts',(-3.75796850753643,-2.56378210944851,
4.85184024742052));
#21808=CARTESIAN_POINT('Ctrl Pts',(-3.82327589732119,-2.35610805969097,
4.84072645836371));
#21809=CARTESIAN_POINT('Ctrl Pts',(-3.68421632616712,-2.18860880066658,
4.8296126693069));
#21810=CARTESIAN_POINT('Ctrl Pts',(-3.46807259659411,-2.2145983037314,4.81849888025011));
#21811=CARTESIAN_POINT('Ctrl Pts',(-3.37268351551706,-2.41028808198908,
4.80738509119329));
#21812=CARTESIAN_POINT('Ctrl Pts',(-3.48535979063151,-2.59656106212739,
4.79627130213649));
#21813=CARTESIAN_POINT('Ctrl Pts',(-3.70296754948933,-2.60291947294643,
4.78515751307969));
#21814=CARTESIAN_POINT('Ctrl Pts',(-3.82632794256814,-2.42354338891427,
4.77404372402288));
#21815=CARTESIAN_POINT('Ctrl Pts',(-3.74252780308088,-2.22261777400868,
4.76292993496608));
#21816=CARTESIAN_POINT('Ctrl Pts',(-3.52827034905847,-2.18405212220422,
4.75181614590928));
#21817=CARTESIAN_POINT('Ctrl Pts',(-3.37966785801241,-2.34314601196173,
4.74070235685247));
#21818=CARTESIAN_POINT('Ctrl Pts',(-3.43273787526403,-2.55427900173875,
4.72958856779567));
#21819=CARTESIAN_POINT('Ctrl Pts',(-3.63890481216799,-2.62419867158141,
4.71847477873886));
#21820=CARTESIAN_POINT('Ctrl Pts',(-3.80946173328402,-2.48890675473974,
4.70736098968206));
#21821=CARTESIAN_POINT('Ctrl Pts',(-3.78829595446756,-2.27223747701361,
4.69624720062526));
#21822=CARTESIAN_POINT('Ctrl Pts',(-3.59478075310558,-2.17251068550248,
4.68513341156845));
#21823=CARTESIAN_POINT('Ctrl Pts',(-3.40604278761636,-2.28100744345521,
4.67401962251164));
#21824=CARTESIAN_POINT('Ctrl Pts',(-3.39483605824625,-2.4984194378808,4.66290583345485));
#21825=CARTESIAN_POINT('Ctrl Pts',(-3.57141821148077,-2.62574700466167,
4.65179204439804));
#21826=CARTESIAN_POINT('Ctrl Pts',(-3.77416159988632,-2.54644577793071,
4.64067825534124));
#21827=CARTESIAN_POINT('Ctrl Pts',(-3.81749290078935,-2.33310106985138,
4.62956446628443));
#21828=CARTESIAN_POINT('Ctrl Pts',(-3.66175048306201,-2.18098971122316,
4.61845067722763));
#21829=CARTESIAN_POINT('Ctrl Pts',(-3.44948714789117,-2.22934095365678,
4.60733688817083));
#21830=CARTESIAN_POINT('Ctrl Pts',(-3.37498993318483,-2.43389835661598,
4.59622309911401));
#21831=CARTESIAN_POINT('Ctrl Pts',(-3.50644698442724,-2.60742820932623,
4.58510931005722));
#21832=CARTESIAN_POINT('Ctrl Pts',(-3.72353417177652,-2.59109666965397,
4.57399552100041));
#21833=CARTESIAN_POINT('Ctrl Pts',(-3.82754913074644,-2.39985218104442,
4.56288173194361));
#21834=CARTESIAN_POINT('Ctrl Pts',(-3.72328578972046,-2.20874299284009,
4.5517679428868));
#21835=CARTESIAN_POINT('Ctrl Pts',(-3.50617756728955,-2.19269351221351,
4.54065415383));
#21836=CARTESIAN_POINT('Ctrl Pts',(-3.37494608137275,-2.36639401102897,
4.52954036477319));
#21837=CARTESIAN_POINT('Ctrl Pts',(-3.44970899978995,-2.57085445235588,
4.51842657571639));
#21838=CARTESIAN_POINT('Ctrl Pts',(-3.66203497445559,-2.61892987644406,
4.50731278665958));
#21839=CARTESIAN_POINT('Ctrl Pts',(-3.81757963479854,-2.46661630054004,
4.49619899760278));
#21840=CARTESIAN_POINT('Ctrl Pts',(-3.77397118524436,-2.2533280717731,4.48508520854598));
#21841=CARTESIAN_POINT('Ctrl Pts',(-3.5711249421653,-2.17429031727573,4.47397141948917));
#21842=CARTESIAN_POINT('Ctrl Pts',(-3.39470835638149,-2.30184720512856,
4.46285763043237));
#21843=CARTESIAN_POINT('Ctrl Pts',(-3.40619756140558,-2.51924443916973,
4.45174384137556));
#21844=CARTESIAN_POINT('Ctrl Pts',(-3.59507629381618,-2.62749592593544,
4.44063005231876));
#21845=CARTESIAN_POINT('Ctrl Pts',(-3.78846183549484,-2.52751773117457,
4.42951626326196));
#21846=CARTESIAN_POINT('Ctrl Pts',(-3.80934595131713,-2.31082127219277,
4.41840247420515));
#21847=CARTESIAN_POINT('Ctrl Pts',(-3.63861368521871,-2.17575079119208,
4.40728868514835));
#21848=CARTESIAN_POINT('Ctrl Pts',(-3.43253719137339,-2.24593880082853,
4.39617489609154));
#21849=CARTESIAN_POINT('Ctrl Pts',(-3.37974267459471,-2.45713947835818,
4.38506110703474));
#21850=CARTESIAN_POINT('Ctrl Pts',(-3.52854944397912,-2.61604233624481,
4.37394731797793));
#21851=CARTESIAN_POINT('Ctrl Pts',(-3.74276120758414,-2.57719400158078,
4.36283352892113));
#21852=CARTESIAN_POINT('Ctrl Pts',(-3.82629102553408,-2.37616838455746,
4.35171973986432));
#21853=CARTESIAN_POINT('Ctrl Pts',(-3.70271611525743,-2.19693529644954,
4.34060595080753));
#21854=CARTESIAN_POINT('Ctrl Pts',(-3.48507989312992,-2.2036113246906,4.32949216175072));
#21855=CARTESIAN_POINT('Ctrl Pts',(-3.37271970468676,-2.38996062824249,
4.31837837269391));
#21856=CARTESIAN_POINT('Ctrl Pts',(-3.4682137593984,-2.58566662529692,4.30726458363711));
#21857=CARTESIAN_POINT('Ctrl Pts',(-3.68470210032476,-2.61108979604925,
4.2961507945803));
#21858=CARTESIAN_POINT('Ctrl Pts',(-3.77668287645173,-2.49971922570604,
4.28874160187577));
#21859=CARTESIAN_POINT('Ctrl Pts',(-3.78894936833816,-2.43688906544025,
4.2850370055235));
#21860=CARTESIAN_POINT('Ctrl Pts',(-3.64632995769868,-2.57347832743338,
5.2149629944765));
#21861=CARTESIAN_POINT('Ctrl Pts',(-3.70401562879218,-2.55807251426281,
5.21125839812423));
#21862=CARTESIAN_POINT('Ctrl Pts',(-3.80180511341523,-2.46540693687679,
5.20384920541969));
#21863=CARTESIAN_POINT('Ctrl Pts',(-3.76439491237975,-2.26557452381591,
5.19273541636289));
#21864=CARTESIAN_POINT('Ctrl Pts',(-3.57621918361154,-2.18914809685241,
5.18162162730608));
#21865=CARTESIAN_POINT('Ctrl Pts',(-3.40995490072177,-2.30554054152415,
5.17050783824929));
#21866=CARTESIAN_POINT('Ctrl Pts',(-3.41756896100391,-2.5084803227728,5.15939404919247));
#21867=CARTESIAN_POINT('Ctrl Pts',(-3.59220021318681,-2.6120831620897,5.14828026013568));
#21868=CARTESIAN_POINT('Ctrl Pts',(-3.77395272466994,-2.52158568489689,
5.13716647107886));
#21869=CARTESIAN_POINT('Ctrl Pts',(-3.79649331057924,-2.31978856138657,
5.12605268202207));
#21870=CARTESIAN_POINT('Ctrl Pts',(-3.63917685833343,-2.19141531571474,
5.11493889296526));
#21871=CARTESIAN_POINT('Ctrl Pts',(-3.44600362194169,-2.25395928116791,
5.10382510390846));
#21872=CARTESIAN_POINT('Ctrl Pts',(-3.39378389888927,-2.45017732909347,
5.09271131485166));
#21873=CARTESIAN_POINT('Ctrl Pts',(-3.53031667012352,-2.60046682131627,
5.08159752579484));
#21874=CARTESIAN_POINT('Ctrl Pts',(-3.73063110464943,-2.56726709679655,
5.07048373673805));
#21875=CARTESIAN_POINT('Ctrl Pts',(-3.81137754686683,-2.38096573271764,
5.05936994768124));
#21876=CARTESIAN_POINT('Ctrl Pts',(-3.69864765371964,-2.21208673370492,
5.04825615862444));
#21877=CARTESIAN_POINT('Ctrl Pts',(-3.49562447910673,-2.21520683628489,
5.03714236956762));
#21878=CARTESIAN_POINT('Ctrl Pts',(-3.38813738512521,-2.38747023834909,
5.02602858051084));
#21879=CARTESIAN_POINT('Ctrl Pts',(-3.47457055388411,-2.57120226284288,
5.01491479145402));
#21880=CARTESIAN_POINT('Ctrl Pts',(-3.67581071281477,-2.59823091983783,
5.00380100239722));
#21881=CARTESIAN_POINT('Ctrl Pts',(-3.80766046871388,-2.44381656519338,
4.99268721334042));
#21882=CARTESIAN_POINT('Ctrl Pts',(-3.74943624149071,-2.24929641282234,
4.9815734242836));
#21883=CARTESIAN_POINT('Ctrl Pts',(-3.55443132824748,-2.19271696223645,
4.97045963522681));
#21884=CARTESIAN_POINT('Ctrl Pts',(-3.40113593677424,-2.32586602719142,
4.95934584617));
#21885=CARTESIAN_POINT('Ctrl Pts',(-3.42986307777772,-2.52687075803154,
4.94823205711319));
#21886=CARTESIAN_POINT('Ctrl Pts',(-3.61431847310812,-2.61174924531453,
4.9371182680564));
#21887=CARTESIAN_POINT('Ctrl Pts',(-3.78566800765362,-2.50281124692072,
4.92600447899958));
#21888=CARTESIAN_POINT('Ctrl Pts',(-3.78707350915862,-2.29976894828182,
4.91489068994279));
#21889=CARTESIAN_POINT('Ctrl Pts',(-3.6172485061812,-2.18846926796789,4.90377690088598));
#21890=CARTESIAN_POINT('Ctrl Pts',(-3.43163574988059,-2.27078606560966,
4.89266311182917));
#21891=CARTESIAN_POINT('Ctrl Pts',(-3.40012870109683,-2.47137384278207,
4.88154932277237));
#21892=CARTESIAN_POINT('Ctrl Pts',(-3.55156611889279,-2.60663233222288,
4.87043553371556));
#21893=CARTESIAN_POINT('Ctrl Pts',(-3.74733561734428,-2.55275790460943,
4.85932174465877));
#21894=CARTESIAN_POINT('Ctrl Pts',(-3.80824715434074,-2.35906243451482,
4.84820795560196));
#21895=CARTESIAN_POINT('Ctrl Pts',(-3.6785477092859,-2.2028375823722,4.83709416654515));
#21896=CARTESIAN_POINT('Ctrl Pts',(-3.47695265513,-2.22707772705829,4.82598037748836));
#21897=CARTESIAN_POINT('Ctrl Pts',(-3.38798423118545,-2.40959558923983,
4.81486658843155));
#21898=CARTESIAN_POINT('Ctrl Pts',(-3.49307624485919,-2.5833304997688,4.80375279937474));
#21899=CARTESIAN_POINT('Ctrl Pts',(-3.69603678421119,-2.5892609247501,4.79263901031794));
#21900=CARTESIAN_POINT('Ctrl Pts',(-3.81109376584347,-2.42195867894277,
4.78152522126113));
#21901=CARTESIAN_POINT('Ctrl Pts',(-3.7329342296331,-2.23455740527076,4.77041143220433));
#21902=CARTESIAN_POINT('Ctrl Pts',(-3.53309848546286,-2.19858761480107,
4.75929764314753));
#21903=CARTESIAN_POINT('Ctrl Pts',(-3.39449845626323,-2.34697286467576,
4.74818385409072));
#21904=CARTESIAN_POINT('Ctrl Pts',(-3.4439963205919,-2.54389445288135,4.73707006503392));
#21905=CARTESIAN_POINT('Ctrl Pts',(-3.63628612188485,-2.60910781649055,
4.72595627597711));
#21906=CARTESIAN_POINT('Ctrl Pts',(-3.79536282430398,-2.48292242422203,
4.71484248692031));
#21907=CARTESIAN_POINT('Ctrl Pts',(-3.77562171807257,-2.28083719665882,
4.7037286978635));
#21908=CARTESIAN_POINT('Ctrl Pts',(-3.59513206160358,-2.18782303439192,
4.6926149088067));
#21909=CARTESIAN_POINT('Ctrl Pts',(-3.41909808435503,-2.28901685499652,
4.6815011197499));
#21910=CARTESIAN_POINT('Ctrl Pts',(-3.40864568206353,-2.49179480685731,
4.67038733069309));
#21911=CARTESIAN_POINT('Ctrl Pts',(-3.57334205708494,-2.61055193097763,
4.65927354163629));
#21912=CARTESIAN_POINT('Ctrl Pts',(-3.76243874957797,-2.53658848485295,
4.64815975257949));
#21913=CARTESIAN_POINT('Ctrl Pts',(-3.80285341240188,-2.33760404952332,
4.63704596352268));
#21914=CARTESIAN_POINT('Ctrl Pts',(-3.65759404633958,-2.19573133528376,
4.62593217446587));
#21915=CARTESIAN_POINT('Ctrl Pts',(-3.45961819650295,-2.24082804642207,
4.61481838540908));
#21916=CARTESIAN_POINT('Ctrl Pts',(-3.39013540344272,-2.43161665180523,
4.60370459635226));
#21917=CARTESIAN_POINT('Ctrl Pts',(-3.51274405564254,-2.59346617722935,
4.59259080729546));
#21918=CARTESIAN_POINT('Ctrl Pts',(-3.71521906325291,-2.57823391658879,
4.58147701823866));
#21919=CARTESIAN_POINT('Ctrl Pts',(-3.81223275561396,-2.39986213076634,
4.57036322918186));
#21920=CARTESIAN_POINT('Ctrl Pts',(-3.71498739984013,-2.2216165382532,4.55924944012505));
#21921=CARTESIAN_POINT('Ctrl Pts',(-3.51249277302345,-2.20664735121048,
4.54813565106825));
#21922=CARTESIAN_POINT('Ctrl Pts',(-3.39009450330442,-2.36865603651811,
4.53702186201144));
#21923=CARTESIAN_POINT('Ctrl Pts',(-3.45982511550835,-2.55935420677483,
4.52590807295464));
#21924=CARTESIAN_POINT('Ctrl Pts',(-3.65785938856352,-2.60419366495283,
4.51479428389783));
#21925=CARTESIAN_POINT('Ctrl Pts',(-3.80293430832847,-2.46213234472064,
4.50368049484103));
#21926=CARTESIAN_POINT('Ctrl Pts',(-3.76226115178167,-2.26320058707017,
4.49256670578422));
#21927=CARTESIAN_POINT('Ctrl Pts',(-3.57306852778269,-2.1894828788131,4.48145291672742));
#21928=CARTESIAN_POINT('Ctrl Pts',(-3.40852657583551,-2.30845388836054,
4.47033912767062));
#21929=CARTESIAN_POINT('Ctrl Pts',(-3.41924244029115,-2.51121807336119,
4.45922533861381));
#21930=CARTESIAN_POINT('Ctrl Pts',(-3.59540770941291,-2.61218313202887,
4.44811154955701));
#21931=CARTESIAN_POINT('Ctrl Pts',(-3.77577643361645,-2.51893448851262,
4.4369977605002));
#21932=CARTESIAN_POINT('Ctrl Pts',(-3.79525483564324,-2.31682390926922,
4.42588397144341));
#21933=CARTESIAN_POINT('Ctrl Pts',(-3.63601459074572,-2.19084504795324,
4.41477018238659));
#21934=CARTESIAN_POINT('Ctrl Pts',(-3.44380914477199,-2.25630868935384,
4.4036563933298));
#21935=CARTESIAN_POINT('Ctrl Pts',(-3.3945682369272,-2.45329340923659,4.39254260427298));
#21936=CARTESIAN_POINT('Ctrl Pts',(-3.53335879445148,-2.60150048563184,
4.38142881521619));
#21937=CARTESIAN_POINT('Ctrl Pts',(-3.73315192363498,-2.56526703973946,
4.37031502615937));
#21938=CARTESIAN_POINT('Ctrl Pts',(-3.81105933370197,-2.37777249511123,
4.35920123710258));
#21939=CARTESIAN_POINT('Ctrl Pts',(-3.69580227406509,-2.21060362014537,
4.34808744804577));
#21940=CARTESIAN_POINT('Ctrl Pts',(-3.49281518731151,-2.21683028365978,
4.33697365898897));
#21941=CARTESIAN_POINT('Ctrl Pts',(-3.38801798445527,-2.3906363802589,4.32585986993216));
#21942=CARTESIAN_POINT('Ctrl Pts',(-3.47708431623917,-2.57316936954691,
4.31474608087536));
#21943=CARTESIAN_POINT('Ctrl Pts',(-3.6790007858929,-2.59688130185582,4.30363229181855));
#21944=CARTESIAN_POINT('Ctrl Pts',(-3.76479031853975,-2.4930071057176,4.29622309911402));
#21945=CARTESIAN_POINT('Ctrl Pts',(-3.77623115053166,-2.43440605545153,
4.29251850276175));
#21946=CARTESIAN_POINT('Ctrl Pts',(-3.64298642568859,-2.56095877486649,
5.22244449171475));
#21947=CARTESIAN_POINT('Ctrl Pts',(-3.69650904770099,-2.54666476563522,
5.21873989536248));
#21948=CARTESIAN_POINT('Ctrl Pts',(-3.78724127847948,-2.46068666088276,
5.21133070265795));
#21949=CARTESIAN_POINT('Ctrl Pts',(-3.75253089006804,-2.27527571727515,
5.20021691360113));
#21950=CARTESIAN_POINT('Ctrl Pts',(-3.57793539326875,-2.20436481887379,
5.18910312454434));
#21951=CARTESIAN_POINT('Ctrl Pts',(-3.42367004108366,-2.31235747464383,
5.17798933548752));
#21952=CARTESIAN_POINT('Ctrl Pts',(-3.43073461124009,-2.5006515344537,5.16687554643073));
#21953=CARTESIAN_POINT('Ctrl Pts',(-3.59276310679123,-2.59677758279563,
5.15576175737392));
#21954=CARTESIAN_POINT('Ctrl Pts',(-3.76139893588905,-2.51281111117365,
5.14464796831712));
#21955=CARTESIAN_POINT('Ctrl Pts',(-3.78231281687012,-2.32557724598507,
5.13353417926031));
#21956=CARTESIAN_POINT('Ctrl Pts',(-3.63634954990495,-2.2064684174952,5.12242039020351));
#21957=CARTESIAN_POINT('Ctrl Pts',(-3.4571172047087,-2.26449872135838,5.1113066011467));
#21958=CARTESIAN_POINT('Ctrl Pts',(-3.40866606518746,-2.44655614068022,
5.10019281208991));
#21959=CARTESIAN_POINT('Ctrl Pts',(-3.53534556407432,-2.58599956800273,
5.08907902303309));
#21960=CARTESIAN_POINT('Ctrl Pts',(-3.72120374270903,-2.55519579519918,
5.0779652339763));
#21961=CARTESIAN_POINT('Ctrl Pts',(-3.79612289028458,-2.3823393942772,5.06685144491949));
#21962=CARTESIAN_POINT('Ctrl Pts',(-3.69152846768288,-2.22564802432955,
5.05573765586268));
#21963=CARTESIAN_POINT('Ctrl Pts',(-3.503157032826,-2.22854295591068,5.04462386680587));
#21964=CARTESIAN_POINT('Ctrl Pts',(-3.40342704800776,-2.38837448392236,
5.03351007774909));
#21965=CARTESIAN_POINT('Ctrl Pts',(-3.483622523472,-2.55884696889381,5.02239628869226));
#21966=CARTESIAN_POINT('Ctrl Pts',(-3.670339619,-2.58392502665791,5.01128249963547));
#21967=CARTESIAN_POINT('Ctrl Pts',(-3.79267406555566,-2.44065441923915,
5.00016871057867));
#21968=CARTESIAN_POINT('Ctrl Pts',(-3.73865175383498,-2.26017236205245,
4.98905492152186));
#21969=CARTESIAN_POINT('Ctrl Pts',(-3.55771991991106,-2.20767612702608,
4.97794113246506));
#21970=CARTESIAN_POINT('Ctrl Pts',(-3.4154875225317,-2.3312161143366,4.96682734340825));
#21971=CARTESIAN_POINT('Ctrl Pts',(-3.44214148841752,-2.51771477210593,
4.95571355435145));
#21972=CARTESIAN_POINT('Ctrl Pts',(-3.61328514012983,-2.59646776406591,
4.94459976529465));
#21973=CARTESIAN_POINT('Ctrl Pts',(-3.77226875244865,-2.49539158344266,
4.93348597623784));
#21974=CARTESIAN_POINT('Ctrl Pts',(-3.77357282197517,-2.30700240469905,
4.92237218718103));
#21975=CARTESIAN_POINT('Ctrl Pts',(-3.61600371910589,-2.20373497958946,
4.91125839812423));
#21976=CARTESIAN_POINT('Ctrl Pts',(-3.44378623064059,-2.28011115346305,
4.90014460906743));
#21977=CARTESIAN_POINT('Ctrl Pts',(-3.41455297685654,-2.46622294820157,
4.88903082001062));
#21978=CARTESIAN_POINT('Ctrl Pts',(-3.555061486467,-2.59172012743304,4.87791703095382));
#21979=CARTESIAN_POINT('Ctrl Pts',(-3.73670272715212,-2.54173369977035,
4.86680324189701));
#21980=CARTESIAN_POINT('Ctrl Pts',(-3.79321841136028,-2.36201680933867,
4.85568945284021));
#21981=CARTESIAN_POINT('Ctrl Pts',(-3.67287909240468,-2.21706636407783,
4.8445756637834));
#21982=CARTESIAN_POINT('Ctrl Pts',(-3.48583271366589,-2.23955715038517,
4.83346187472661));
#21983=CARTESIAN_POINT('Ctrl Pts',(-3.40328494685383,-2.40890309649059,
4.82234808566979));
#21984=CARTESIAN_POINT('Ctrl Pts',(-3.50079269908688,-2.57009993741021,
4.811234296613));
#21985=CARTESIAN_POINT('Ctrl Pts',(-3.68910601893303,-2.57560237655376,
4.80012050755619));
#21986=CARTESIAN_POINT('Ctrl Pts',(-3.79585958911879,-2.42037396897126,
4.78900671849938));
#21987=CARTESIAN_POINT('Ctrl Pts',(-3.72334065618531,-2.24649703653284,
4.77789292944258));
#21988=CARTESIAN_POINT('Ctrl Pts',(-3.53792662186724,-2.21312310739792,
4.76677914038578));
#21989=CARTESIAN_POINT('Ctrl Pts',(-3.40932905451407,-2.35079971738979,
4.75566535132897));
#21990=CARTESIAN_POINT('Ctrl Pts',(-3.45525476591977,-2.53350990402394,
4.74455156227217));
#21991=CARTESIAN_POINT('Ctrl Pts',(-3.6336674316017,-2.59401696139969,4.73343777321536));
#21992=CARTESIAN_POINT('Ctrl Pts',(-3.78126391532395,-2.47693809370431,
4.72232398415856));
#21993=CARTESIAN_POINT('Ctrl Pts',(-3.76294748167758,-2.28943691630404,
4.71121019510175));
#21994=CARTESIAN_POINT('Ctrl Pts',(-3.59548337010158,-2.20313538328135,
4.70009640604495));
#21995=CARTESIAN_POINT('Ctrl Pts',(-3.43215338109369,-2.29702626653782,
4.68898261698815));
#21996=CARTESIAN_POINT('Ctrl Pts',(-3.42245530588083,-2.48517017583382,
4.67786882793134));
#21997=CARTESIAN_POINT('Ctrl Pts',(-3.5752659026891,-2.59535685729358,4.66675503887453));
#21998=CARTESIAN_POINT('Ctrl Pts',(-3.75071589926964,-2.5267311917752,4.65564124981774));
#21999=CARTESIAN_POINT('Ctrl Pts',(-3.7882139240144,-2.34210702919526,4.64452746076093));
#22000=CARTESIAN_POINT('Ctrl Pts',(-3.65343760961716,-2.21047295934436,
4.63341367170412));
#22001=CARTESIAN_POINT('Ctrl Pts',(-3.46974924511472,-2.25231513918736,
4.62229988264733));
#22002=CARTESIAN_POINT('Ctrl Pts',(-3.4052808737006,-2.42933494699449,4.61118609359051));
#22003=CARTESIAN_POINT('Ctrl Pts',(-3.51904112685782,-2.57950414513246,
4.60007230453372));
#22004=CARTESIAN_POINT('Ctrl Pts',(-3.7069039547293,-2.5653711635236,4.5889585154769));
#22005=CARTESIAN_POINT('Ctrl Pts',(-3.79691638048147,-2.39987208048827,
4.57784472642011));
#22006=CARTESIAN_POINT('Ctrl Pts',(-3.7066890099598,-2.23449008366631,4.5667309373633));
#22007=CARTESIAN_POINT('Ctrl Pts',(-3.51880797875736,-2.22060119020745,
4.5556171483065));
#22008=CARTESIAN_POINT('Ctrl Pts',(-3.40524292523608,-2.37091806200724,
4.54450335924969));
#22009=CARTESIAN_POINT('Ctrl Pts',(-3.46994123122676,-2.54785396119378,
4.53338957019289));
#22010=CARTESIAN_POINT('Ctrl Pts',(-3.65368380267146,-2.5894574534616,4.52227578113609));
#22011=CARTESIAN_POINT('Ctrl Pts',(-3.78828898185839,-2.45764838890124,
4.51116199207927));
#22012=CARTESIAN_POINT('Ctrl Pts',(-3.75055111831899,-2.27307310236724,
4.50004820302248));
#22013=CARTESIAN_POINT('Ctrl Pts',(-3.57501211340008,-2.20467544035046,
4.48893441396567));
#22014=CARTESIAN_POINT('Ctrl Pts',(-3.42234479528953,-2.31506057159251,
4.47782062490887));
#22015=CARTESIAN_POINT('Ctrl Pts',(-3.43228731917671,-2.50319170755265,
4.46670683585206));
#22016=CARTESIAN_POINT('Ctrl Pts',(-3.59573912500965,-2.5968703381223,4.45559304679526));
#22017=CARTESIAN_POINT('Ctrl Pts',(-3.76309103173807,-2.51035124585066,
4.44447925773846));
#22018=CARTESIAN_POINT('Ctrl Pts',(-3.78116371996935,-2.32282654634568,
4.43336546868165));
#22019=CARTESIAN_POINT('Ctrl Pts',(-3.63341549627273,-2.20593930471439,
4.42225167962485));
#22020=CARTESIAN_POINT('Ctrl Pts',(-3.45508109817058,-2.26667857787915,
4.41113789056804));
#22021=CARTESIAN_POINT('Ctrl Pts',(-3.40939379925969,-2.449447340115,4.40002410151124));
#22022=CARTESIAN_POINT('Ctrl Pts',(-3.53816814492384,-2.58695863501888,
4.38891031245443));
#22023=CARTESIAN_POINT('Ctrl Pts',(-3.72354263968583,-2.55334007789814,
4.37779652339763));
#22024=CARTESIAN_POINT('Ctrl Pts',(-3.79582764186986,-2.379376605665,4.36668273434082));
#22025=CARTESIAN_POINT('Ctrl Pts',(-3.68888843287276,-2.22427194384119,
4.35556894528402));
#22026=CARTESIAN_POINT('Ctrl Pts',(-3.50055048149309,-2.23004924262897,
4.34445515622722));
#22027=CARTESIAN_POINT('Ctrl Pts',(-3.40331626422378,-2.3913121322753,4.33334136717041));
#22028=CARTESIAN_POINT('Ctrl Pts',(-3.48595487307994,-2.5606721137969,4.32222757811361));
#22029=CARTESIAN_POINT('Ctrl Pts',(-3.67329947146103,-2.58267280766239,
4.3111137890568));
#22030=CARTESIAN_POINT('Ctrl Pts',(-3.75289776062778,-2.48629498572916,
4.30370459635227));
#22031=CARTESIAN_POINT('Ctrl Pts',(-3.76351293272515,-2.4319230454628,4.3));
#22032=CARTESIAN_POINT('Ctrl Pts',(-3.76638442554721,-2.39990578503699,
5.13785196366098));
#22033=CARTESIAN_POINT('Ctrl Pts',(-3.76649613683224,-2.3783172805639,5.13641270219409));
#22034=CARTESIAN_POINT('Ctrl Pts',(-3.76259705167907,-2.35676746354197,
5.1349734407272));
#22035=CARTESIAN_POINT('Ctrl Pts',(-3.75449995887908,-2.33693141876819,
5.13353417926032));
#22036=CARTESIAN_POINT('Ctrl Pts',(-3.73365839454839,-2.28587430315511,
5.12982958290805));
#22037=CARTESIAN_POINT('Ctrl Pts',(-3.68500397222667,-2.24617136032516,
5.12612498655578));
#22038=CARTESIAN_POINT('Ctrl Pts',(-3.6308047035331,-2.23599160622071,5.12242039020351));
#22039=CARTESIAN_POINT('Ctrl Pts',(-3.57660543483953,-2.22581185211626,
5.11871579385124));
#22040=CARTESIAN_POINT('Ctrl Pts',(-3.51686131977411,-2.24515528673732,
5.11501119749897));
#22041=CARTESIAN_POINT('Ctrl Pts',(-3.4789140723212,-2.28516990726816,5.1113066011467));
#22042=CARTESIAN_POINT('Ctrl Pts',(-3.44096682486829,-2.32518452779899,
5.10760200479444));
#22043=CARTESIAN_POINT('Ctrl Pts',(-3.42481644502788,-2.3858703342396,5.10389740844217));
#22044=CARTESIAN_POINT('Ctrl Pts',(-3.43785450492215,-2.43945380868033,
5.1001928120899));
#22045=CARTESIAN_POINT('Ctrl Pts',(-3.45089256481642,-2.49303728312105,
5.09648821573763));
#22046=CARTESIAN_POINT('Ctrl Pts',(-3.49311906444537,-2.53951842556189,
5.09278361938536));
#22047=CARTESIAN_POINT('Ctrl Pts',(-3.54520867736563,-2.55762503464839,
5.08907902303309));
#22048=CARTESIAN_POINT('Ctrl Pts',(-3.59729829028589,-2.57573164373488,
5.08537442668083));
#22049=CARTESIAN_POINT('Ctrl Pts',(-3.65925101649746,-2.56546371946703,
5.08166983032856));
#22050=CARTESIAN_POINT('Ctrl Pts',(-3.70271390419917,-2.53152035717944,
5.07796523397629));
#22051=CARTESIAN_POINT('Ctrl Pts',(-3.74226404589835,-2.50063274572034,
5.07459414387119));
#22052=CARTESIAN_POINT('Ctrl Pts',(-3.76650359324528,-2.4501405807959,5.07122305376609));
#22053=CARTESIAN_POINT('Ctrl Pts',(-3.7668206250807,-2.39991359866148,5.06785196366098));
#22054=CARTESIAN_POINT('Ctrl Pts',(-3.65301702171886,-2.59851743256717,
5.2));
#22055=CARTESIAN_POINT('Ctrl Pts',(-3.66542047324148,-2.59392489431986,
5.2));
#22056=CARTESIAN_POINT('Ctrl Pts',(-3.67726976851323,-2.58806562778896,
5.2));
#22057=CARTESIAN_POINT('Ctrl Pts',(-3.6884471572875,-2.58110287343,5.2));
#22058=CARTESIAN_POINT('Ctrl Pts',(-3.69411332072466,-2.57757323829184,
5.2));
#22059=CARTESIAN_POINT('Ctrl Pts',(-3.69960638117381,-2.57375928297626,
5.2));
#22060=CARTESIAN_POINT('Ctrl Pts',(-3.70490756348411,-2.56967869660782,
5.2));
#22061=CARTESIAN_POINT('Ctrl Pts',(-3.7094943667238,-2.56614800370216,5.2));
#22062=CARTESIAN_POINT('Ctrl Pts',(-3.71393749668481,-2.56241764644412,
5.2));
#22063=CARTESIAN_POINT('Ctrl Pts',(-3.71822298464189,-2.55849819748795,
5.2));
#22064=CARTESIAN_POINT('Ctrl Pts',(-3.7213335990699,-2.55565327187038,5.2));
#22065=CARTESIAN_POINT('Ctrl Pts',(-3.72435497328541,-2.55271413748664,
5.2));
#22066=CARTESIAN_POINT('Ctrl Pts',(-3.72727770073803,-2.54969101779411,
5.2));
#22067=CARTESIAN_POINT('Ctrl Pts',(-3.73622270492435,-2.54043876326685,
5.2));
#22068=CARTESIAN_POINT('Ctrl Pts',(-3.7442634301432,-2.53038665580988,5.2));
#22069=CARTESIAN_POINT('Ctrl Pts',(-3.75126083636282,-2.51966573521934,
5.2));
#22070=CARTESIAN_POINT('Ctrl Pts',(-3.75579169616378,-2.51272387896453,
5.2));
#22071=CARTESIAN_POINT('Ctrl Pts',(-3.75988429343086,-2.5055010355982,5.2));
#22072=CARTESIAN_POINT('Ctrl Pts',(-3.76348914806144,-2.49803012759629,
5.2));
#22073=CARTESIAN_POINT('Ctrl Pts',(-3.76515593070928,-2.49457579140323,
5.2));
#22074=CARTESIAN_POINT('Ctrl Pts',(-3.76671430859645,-2.49107651026494,
5.2));
#22075=CARTESIAN_POINT('Ctrl Pts',(-3.76815914917795,-2.48753923965477,
5.2));
#22076=CARTESIAN_POINT('Ctrl Pts',(-3.77216127817835,-2.47774119447769,
5.2));
#22077=CARTESIAN_POINT('Ctrl Pts',(-3.77529843764987,-2.46764366345261,
5.2));
#22078=CARTESIAN_POINT('Ctrl Pts',(-3.77747651250232,-2.45732003292749,
5.2));
#22079=CARTESIAN_POINT('Ctrl Pts',(-3.779330303747,-2.44853344055707,5.2));
#22080=CARTESIAN_POINT('Ctrl Pts',(-3.78048859875581,-2.43958258054595,
5.2));
#22081=CARTESIAN_POINT('Ctrl Pts',(-3.78096402676373,-2.43054575199388,
5.2));
#22082=CARTESIAN_POINT('Ctrl Pts',(-3.78113316899519,-2.42733073453364,
5.2));
#22083=CARTESIAN_POINT('Ctrl Pts',(-3.78121551844131,-2.4241062749112,5.2));
#22084=CARTESIAN_POINT('Ctrl Pts',(-3.78121200526832,-2.42088560814198,
5.2));
#22085=CARTESIAN_POINT('Ctrl Pts',(-3.78119923320481,-2.40917694458053,
5.2));
#22086=CARTESIAN_POINT('Ctrl Pts',(-3.78005717128054,-2.39748206272171,
5.2));
#22087=CARTESIAN_POINT('Ctrl Pts',(-3.77783120534438,-2.38597327518306,
5.2));
#22088=CARTESIAN_POINT('Ctrl Pts',(-3.77668820057652,-2.38006366137664,
5.2));
#22089=CARTESIAN_POINT('Ctrl Pts',(-3.77525871074905,-2.37420329819383,
5.2));
#22090=CARTESIAN_POINT('Ctrl Pts',(-3.77354495279965,-2.36841778018193,
5.2));
#22091=CARTESIAN_POINT('Ctrl Pts',(-3.771857709037,-2.36272177207139,5.2));
#22092=CARTESIAN_POINT('Ctrl Pts',(-3.76989216970551,-2.35709287385817,
5.2));
#22093=CARTESIAN_POINT('Ctrl Pts',(-3.76766230775392,-2.35158840548752,
5.2));
#22094=CARTESIAN_POINT('Ctrl Pts',(-3.76420558159522,-2.34305539303218,
5.2));
#22095=CARTESIAN_POINT('Ctrl Pts',(-3.76011199819993,-2.33480777321703,
5.2));
#22096=CARTESIAN_POINT('Ctrl Pts',(-3.75539090007917,-2.32694141045687,
5.2));
#22097=CARTESIAN_POINT('Ctrl Pts',(-3.75297689160326,-2.32291915421652,
5.2));
#22098=CARTESIAN_POINT('Ctrl Pts',(-3.75039789394566,-2.31899648610286,
5.2));
#22099=CARTESIAN_POINT('Ctrl Pts',(-3.74766394659108,-2.31519991459367,
5.2));
#22100=CARTESIAN_POINT('Ctrl Pts',(-3.7422293448357,-2.30765300475514,5.2));
#22101=CARTESIAN_POINT('Ctrl Pts',(-3.73617584795258,-2.30058959872182,
5.2));
#22102=CARTESIAN_POINT('Ctrl Pts',(-3.7295081063639,-2.29412082362908,5.2));
#22103=CARTESIAN_POINT('Ctrl Pts',(-3.72872963705521,-2.29336558397147,
5.2));
#22104=CARTESIAN_POINT('Ctrl Pts',(-3.72794278071792,-2.29261847520289,
5.2));
#22105=CARTESIAN_POINT('Ctrl Pts',(-3.72714769448934,-2.29187956305505,
5.2));
#22106=CARTESIAN_POINT('Origin',(-3.6,-2.4,4.7));
#22107=CARTESIAN_POINT('Origin',(3.6,-2.4,4.2));
#22108=CARTESIAN_POINT('Origin',(-3.6,-2.4,4.2));
#22109=CARTESIAN_POINT('Origin',(-3.6,2.4,4.2));
#22110=CARTESIAN_POINT('Origin',(3.6,2.4,4.2));
#22111=CARTESIAN_POINT('Origin',(-4.6,0.,0.3));
#22112=CARTESIAN_POINT('',(-4.9,3.67394039744206E-17,0.6));
#22113=CARTESIAN_POINT('Origin',(-4.6,0.,0.6));
#22114=CARTESIAN_POINT('',(-4.9,3.67394039744206E-17,0.));
#22115=CARTESIAN_POINT('',(-4.9,3.67394039744206E-17,0.3));
#22116=CARTESIAN_POINT('Origin',(-4.6,0.,0.));
#22117=CARTESIAN_POINT('Origin',(4.6,0.,0.3));
#22118=CARTESIAN_POINT('',(4.3,3.67394039744206E-17,0.6));
#22119=CARTESIAN_POINT('Origin',(4.6,0.,0.6));
#22120=CARTESIAN_POINT('',(4.3,3.67394039744206E-17,0.));
#22121=CARTESIAN_POINT('',(4.3,3.67394039744206E-17,0.3));
#22122=CARTESIAN_POINT('Origin',(4.6,0.,0.));
#22123=CARTESIAN_POINT('Origin',(5.2,1.,0.));
#22124=CARTESIAN_POINT('',(5.2,1.,0.));
#22125=CARTESIAN_POINT('',(4.,1.,0.));
#22126=CARTESIAN_POINT('',(5.2,1.,0.));
#22127=CARTESIAN_POINT('',(4.,1.,0.6));
#22128=CARTESIAN_POINT('',(4.,1.,0.));
#22129=CARTESIAN_POINT('',(5.2,1.,0.6));
#22130=CARTESIAN_POINT('',(5.2,1.,0.6));
#22131=CARTESIAN_POINT('',(5.2,1.,0.));
#22132=CARTESIAN_POINT('Origin',(5.2,-1.,0.));
#22133=CARTESIAN_POINT('',(5.2,-1.,0.));
#22134=CARTESIAN_POINT('',(5.2,-1.,0.));
#22135=CARTESIAN_POINT('',(5.2,-1.,0.6));
#22136=CARTESIAN_POINT('',(5.2,-1.,0.6));
#22137=CARTESIAN_POINT('',(5.2,-1.,0.));
#22138=CARTESIAN_POINT('Origin',(4.,-1.,0.));
#22139=CARTESIAN_POINT('',(4.,-1.,0.));
#22140=CARTESIAN_POINT('',(4.,-1.,0.));
#22141=CARTESIAN_POINT('',(4.,-1.,0.6));
#22142=CARTESIAN_POINT('',(4.,-1.,0.6));
#22143=CARTESIAN_POINT('',(4.,-1.,0.));
#22144=CARTESIAN_POINT('Origin',(4.6,0.,0.6));
#22145=CARTESIAN_POINT('',(4.,-1.4,0.6));
#22146=CARTESIAN_POINT('Origin',(-4.,1.,0.));
#22147=CARTESIAN_POINT('',(-4.,1.,0.));
#22148=CARTESIAN_POINT('',(-5.2,1.,0.));
#22149=CARTESIAN_POINT('',(-4.,1.,0.));
#22150=CARTESIAN_POINT('',(-5.2,1.,0.6));
#22151=CARTESIAN_POINT('',(-5.2,1.,0.));
#22152=CARTESIAN_POINT('',(-4.,1.,0.6));
#22153=CARTESIAN_POINT('',(-4.,1.,0.6));
#22154=CARTESIAN_POINT('',(-4.,1.,0.));
#22155=CARTESIAN_POINT('Origin',(-5.2,-1.,0.));
#22156=CARTESIAN_POINT('',(-5.2,-1.,0.));
#22157=CARTESIAN_POINT('',(-4.,-1.,0.));
#22158=CARTESIAN_POINT('',(-5.2,-1.,0.));
#22159=CARTESIAN_POINT('',(-4.,-1.,0.6));
#22160=CARTESIAN_POINT('',(-4.,-1.,0.));
#22161=CARTESIAN_POINT('',(-5.2,-1.,0.6));
#22162=CARTESIAN_POINT('',(-5.2,-1.,0.6));
#22163=CARTESIAN_POINT('',(-5.2,-1.,0.));
#22164=CARTESIAN_POINT('Origin',(-5.2,1.,0.));
#22165=CARTESIAN_POINT('',(-5.2,1.,0.));
#22166=CARTESIAN_POINT('',(-5.2,1.,0.6));
#22167=CARTESIAN_POINT('Origin',(-4.6,0.,0.6));
#22168=CARTESIAN_POINT('',(-4.,1.4,0.6));
#22169=CARTESIAN_POINT('Origin',(0.,0.,0.8));
#22170=CARTESIAN_POINT('',(-0.65,-7.9602041944578E-17,1.4));
#22171=CARTESIAN_POINT('Origin',(0.,0.,1.4));
#22172=CARTESIAN_POINT('',(-0.65,-7.9602041944578E-17,0.8));
#22173=CARTESIAN_POINT('',(-0.65,-7.9602041944578E-17,0.8));
#22174=CARTESIAN_POINT('Origin',(0.,0.,0.8));
#22175=CARTESIAN_POINT('Origin',(0.,0.,0.8));
#22176=CARTESIAN_POINT('',(-0.8,-9.79717439317883E-17,1.4));
#22177=CARTESIAN_POINT('Origin',(0.,0.,1.4));
#22178=CARTESIAN_POINT('',(-0.8,-9.79717439317883E-17,0.8));
#22179=CARTESIAN_POINT('',(-0.8,-9.79717439317883E-17,0.8));
#22180=CARTESIAN_POINT('Origin',(0.,0.,0.8));
#22181=CARTESIAN_POINT('Origin',(0.,0.,1.4));
#22182=CARTESIAN_POINT('Origin',(0.,0.,0.8));
#22183=CARTESIAN_POINT('',(-3.,2.,0.8));
#22184=CARTESIAN_POINT('',(-3.2,1.8,0.8));
#22185=CARTESIAN_POINT('Origin',(-3.,1.8,0.8));
#22186=CARTESIAN_POINT('',(-3.2,-1.8,0.8));
#22187=CARTESIAN_POINT('',(-3.2,2.,0.8));
#22188=CARTESIAN_POINT('',(-3.,-2.,0.8));
#22189=CARTESIAN_POINT('Origin',(-3.,-1.8,0.8));
#22190=CARTESIAN_POINT('',(3.,-2.,0.8));
#22191=CARTESIAN_POINT('',(-3.2,-2.,0.8));
#22192=CARTESIAN_POINT('',(3.2,-1.8,0.8));
#22193=CARTESIAN_POINT('Origin',(3.,-1.8,0.8));
#22194=CARTESIAN_POINT('',(3.2,1.8,0.8));
#22195=CARTESIAN_POINT('',(3.2,-2.,0.8));
#22196=CARTESIAN_POINT('',(3.,2.,0.8));
#22197=CARTESIAN_POINT('Origin',(3.,1.8,0.8));
#22198=CARTESIAN_POINT('',(3.2,2.,0.8));
#22199=CARTESIAN_POINT('Origin',(-3.,1.8,5.2));
#22200=CARTESIAN_POINT('',(-3.,2.,5.2));
#22201=CARTESIAN_POINT('',(-3.,2.,5.2));
#22202=CARTESIAN_POINT('',(-3.2,1.8,5.2));
#22203=CARTESIAN_POINT('Origin',(-3.,1.8,5.2));
#22204=CARTESIAN_POINT('',(-3.2,1.8,5.2));
#22205=CARTESIAN_POINT('Origin',(-3.2,2.,5.2));
#22206=CARTESIAN_POINT('',(3.,2.,5.2));
#22207=CARTESIAN_POINT('',(3.,2.,5.2));
#22208=CARTESIAN_POINT('',(-1.6,2.,5.2));
#22209=CARTESIAN_POINT('Origin',(3.,1.8,5.2));
#22210=CARTESIAN_POINT('',(3.2,1.8,5.2));
#22211=CARTESIAN_POINT('',(3.2,1.8,5.2));
#22212=CARTESIAN_POINT('Origin',(3.,1.8,5.2));
#22213=CARTESIAN_POINT('Origin',(3.2,2.,5.2));
#22214=CARTESIAN_POINT('',(3.2,-1.8,5.2));
#22215=CARTESIAN_POINT('',(3.2,-1.8,5.2));
#22216=CARTESIAN_POINT('',(3.2,1.,5.2));
#22217=CARTESIAN_POINT('Origin',(-3.,-1.8,5.2));
#22218=CARTESIAN_POINT('',(-3.2,-1.8,5.2));
#22219=CARTESIAN_POINT('',(-3.2,-1.8,5.2));
#22220=CARTESIAN_POINT('',(-3.,-2.,5.2));
#22221=CARTESIAN_POINT('Origin',(-3.,-1.8,5.2));
#22222=CARTESIAN_POINT('',(-3.,-2.,5.2));
#22223=CARTESIAN_POINT('Origin',(0.,0.,0.8));
#22224=CARTESIAN_POINT('Origin',(3.2,-2.,5.2));
#22225=CARTESIAN_POINT('',(3.,-2.,5.2));
#22226=CARTESIAN_POINT('',(1.6,-2.,5.2));
#22227=CARTESIAN_POINT('',(3.,-2.,5.2));
#22228=CARTESIAN_POINT('Origin',(3.,-1.8,5.2));
#22229=CARTESIAN_POINT('Origin',(3.,-1.8,5.2));
#22230=CARTESIAN_POINT('Origin',(-3.2,-2.,5.2));
#22231=CARTESIAN_POINT('',(-3.2,-1.,5.2));
#22232=CARTESIAN_POINT('Origin',(4.,2.8,0.));
#22233=CARTESIAN_POINT('',(4.,2.8,0.));
#22234=CARTESIAN_POINT('',(-4.,2.8,0.));
#22235=CARTESIAN_POINT('',(4.,2.8,0.));
#22236=CARTESIAN_POINT('',(-4.,2.8,5.2));
#22237=CARTESIAN_POINT('',(-4.,2.8,0.));
#22238=CARTESIAN_POINT('',(4.,2.8,5.2));
#22239=CARTESIAN_POINT('',(4.,2.8,5.2));
#22240=CARTESIAN_POINT('',(4.,2.8,0.));
#22241=CARTESIAN_POINT('Origin',(4.,-2.8,0.));
#22242=CARTESIAN_POINT('',(4.,-2.8,0.));
#22243=CARTESIAN_POINT('',(4.,-2.8,5.2));
#22244=CARTESIAN_POINT('',(4.,-2.8,5.2));
#22245=CARTESIAN_POINT('',(4.,-2.8,0.));
#22246=CARTESIAN_POINT('',(4.,-2.8,0.));
#22247=CARTESIAN_POINT('',(4.,-2.8,0.));
#22248=CARTESIAN_POINT('Origin',(-4.,-2.8,0.));
#22249=CARTESIAN_POINT('',(-4.,-2.8,0.));
#22250=CARTESIAN_POINT('',(-4.,-2.8,0.));
#22251=CARTESIAN_POINT('',(-4.,-2.8,5.2));
#22252=CARTESIAN_POINT('',(-4.,-2.8,5.2));
#22253=CARTESIAN_POINT('',(-4.,-2.8,0.));
#22254=CARTESIAN_POINT('Origin',(-4.,2.8,0.));
#22255=CARTESIAN_POINT('',(-4.,2.8,0.));
#22256=CARTESIAN_POINT('',(-4.,2.8,5.2));
#22257=CARTESIAN_POINT('',(-4.,2.8,0.));
#22258=CARTESIAN_POINT('Origin',(0.,0.,5.2));
#22259=CARTESIAN_POINT('Origin',(0.,0.,0.));
#22260=CARTESIAN_POINT('',(0.,0.,0.));
#22261=CARTESIAN_POINT('Origin',(-2.35,0.,6.4));
#22262=CARTESIAN_POINT('',(-2.2079681670589,0.426326761040182,6.40000738455106));
#22263=CARTESIAN_POINT('',(-2.16703183294109,0.426272942583651,6.39999240784429));
#22264=CARTESIAN_POINT('',(-2.35,0.4263,6.4));
#22265=CARTESIAN_POINT('',(-2.1,-0.402774227945242,6.53965891057542));
#22266=CARTESIAN_POINT('Ctrl Pts',(-2.16703183294109,0.426272942583651,
6.39999240784429));
#22267=CARTESIAN_POINT('Ctrl Pts',(-2.16455261625436,0.426244983352413,
6.44427071500844));
#22268=CARTESIAN_POINT('Ctrl Pts',(-2.16207339956763,0.419380394763561,
6.488557477259));
#22269=CARTESIAN_POINT('Ctrl Pts',(-2.1595941828809,0.405813684403497,6.53068600993882));
#22270=CARTESIAN_POINT('Ctrl Pts',(-2.1556212373555,0.384073026756357,6.59819699689588));
#22271=CARTESIAN_POINT('Ctrl Pts',(-2.15164829183011,0.34512127171195,6.66016563463643));
#22272=CARTESIAN_POINT('Ctrl Pts',(-2.14767534630472,0.293711532789595,
6.70902687081076));
#22273=CARTESIAN_POINT('Ctrl Pts',(-2.14370240077932,0.242301793867241,
6.75788810698509));
#22274=CARTESIAN_POINT('Ctrl Pts',(-2.13972945525393,0.178434071066939,
6.7936419415932));
#22275=CARTESIAN_POINT('Ctrl Pts',(-2.13575650972854,0.10990720362842,6.81192661575963));
#22276=CARTESIAN_POINT('Ctrl Pts',(-2.13178356420314,0.0413803361899007,
6.83021128992606));
#22277=CARTESIAN_POINT('Ctrl Pts',(-2.12781061867775,-0.031805675886835,
6.83102680365082));
#22278=CARTESIAN_POINT('Ctrl Pts',(-2.12383767315236,-0.100723579247557,
6.81426824831305));
#22279=CARTESIAN_POINT('Ctrl Pts',(-2.11986472762697,-0.169641482608279,
6.79750969297527));
#22280=CARTESIAN_POINT('Ctrl Pts',(-2.11589178210157,-0.234291277252986,
6.76317706857497));
#22281=CARTESIAN_POINT('Ctrl Pts',(-2.11191883657618,-0.286764012116973,
6.71547162888731));
#22282=CARTESIAN_POINT('Ctrl Pts',(-2.10794589105079,-0.33923674698096,
6.66776618919964));
#22283=CARTESIAN_POINT('Ctrl Pts',(-2.10397294552539,-0.379532422064226,
6.60668793422461));
#22284=CARTESIAN_POINT('Ctrl Pts',(-2.1,-0.402774227945242,6.53965891057542));
#22285=CARTESIAN_POINT('',(-2.1,-0.0804421690761202,5.98132232055468));
#22286=CARTESIAN_POINT('Origin',(-2.1,0.,6.4));
#22287=CARTESIAN_POINT('Ctrl Pts',(-2.1,-0.0804421690761202,5.98132232055468));
#22288=CARTESIAN_POINT('Ctrl Pts',(-2.10377590012555,-0.14663424989577,
5.99407142716487));
#22289=CARTESIAN_POINT('Ctrl Pts',(-2.1075518002511,-0.209775930044154,
6.02277117104005));
#22290=CARTESIAN_POINT('Ctrl Pts',(-2.11132770037664,-0.262848123123102,
6.06432984686491));
#22291=CARTESIAN_POINT('Ctrl Pts',(-2.11530064590204,-0.318689889325856,
6.10805726275774));
#22292=CARTESIAN_POINT('Ctrl Pts',(-2.11927359142743,-0.363383793828482,
6.16602071609696));
#22293=CARTESIAN_POINT('Ctrl Pts',(-2.12324653695282,-0.391474229567156,
6.2311459484684));
#22294=CARTESIAN_POINT('Ctrl Pts',(-2.12721948247822,-0.41956466530583,
6.29627118083984));
#22295=CARTESIAN_POINT('Ctrl Pts',(-2.13119242800361,-0.431051632280552,
6.36855819224351));
#22296=CARTESIAN_POINT('Ctrl Pts',(-2.135165373529,-0.4245331350138,6.43918322464256));
#22297=CARTESIAN_POINT('Ctrl Pts',(-2.1391383190544,-0.418014637747048,
6.50980825704162));
#22298=CARTESIAN_POINT('Ctrl Pts',(-2.14311126457979,-0.393490676238824,
6.57877131043605));
#22299=CARTESIAN_POINT('Ctrl Pts',(-2.14708421010518,-0.353954606539213,
6.63765488796442));
#22300=CARTESIAN_POINT('Ctrl Pts',(-2.15105715563058,-0.314418536839601,
6.69653846549279));
#22301=CARTESIAN_POINT('Ctrl Pts',(-2.15503010115597,-0.259870358948601,
6.74534256715509));
#22302=CARTESIAN_POINT('Ctrl Pts',(-2.15900304668136,-0.196968276722384,
6.77811005889651));
#22303=CARTESIAN_POINT('Ctrl Pts',(-2.16297599220675,-0.134066194496165,
6.81087755063794));
#22304=CARTESIAN_POINT('Ctrl Pts',(-2.16694893773215,-0.0628102079347276,
6.8276084324585));
#22305=CARTESIAN_POINT('Ctrl Pts',(-2.17092188325754,0.00810215006175566,
6.82626056070251));
#22306=CARTESIAN_POINT('Ctrl Pts',(-2.17489482878293,0.0790145080582389,
6.82491268894653));
#22307=CARTESIAN_POINT('Ctrl Pts',(-2.17886777430833,0.149583237489768,
6.805486063614));
#22308=CARTESIAN_POINT('Ctrl Pts',(-2.18284071983372,0.211194676111135,
6.77035189196174));
#22309=CARTESIAN_POINT('Ctrl Pts',(-2.18681366535911,0.272806114732501,
6.73521772030948));
#22310=CARTESIAN_POINT('Ctrl Pts',(-2.19078661088451,0.325460262543706,
6.68437600233748));
#22311=CARTESIAN_POINT('Ctrl Pts',(-2.1947595564099,0.362730128342859,6.62403251342481));
#22312=CARTESIAN_POINT('Ctrl Pts',(-2.19873250193529,0.399999994142011,
6.56368902451214));
#22313=CARTESIAN_POINT('Ctrl Pts',(-2.20270544746069,0.421885577929111,
6.4938437646588));
#22314=CARTESIAN_POINT('Ctrl Pts',(-2.20667839298608,0.425715512458415,
6.42302208016789));
#22315=CARTESIAN_POINT('Ctrl Pts',(-2.20710831767702,0.426129961488313,
6.41535824722023));
#22316=CARTESIAN_POINT('Ctrl Pts',(-2.20753824236796,0.426332977570519,
6.40768298027005));
#22317=CARTESIAN_POINT('Ctrl Pts',(-2.2079681670589,0.426326761040182,6.40000738455106));
#22318=CARTESIAN_POINT('Origin',(-2.35,0.,6.4));
#22319=CARTESIAN_POINT('',(-2.3579681670589,0.426284649716722,6.39998978457651));
#22320=CARTESIAN_POINT('',(-2.31703183294109,0.426305653513777,6.40001091236462));
#22321=CARTESIAN_POINT('',(-2.35,0.4263,6.4));
#22322=CARTESIAN_POINT('Ctrl Pts',(-2.31703183294109,0.426305653513777,
6.40001091236462));
#22323=CARTESIAN_POINT('Ctrl Pts',(-2.31620090808447,0.426321019141741,
6.41484782419694));
#22324=CARTESIAN_POINT('Ctrl Pts',(-2.31536998322785,0.425561575912188,
6.42968317075982));
#22325=CARTESIAN_POINT('Ctrl Pts',(-2.31453905837123,0.42401549701117,6.44443607928542));
#22326=CARTESIAN_POINT('Ctrl Pts',(-2.31056611284584,0.416623147146128,
6.51497495105736));
#22327=CARTESIAN_POINT('Ctrl Pts',(-2.30659316732044,0.391247250234886,
6.58362917867256));
#22328=CARTESIAN_POINT('Ctrl Pts',(-2.30262022179505,0.350985201969758,
6.6420187902307));
#22329=CARTESIAN_POINT('Ctrl Pts',(-2.29864727626966,0.310723153704629,
6.70040840178883));
#22330=CARTESIAN_POINT('Ctrl Pts',(-2.29467433074426,0.255574954085614,
6.74853339728991));
#22331=CARTESIAN_POINT('Ctrl Pts',(-2.29070138521887,0.192272021883084,
6.78051961378245));
#22332=CARTESIAN_POINT('Ctrl Pts',(-2.28672843969348,0.128969089680553,
6.81250583027498));
#22333=CARTESIAN_POINT('Ctrl Pts',(-2.28275549416808,0.0575114248945075,
6.82835326775898));
#22334=CARTESIAN_POINT('Ctrl Pts',(-2.27878254864269,-0.013378811171034,
6.82612757973448));
#22335=CARTESIAN_POINT('Ctrl Pts',(-2.2748096031173,-0.0842690472365756,
6.82390189170998));
#22336=CARTESIAN_POINT('Ctrl Pts',(-2.27083665759191,-0.154591854581613,
6.80360307817698));
#22337=CARTESIAN_POINT('Ctrl Pts',(-2.26686371206651,-0.215763594163553,
6.76770882270937));
#22338=CARTESIAN_POINT('Ctrl Pts',(-2.26289076654112,-0.276935333745493,
6.73181456724177));
#22339=CARTESIAN_POINT('Ctrl Pts',(-2.25891782101573,-0.328956005564335,
6.68032486983957));
#22340=CARTESIAN_POINT('Ctrl Pts',(-2.25494487549033,-0.365475937036552,
6.61952459179481));
#22341=CARTESIAN_POINT('Ctrl Pts',(-2.25097192996494,-0.401995868508769,
6.55872431375006));
#22342=CARTESIAN_POINT('Ctrl Pts',(-2.24699898443955,-0.423015059634361,
6.48861345506275));
#22343=CARTESIAN_POINT('Ctrl Pts',(-2.24302603891415,-0.425967899647639,
6.4177497824262));
#22344=CARTESIAN_POINT('Ctrl Pts',(-2.23905309338876,-0.428920739660916,
6.34688610978966));
#22345=CARTESIAN_POINT('Ctrl Pts',(-2.23508014786337,-0.413807228561879,
6.27526962320388));
#22346=CARTESIAN_POINT('Ctrl Pts',(-2.23110720233797,-0.382472123166929,
6.21164187477894));
#22347=CARTESIAN_POINT('Ctrl Pts',(-2.22713425681258,-0.35113701777198,
6.14801412635401));
#22348=CARTESIAN_POINT('Ctrl Pts',(-2.22316131128719,-0.303580318081118,
6.09237511608992));
#22349=CARTESIAN_POINT('Ctrl Pts',(-2.2191883657618,-0.245606834378852,
6.05151616024381));
#22350=CARTESIAN_POINT('Ctrl Pts',(-2.2152154202364,-0.187633350676587,
6.0106572043977));
#22351=CARTESIAN_POINT('Ctrl Pts',(-2.21124247471101,-0.119243082962917,
5.98457830296956));
#22352=CARTESIAN_POINT('Ctrl Pts',(-2.20726952918561,-0.0487837540878456,
5.97646268493538));
#22353=CARTESIAN_POINT('Ctrl Pts',(-2.20329658366022,0.0216755747872263,
5.96834706690119));
#22354=CARTESIAN_POINT('Ctrl Pts',(-2.19932363813483,0.0942039648236993,
5.97819473226094));
#22355=CARTESIAN_POINT('Ctrl Pts',(-2.19535069260944,0.159948497199684,
6.00480361749332));
#22356=CARTESIAN_POINT('Ctrl Pts',(-2.19137774708404,0.225693029575669,
6.03141250272569));
#22357=CARTESIAN_POINT('Ctrl Pts',(-2.18740480155865,0.284653704291167,
6.07478260783069));
#22358=CARTESIAN_POINT('Ctrl Pts',(-2.18343185603326,0.329633888906202,
6.12962026666635));
#22359=CARTESIAN_POINT('Ctrl Pts',(-2.17945891050786,0.374614073521237,
6.184457925502));
#22360=CARTESIAN_POINT('Ctrl Pts',(-2.17548596498247,0.40561376803581,6.25076313806833));
#22361=CARTESIAN_POINT('Ctrl Pts',(-2.17151301945708,0.41884883516816,6.32044241243827));
#22362=CARTESIAN_POINT('Ctrl Pts',(-2.17001929061842,0.423824891681104,
6.34664008892744));
#22363=CARTESIAN_POINT('Ctrl Pts',(-2.16852556177975,0.426289788029324,
6.37331471375964));
#22364=CARTESIAN_POINT('Ctrl Pts',(-2.16703183294109,0.426272942583651,
6.39999240784429));
#22365=CARTESIAN_POINT('Ctrl Pts',(-2.2079681670589,0.426326761040182,6.40000738455106));
#22366=CARTESIAN_POINT('Ctrl Pts',(-2.21151118789336,0.426275530448026,
6.3367525956958));
#22367=CARTESIAN_POINT('Ctrl Pts',(-2.21505420872781,0.412014367364063,
6.27347547866508));
#22368=CARTESIAN_POINT('Ctrl Pts',(-2.21859722956226,0.384774767183445,
6.21639147031607));
#22369=CARTESIAN_POINT('Ctrl Pts',(-2.22257017508765,0.354229802107662,
6.15238065408364));
#22370=CARTESIAN_POINT('Ctrl Pts',(-2.22654312061304,0.307365586684588,
6.09615713074728));
#22371=CARTESIAN_POINT('Ctrl Pts',(-2.23051606613844,0.249902392017012,
6.05458357301381));
#22372=CARTESIAN_POINT('Ctrl Pts',(-2.23448901166383,0.192439197349434,
6.01301001528034));
#22373=CARTESIAN_POINT('Ctrl Pts',(-2.23846195718922,0.124377023437354,
5.98608642314976));
#22374=CARTESIAN_POINT('Ctrl Pts',(-2.24243490271462,0.0540235759521597,
5.97709910512957));
#22375=CARTESIAN_POINT('Ctrl Pts',(-2.24640784824001,-0.0163298715330345,
5.96811178710938));
#22376=CARTESIAN_POINT('Ctrl Pts',(-2.2503807937654,-0.0889745925913431,
5.97706074319959));
#22377=CARTESIAN_POINT('Ctrl Pts',(-2.2543537392908,-0.155043533545503,
6.00285365883444));
#22378=CARTESIAN_POINT('Ctrl Pts',(-2.25832668481619,-0.221112474499663,
6.02864657446929));
#22379=CARTESIAN_POINT('Ctrl Pts',(-2.26229963034158,-0.280605635349674,
6.07128344964878));
#22380=CARTESIAN_POINT('Ctrl Pts',(-2.26627257586698,-0.326261248855651,
6.1255600045331));
#22381=CARTESIAN_POINT('Ctrl Pts',(-2.27024552139237,-0.371916862361629,
6.17983655941743));
#22382=CARTESIAN_POINT('Ctrl Pts',(-2.27421846691776,-0.403734928523572,
6.24575279400659));
#22383=CARTESIAN_POINT('Ctrl Pts',(-2.27819141244315,-0.417831717081485,
6.31526293721211));
#22384=CARTESIAN_POINT('Ctrl Pts',(-2.28216435796855,-0.431928505639397,
6.38477308041763));
#22385=CARTESIAN_POINT('Ctrl Pts',(-2.28613730349394,-0.42830401659328,
6.45787713223949));
#22386=CARTESIAN_POINT('Ctrl Pts',(-2.29011024901934,-0.407400657020557,
6.52565197280568));
#22387=CARTESIAN_POINT('Ctrl Pts',(-2.29408319454473,-0.386497297447833,
6.59342681337187));
#22388=CARTESIAN_POINT('Ctrl Pts',(-2.29805614007012,-0.348315067348504,
6.65587244268238));
#22389=CARTESIAN_POINT('Ctrl Pts',(-2.30202908559551,-0.297514510269819,
6.70536671362482));
#22390=CARTESIAN_POINT('Ctrl Pts',(-2.30600203112091,-0.246713953191133,
6.75486098456727));
#22391=CARTESIAN_POINT('Ctrl Pts',(-2.3099749766463,-0.18329506913309,6.79140389714166));
#22392=CARTESIAN_POINT('Ctrl Pts',(-2.31394792217169,-0.114998801196742,
6.81053500378618));
#22393=CARTESIAN_POINT('Ctrl Pts',(-2.31792086769709,-0.0467025332603938,
6.8296661104307));
#22394=CARTESIAN_POINT('Ctrl Pts',(-2.32189381322248,0.0264711185542592,
6.83138541114536));
#22395=CARTESIAN_POINT('Ctrl Pts',(-2.32586675874787,0.0955905389447022,
6.81548304715754));
#22396=CARTESIAN_POINT('Ctrl Pts',(-2.32983970427327,0.164709959335145,
6.79958068316972));
#22397=CARTESIAN_POINT('Ctrl Pts',(-2.33381264979866,0.229775148301378,
6.76605665447942));
#22398=CARTESIAN_POINT('Ctrl Pts',(-2.33778559532405,0.282844213879021,
6.71900292206431));
#22399=CARTESIAN_POINT('Ctrl Pts',(-2.34175854084945,0.335913279456664,
6.67194918964919));
#22400=CARTESIAN_POINT('Ctrl Pts',(-2.34573148637484,0.376986221645717,
6.61136575350926));
#22401=CARTESIAN_POINT('Ctrl Pts',(-2.34970443190023,0.40104965502802,6.54464746044443));
#22402=CARTESIAN_POINT('Ctrl Pts',(-2.35245901028646,0.417733652598481,
6.49838939653));
#22403=CARTESIAN_POINT('Ctrl Pts',(-2.35521358867268,0.42624097353767,6.44918223268425));
#22404=CARTESIAN_POINT('Ctrl Pts',(-2.3579681670589,0.426284649716722,6.39998978457651));
#22405=CARTESIAN_POINT('Origin',(-2.35,0.,6.4));
#22406=CARTESIAN_POINT('',(-2.50796816705891,0.426290360635438,6.40001083203199));
#22407=CARTESIAN_POINT('',(-2.46703183294109,0.426306423912841,6.39998913682467));
#22408=CARTESIAN_POINT('',(-2.35,0.4263,6.4));
#22409=CARTESIAN_POINT('',(-2.6,-0.32233527839578,6.67898325810255));
#22410=CARTESIAN_POINT('Ctrl Pts',(-2.50796816705891,0.426290360635438,
6.40001083203199));
#22411=CARTESIAN_POINT('Ctrl Pts',(-2.51083482602818,0.426241188929821,
6.34881879719149));
#22412=CARTESIAN_POINT('Ctrl Pts',(-2.51370148499746,0.417011809736389,
6.29760951317986));
#22413=CARTESIAN_POINT('Ctrl Pts',(-2.51656814396674,0.398972669717071,
6.24971854193924));
#22414=CARTESIAN_POINT('Ctrl Pts',(-2.52054108949214,0.373971955858283,
6.18334572887142));
#22415=CARTESIAN_POINT('Ctrl Pts',(-2.52451403501753,0.332049803576913,
6.12334659907732));
#22416=CARTESIAN_POINT('Ctrl Pts',(-2.52848698054292,0.278323314671085,
6.07704505632467));
#22417=CARTESIAN_POINT('Ctrl Pts',(-2.53245992606832,0.224596825765257,
6.03074351357203));
#22418=CARTESIAN_POINT('Ctrl Pts',(-2.53643287159371,0.159066000234972,
5.99813955786084));
#22419=CARTESIAN_POINT('Ctrl Pts',(-2.5404058171191,0.089729440237079,5.98321202621739));
#22420=CARTESIAN_POINT('Ctrl Pts',(-2.5443787626445,0.0203928802391868,
5.96828449457393));
#22421=CARTESIAN_POINT('Ctrl Pts',(-2.54835170816989,-0.0527494142263132,
5.97103338699821));
#22422=CARTESIAN_POINT('Ctrl Pts',(-2.55232465369528,-0.120769354923407,
5.99112490728642));
#22423=CARTESIAN_POINT('Ctrl Pts',(-2.55629759922068,-0.188789295620503,
6.01121642757463));
#22424=CARTESIAN_POINT('Ctrl Pts',(-2.56027054474607,-0.251686882549192,
6.04865057572677));
#22425=CARTESIAN_POINT('Ctrl Pts',(-2.56424349027146,-0.301785308483965,
6.09885424668315));
#22426=CARTESIAN_POINT('Ctrl Pts',(-2.56821643579686,-0.351883734418738,
6.14905791763954));
#22427=CARTESIAN_POINT('Ctrl Pts',(-2.57218938132225,-0.389182999359593,
6.21203111140016));
#22428=CARTESIAN_POINT('Ctrl Pts',(-2.57616232684764,-0.409128604357937,
6.28009503442026));
#22429=CARTESIAN_POINT('Ctrl Pts',(-2.58013527237303,-0.429074209356281,
6.34815895744036));
#22430=CARTESIAN_POINT('Ctrl Pts',(-2.58410821789843,-0.431666154412113,
6.42131360971993));
#22431=CARTESIAN_POINT('Ctrl Pts',(-2.58808116342382,-0.416588405254627,
6.49060905834863));
#22432=CARTESIAN_POINT('Ctrl Pts',(-2.59205410894921,-0.401510656097141,
6.55990450697734));
#22433=CARTESIAN_POINT('Ctrl Pts',(-2.59602705447461,-0.368763212726337,
6.62534075195518));
#22434=CARTESIAN_POINT('Ctrl Pts',(-2.6,-0.322335278395778,6.67898325810255));
#22435=CARTESIAN_POINT('',(-2.6,0.322364416527282,6.67900379523473));
#22436=CARTESIAN_POINT('Origin',(-2.6,0.,6.4));
#22437=CARTESIAN_POINT('Ctrl Pts',(-2.6,0.322364416527282,6.67900379523473));
#22438=CARTESIAN_POINT('Ctrl Pts',(-2.59622409987445,0.278227326350059,
6.7299532665394));
#22439=CARTESIAN_POINT('Ctrl Pts',(-2.5924481997489,0.221801779901377,6.77028569095882));
#22440=CARTESIAN_POINT('Ctrl Pts',(-2.58867229962336,0.159274815469995,
6.79546821970908));
#22441=CARTESIAN_POINT('Ctrl Pts',(-2.58469935409796,0.0934848805420922,
6.8219648990676));
#22442=CARTESIAN_POINT('Ctrl Pts',(-2.58072640857257,0.0209401066261879,
6.83168923038829));
#22443=CARTESIAN_POINT('Ctrl Pts',(-2.57675346304718,-0.0495052156044451,
6.82345364573744));
#22444=CARTESIAN_POINT('Ctrl Pts',(-2.57278051752178,-0.119950537835078,
6.81521806108658));
#22445=CARTESIAN_POINT('Ctrl Pts',(-2.56880757199639,-0.18829640838044,
6.78902256046417));
#22446=CARTESIAN_POINT('Ctrl Pts',(-2.564834626471,-0.246200230888236,6.74806486065615));
#22447=CARTESIAN_POINT('Ctrl Pts',(-2.5608616809456,-0.304104053396033,
6.70710716084812));
#22448=CARTESIAN_POINT('Ctrl Pts',(-2.55688873542021,-0.351565827866263,
6.65138726185447));
#22449=CARTESIAN_POINT('Ctrl Pts',(-2.55291578989482,-0.382792466430557,
6.58770623363867));
#22450=CARTESIAN_POINT('Ctrl Pts',(-2.54894284436942,-0.414019104994851,
6.52402520542287));
#22451=CARTESIAN_POINT('Ctrl Pts',(-2.54496989884403,-0.429010607653208,
6.45238304798492));
#22452=CARTESIAN_POINT('Ctrl Pts',(-2.54099695331864,-0.425937046871258,
6.3815245022355));
#22453=CARTESIAN_POINT('Ctrl Pts',(-2.53702400779324,-0.422863486089309,
6.31066595648609));
#22454=CARTESIAN_POINT('Ctrl Pts',(-2.53305106226785,-0.401724861867054,
6.24059102242521));
#22455=CARTESIAN_POINT('Ctrl Pts',(-2.52907811674246,-0.36510139236472,
6.17985305598722));
#22456=CARTESIAN_POINT('Ctrl Pts',(-2.52510517121707,-0.328477922862385,
6.11911508954922));
#22457=CARTESIAN_POINT('Ctrl Pts',(-2.52113222569167,-0.276369608079971,
6.06771409073411));
#22458=CARTESIAN_POINT('Ctrl Pts',(-2.51715928016628,-0.215136804720175,
6.03192410620715));
#22459=CARTESIAN_POINT('Ctrl Pts',(-2.51318633464089,-0.153904001360379,
5.99613412168019));
#22460=CARTESIAN_POINT('Ctrl Pts',(-2.50921338911549,-0.0835467094232002,
5.97595515144138));
#22461=CARTESIAN_POINT('Ctrl Pts',(-2.5052404435901,-0.01265278349094,5.97385024536399));
#22462=CARTESIAN_POINT('Ctrl Pts',(-2.50126749806471,0.0582411424413201,
5.9717453392866));
#22463=CARTESIAN_POINT('Ctrl Pts',(-2.49729455253931,0.129671702368662,
5.98771449737062));
#22464=CARTESIAN_POINT('Ctrl Pts',(-2.49332160701392,0.192920046362828,
6.01980851841896));
#22465=CARTESIAN_POINT('Ctrl Pts',(-2.48934866148853,0.256168390356993,
6.05190253946729));
#22466=CARTESIAN_POINT('Ctrl Pts',(-2.48537571596313,0.311234518417982,
6.10012142347994));
#22467=CARTESIAN_POINT('Ctrl Pts',(-2.48140277043774,0.351397028106915,
6.15857954622212));
#22468=CARTESIAN_POINT('Ctrl Pts',(-2.47742982491235,0.391559537795848,
6.21703766896431));
#22469=CARTESIAN_POINT('Ctrl Pts',(-2.47345687938695,0.416818429112726,
6.28573503043603));
#22470=CARTESIAN_POINT('Ctrl Pts',(-2.46948393386156,0.424090588766216,
6.35628639435329));
#22471=CARTESIAN_POINT('Ctrl Pts',(-2.46866656688807,0.425586713766852,
6.37080115536172));
#22472=CARTESIAN_POINT('Ctrl Pts',(-2.46784919991458,0.426321529342654,
6.385394389189));
#22473=CARTESIAN_POINT('Ctrl Pts',(-2.46703183294109,0.426306423912841,
6.39998913682467));
#22474=CARTESIAN_POINT('Origin',(2.35,0.,6.4));
#22475=CARTESIAN_POINT('',(2.2079681670589,-0.426326761040182,6.40000738455106));
#22476=CARTESIAN_POINT('',(2.16703183294109,-0.426272942583651,6.39999240784429));
#22477=CARTESIAN_POINT('',(2.35,-0.4263,6.4));
#22478=CARTESIAN_POINT('',(2.1,0.402774227945242,6.53965891057542));
#22479=CARTESIAN_POINT('Ctrl Pts',(2.16703183294109,-0.426272942583651,
6.39999240784429));
#22480=CARTESIAN_POINT('Ctrl Pts',(2.16455261625436,-0.426244983352413,
6.44427071500844));
#22481=CARTESIAN_POINT('Ctrl Pts',(2.16207339956763,-0.419380394763561,
6.488557477259));
#22482=CARTESIAN_POINT('Ctrl Pts',(2.1595941828809,-0.405813684403497,6.53068600993882));
#22483=CARTESIAN_POINT('Ctrl Pts',(2.1556212373555,-0.384073026756357,6.59819699689588));
#22484=CARTESIAN_POINT('Ctrl Pts',(2.15164829183011,-0.34512127171195,6.66016563463643));
#22485=CARTESIAN_POINT('Ctrl Pts',(2.14767534630472,-0.293711532789595,
6.70902687081076));
#22486=CARTESIAN_POINT('Ctrl Pts',(2.14370240077932,-0.242301793867241,
6.75788810698509));
#22487=CARTESIAN_POINT('Ctrl Pts',(2.13972945525393,-0.178434071066939,
6.7936419415932));
#22488=CARTESIAN_POINT('Ctrl Pts',(2.13575650972854,-0.10990720362842,6.81192661575963));
#22489=CARTESIAN_POINT('Ctrl Pts',(2.13178356420314,-0.0413803361899007,
6.83021128992606));
#22490=CARTESIAN_POINT('Ctrl Pts',(2.12781061867775,0.031805675886835,6.83102680365082));
#22491=CARTESIAN_POINT('Ctrl Pts',(2.12383767315236,0.100723579247557,6.81426824831305));
#22492=CARTESIAN_POINT('Ctrl Pts',(2.11986472762697,0.169641482608279,6.79750969297527));
#22493=CARTESIAN_POINT('Ctrl Pts',(2.11589178210157,0.234291277252986,6.76317706857497));
#22494=CARTESIAN_POINT('Ctrl Pts',(2.11191883657618,0.286764012116973,6.71547162888731));
#22495=CARTESIAN_POINT('Ctrl Pts',(2.10794589105079,0.33923674698096,6.66776618919964));
#22496=CARTESIAN_POINT('Ctrl Pts',(2.10397294552539,0.379532422064226,6.60668793422461));
#22497=CARTESIAN_POINT('Ctrl Pts',(2.1,0.402774227945242,6.53965891057542));
#22498=CARTESIAN_POINT('',(2.1,0.0804421690761202,5.98132232055468));
#22499=CARTESIAN_POINT('Origin',(2.1,0.,6.4));
#22500=CARTESIAN_POINT('Ctrl Pts',(2.1,0.0804421690761202,5.98132232055468));
#22501=CARTESIAN_POINT('Ctrl Pts',(2.10377590012555,0.14663424989577,5.99407142716487));
#22502=CARTESIAN_POINT('Ctrl Pts',(2.1075518002511,0.209775930044154,6.02277117104005));
#22503=CARTESIAN_POINT('Ctrl Pts',(2.11132770037664,0.262848123123102,6.06432984686491));
#22504=CARTESIAN_POINT('Ctrl Pts',(2.11530064590204,0.318689889325856,6.10805726275774));
#22505=CARTESIAN_POINT('Ctrl Pts',(2.11927359142743,0.363383793828482,6.16602071609696));
#22506=CARTESIAN_POINT('Ctrl Pts',(2.12324653695282,0.391474229567156,6.2311459484684));
#22507=CARTESIAN_POINT('Ctrl Pts',(2.12721948247822,0.41956466530583,6.29627118083984));
#22508=CARTESIAN_POINT('Ctrl Pts',(2.13119242800361,0.431051632280552,6.36855819224351));
#22509=CARTESIAN_POINT('Ctrl Pts',(2.135165373529,0.4245331350138,6.43918322464256));
#22510=CARTESIAN_POINT('Ctrl Pts',(2.1391383190544,0.418014637747048,6.50980825704162));
#22511=CARTESIAN_POINT('Ctrl Pts',(2.14311126457979,0.393490676238824,6.57877131043605));
#22512=CARTESIAN_POINT('Ctrl Pts',(2.14708421010518,0.353954606539213,6.63765488796442));
#22513=CARTESIAN_POINT('Ctrl Pts',(2.15105715563058,0.314418536839601,6.69653846549279));
#22514=CARTESIAN_POINT('Ctrl Pts',(2.15503010115597,0.259870358948601,6.74534256715509));
#22515=CARTESIAN_POINT('Ctrl Pts',(2.15900304668136,0.196968276722384,6.77811005889651));
#22516=CARTESIAN_POINT('Ctrl Pts',(2.16297599220675,0.134066194496165,6.81087755063794));
#22517=CARTESIAN_POINT('Ctrl Pts',(2.16694893773215,0.0628102079347276,
6.8276084324585));
#22518=CARTESIAN_POINT('Ctrl Pts',(2.17092188325754,-0.00810215006175566,
6.82626056070251));
#22519=CARTESIAN_POINT('Ctrl Pts',(2.17489482878293,-0.0790145080582389,
6.82491268894653));
#22520=CARTESIAN_POINT('Ctrl Pts',(2.17886777430833,-0.149583237489768,
6.805486063614));
#22521=CARTESIAN_POINT('Ctrl Pts',(2.18284071983372,-0.211194676111135,
6.77035189196174));
#22522=CARTESIAN_POINT('Ctrl Pts',(2.18681366535911,-0.272806114732501,
6.73521772030948));
#22523=CARTESIAN_POINT('Ctrl Pts',(2.19078661088451,-0.325460262543706,
6.68437600233748));
#22524=CARTESIAN_POINT('Ctrl Pts',(2.1947595564099,-0.362730128342859,6.62403251342481));
#22525=CARTESIAN_POINT('Ctrl Pts',(2.19873250193529,-0.399999994142011,
6.56368902451214));
#22526=CARTESIAN_POINT('Ctrl Pts',(2.20270544746069,-0.421885577929111,
6.4938437646588));
#22527=CARTESIAN_POINT('Ctrl Pts',(2.20667839298608,-0.425715512458415,
6.42302208016789));
#22528=CARTESIAN_POINT('Ctrl Pts',(2.20710831767702,-0.426129961488313,
6.41535824722023));
#22529=CARTESIAN_POINT('Ctrl Pts',(2.20753824236796,-0.426332977570519,
6.40768298027005));
#22530=CARTESIAN_POINT('Ctrl Pts',(2.2079681670589,-0.426326761040182,6.40000738455106));
#22531=CARTESIAN_POINT('Origin',(2.35,0.,6.4));
#22532=CARTESIAN_POINT('',(2.3579681670589,-0.426284649716722,6.39998978457651));
#22533=CARTESIAN_POINT('',(2.31703183294109,-0.426305653513777,6.40001091236462));
#22534=CARTESIAN_POINT('',(2.35,-0.4263,6.4));
#22535=CARTESIAN_POINT('Ctrl Pts',(2.31703183294109,-0.426305653513777,
6.40001091236462));
#22536=CARTESIAN_POINT('Ctrl Pts',(2.31620090808447,-0.426321019141741,
6.41484782419694));
#22537=CARTESIAN_POINT('Ctrl Pts',(2.31536998322785,-0.425561575912188,
6.42968317075982));
#22538=CARTESIAN_POINT('Ctrl Pts',(2.31453905837123,-0.42401549701117,6.44443607928542));
#22539=CARTESIAN_POINT('Ctrl Pts',(2.31056611284584,-0.416623147146128,
6.51497495105736));
#22540=CARTESIAN_POINT('Ctrl Pts',(2.30659316732044,-0.391247250234886,
6.58362917867256));
#22541=CARTESIAN_POINT('Ctrl Pts',(2.30262022179505,-0.350985201969758,
6.6420187902307));
#22542=CARTESIAN_POINT('Ctrl Pts',(2.29864727626966,-0.310723153704629,
6.70040840178883));
#22543=CARTESIAN_POINT('Ctrl Pts',(2.29467433074426,-0.255574954085614,
6.74853339728991));
#22544=CARTESIAN_POINT('Ctrl Pts',(2.29070138521887,-0.192272021883084,
6.78051961378245));
#22545=CARTESIAN_POINT('Ctrl Pts',(2.28672843969348,-0.128969089680553,
6.81250583027498));
#22546=CARTESIAN_POINT('Ctrl Pts',(2.28275549416808,-0.0575114248945075,
6.82835326775898));
#22547=CARTESIAN_POINT('Ctrl Pts',(2.27878254864269,0.013378811171034,6.82612757973448));
#22548=CARTESIAN_POINT('Ctrl Pts',(2.2748096031173,0.0842690472365756,6.82390189170998));
#22549=CARTESIAN_POINT('Ctrl Pts',(2.27083665759191,0.154591854581613,6.80360307817698));
#22550=CARTESIAN_POINT('Ctrl Pts',(2.26686371206651,0.215763594163553,6.76770882270937));
#22551=CARTESIAN_POINT('Ctrl Pts',(2.26289076654112,0.276935333745493,6.73181456724177));
#22552=CARTESIAN_POINT('Ctrl Pts',(2.25891782101573,0.328956005564335,6.68032486983957));
#22553=CARTESIAN_POINT('Ctrl Pts',(2.25494487549033,0.365475937036552,6.61952459179481));
#22554=CARTESIAN_POINT('Ctrl Pts',(2.25097192996494,0.401995868508769,6.55872431375006));
#22555=CARTESIAN_POINT('Ctrl Pts',(2.24699898443955,0.423015059634361,6.48861345506275));
#22556=CARTESIAN_POINT('Ctrl Pts',(2.24302603891415,0.425967899647639,6.4177497824262));
#22557=CARTESIAN_POINT('Ctrl Pts',(2.23905309338876,0.428920739660916,6.34688610978966));
#22558=CARTESIAN_POINT('Ctrl Pts',(2.23508014786337,0.413807228561879,6.27526962320388));
#22559=CARTESIAN_POINT('Ctrl Pts',(2.23110720233797,0.382472123166929,6.21164187477894));
#22560=CARTESIAN_POINT('Ctrl Pts',(2.22713425681258,0.35113701777198,6.14801412635401));
#22561=CARTESIAN_POINT('Ctrl Pts',(2.22316131128719,0.303580318081118,6.09237511608992));
#22562=CARTESIAN_POINT('Ctrl Pts',(2.2191883657618,0.245606834378852,6.05151616024381));
#22563=CARTESIAN_POINT('Ctrl Pts',(2.2152154202364,0.187633350676587,6.0106572043977));
#22564=CARTESIAN_POINT('Ctrl Pts',(2.21124247471101,0.119243082962917,5.98457830296956));
#22565=CARTESIAN_POINT('Ctrl Pts',(2.20726952918561,0.0487837540878456,
5.97646268493538));
#22566=CARTESIAN_POINT('Ctrl Pts',(2.20329658366022,-0.0216755747872263,
5.96834706690119));
#22567=CARTESIAN_POINT('Ctrl Pts',(2.19932363813483,-0.0942039648236993,
5.97819473226094));
#22568=CARTESIAN_POINT('Ctrl Pts',(2.19535069260944,-0.159948497199684,
6.00480361749332));
#22569=CARTESIAN_POINT('Ctrl Pts',(2.19137774708404,-0.225693029575669,
6.03141250272569));
#22570=CARTESIAN_POINT('Ctrl Pts',(2.18740480155865,-0.284653704291167,
6.07478260783069));
#22571=CARTESIAN_POINT('Ctrl Pts',(2.18343185603326,-0.329633888906202,
6.12962026666635));
#22572=CARTESIAN_POINT('Ctrl Pts',(2.17945891050786,-0.374614073521237,
6.184457925502));
#22573=CARTESIAN_POINT('Ctrl Pts',(2.17548596498247,-0.40561376803581,6.25076313806833));
#22574=CARTESIAN_POINT('Ctrl Pts',(2.17151301945708,-0.41884883516816,6.32044241243827));
#22575=CARTESIAN_POINT('Ctrl Pts',(2.17001929061842,-0.423824891681104,
6.34664008892744));
#22576=CARTESIAN_POINT('Ctrl Pts',(2.16852556177975,-0.426289788029324,
6.37331471375964));
#22577=CARTESIAN_POINT('Ctrl Pts',(2.16703183294109,-0.426272942583651,
6.39999240784429));
#22578=CARTESIAN_POINT('Ctrl Pts',(2.2079681670589,-0.426326761040182,6.40000738455106));
#22579=CARTESIAN_POINT('Ctrl Pts',(2.21151118789336,-0.426275530448026,
6.3367525956958));
#22580=CARTESIAN_POINT('Ctrl Pts',(2.21505420872781,-0.412014367364063,
6.27347547866508));
#22581=CARTESIAN_POINT('Ctrl Pts',(2.21859722956226,-0.384774767183445,
6.21639147031607));
#22582=CARTESIAN_POINT('Ctrl Pts',(2.22257017508765,-0.354229802107662,
6.15238065408364));
#22583=CARTESIAN_POINT('Ctrl Pts',(2.22654312061304,-0.307365586684588,
6.09615713074728));
#22584=CARTESIAN_POINT('Ctrl Pts',(2.23051606613844,-0.249902392017012,
6.05458357301381));
#22585=CARTESIAN_POINT('Ctrl Pts',(2.23448901166383,-0.192439197349434,
6.01301001528034));
#22586=CARTESIAN_POINT('Ctrl Pts',(2.23846195718922,-0.124377023437354,
5.98608642314976));
#22587=CARTESIAN_POINT('Ctrl Pts',(2.24243490271462,-0.0540235759521597,
5.97709910512957));
#22588=CARTESIAN_POINT('Ctrl Pts',(2.24640784824001,0.0163298715330345,
5.96811178710938));
#22589=CARTESIAN_POINT('Ctrl Pts',(2.2503807937654,0.0889745925913431,5.97706074319959));
#22590=CARTESIAN_POINT('Ctrl Pts',(2.2543537392908,0.155043533545503,6.00285365883444));
#22591=CARTESIAN_POINT('Ctrl Pts',(2.25832668481619,0.221112474499663,6.02864657446929));
#22592=CARTESIAN_POINT('Ctrl Pts',(2.26229963034158,0.280605635349674,6.07128344964878));
#22593=CARTESIAN_POINT('Ctrl Pts',(2.26627257586698,0.326261248855651,6.1255600045331));
#22594=CARTESIAN_POINT('Ctrl Pts',(2.27024552139237,0.371916862361629,6.17983655941743));
#22595=CARTESIAN_POINT('Ctrl Pts',(2.27421846691776,0.403734928523572,6.24575279400659));
#22596=CARTESIAN_POINT('Ctrl Pts',(2.27819141244315,0.417831717081485,6.31526293721211));
#22597=CARTESIAN_POINT('Ctrl Pts',(2.28216435796855,0.431928505639397,6.38477308041763));
#22598=CARTESIAN_POINT('Ctrl Pts',(2.28613730349394,0.42830401659328,6.45787713223949));
#22599=CARTESIAN_POINT('Ctrl Pts',(2.29011024901934,0.407400657020557,6.52565197280568));
#22600=CARTESIAN_POINT('Ctrl Pts',(2.29408319454473,0.386497297447833,6.59342681337187));
#22601=CARTESIAN_POINT('Ctrl Pts',(2.29805614007012,0.348315067348504,6.65587244268238));
#22602=CARTESIAN_POINT('Ctrl Pts',(2.30202908559551,0.297514510269819,6.70536671362482));
#22603=CARTESIAN_POINT('Ctrl Pts',(2.30600203112091,0.246713953191133,6.75486098456727));
#22604=CARTESIAN_POINT('Ctrl Pts',(2.3099749766463,0.18329506913309,6.79140389714166));
#22605=CARTESIAN_POINT('Ctrl Pts',(2.31394792217169,0.114998801196742,6.81053500378618));
#22606=CARTESIAN_POINT('Ctrl Pts',(2.31792086769709,0.0467025332603938,
6.8296661104307));
#22607=CARTESIAN_POINT('Ctrl Pts',(2.32189381322248,-0.0264711185542592,
6.83138541114536));
#22608=CARTESIAN_POINT('Ctrl Pts',(2.32586675874787,-0.0955905389447022,
6.81548304715754));
#22609=CARTESIAN_POINT('Ctrl Pts',(2.32983970427327,-0.164709959335145,
6.79958068316972));
#22610=CARTESIAN_POINT('Ctrl Pts',(2.33381264979866,-0.229775148301378,
6.76605665447942));
#22611=CARTESIAN_POINT('Ctrl Pts',(2.33778559532405,-0.282844213879021,
6.71900292206431));
#22612=CARTESIAN_POINT('Ctrl Pts',(2.34175854084945,-0.335913279456664,
6.67194918964919));
#22613=CARTESIAN_POINT('Ctrl Pts',(2.34573148637484,-0.376986221645717,
6.61136575350926));
#22614=CARTESIAN_POINT('Ctrl Pts',(2.34970443190023,-0.40104965502802,6.54464746044443));
#22615=CARTESIAN_POINT('Ctrl Pts',(2.35245901028646,-0.417733652598481,
6.49838939653));
#22616=CARTESIAN_POINT('Ctrl Pts',(2.35521358867268,-0.42624097353767,6.44918223268425));
#22617=CARTESIAN_POINT('Ctrl Pts',(2.3579681670589,-0.426284649716722,6.39998978457651));
#22618=CARTESIAN_POINT('Origin',(2.35,0.,6.4));
#22619=CARTESIAN_POINT('',(2.50796816705891,-0.426290360635438,6.40001083203199));
#22620=CARTESIAN_POINT('',(2.46703183294109,-0.426306423912841,6.39998913682467));
#22621=CARTESIAN_POINT('',(2.35,-0.4263,6.4));
#22622=CARTESIAN_POINT('',(2.6,0.32233527839578,6.67898325810255));
#22623=CARTESIAN_POINT('Ctrl Pts',(2.50796816705891,-0.426290360635438,
6.40001083203199));
#22624=CARTESIAN_POINT('Ctrl Pts',(2.51083482602818,-0.426241188929821,
6.34881879719149));
#22625=CARTESIAN_POINT('Ctrl Pts',(2.51370148499746,-0.417011809736389,
6.29760951317986));
#22626=CARTESIAN_POINT('Ctrl Pts',(2.51656814396674,-0.398972669717071,
6.24971854193924));
#22627=CARTESIAN_POINT('Ctrl Pts',(2.52054108949214,-0.373971955858283,
6.18334572887142));
#22628=CARTESIAN_POINT('Ctrl Pts',(2.52451403501753,-0.332049803576913,
6.12334659907732));
#22629=CARTESIAN_POINT('Ctrl Pts',(2.52848698054292,-0.278323314671085,
6.07704505632467));
#22630=CARTESIAN_POINT('Ctrl Pts',(2.53245992606832,-0.224596825765257,
6.03074351357203));
#22631=CARTESIAN_POINT('Ctrl Pts',(2.53643287159371,-0.159066000234972,
5.99813955786084));
#22632=CARTESIAN_POINT('Ctrl Pts',(2.5404058171191,-0.089729440237079,5.98321202621739));
#22633=CARTESIAN_POINT('Ctrl Pts',(2.5443787626445,-0.0203928802391868,
5.96828449457393));
#22634=CARTESIAN_POINT('Ctrl Pts',(2.54835170816989,0.0527494142263132,
5.97103338699821));
#22635=CARTESIAN_POINT('Ctrl Pts',(2.55232465369528,0.120769354923407,5.99112490728642));
#22636=CARTESIAN_POINT('Ctrl Pts',(2.55629759922068,0.188789295620503,6.01121642757463));
#22637=CARTESIAN_POINT('Ctrl Pts',(2.56027054474607,0.251686882549192,6.04865057572677));
#22638=CARTESIAN_POINT('Ctrl Pts',(2.56424349027146,0.301785308483965,6.09885424668315));
#22639=CARTESIAN_POINT('Ctrl Pts',(2.56821643579686,0.351883734418738,6.14905791763954));
#22640=CARTESIAN_POINT('Ctrl Pts',(2.57218938132225,0.389182999359593,6.21203111140016));
#22641=CARTESIAN_POINT('Ctrl Pts',(2.57616232684764,0.409128604357937,6.28009503442026));
#22642=CARTESIAN_POINT('Ctrl Pts',(2.58013527237303,0.429074209356281,6.34815895744036));
#22643=CARTESIAN_POINT('Ctrl Pts',(2.58410821789843,0.431666154412113,6.42131360971993));
#22644=CARTESIAN_POINT('Ctrl Pts',(2.58808116342382,0.416588405254627,6.49060905834863));
#22645=CARTESIAN_POINT('Ctrl Pts',(2.59205410894921,0.401510656097141,6.55990450697734));
#22646=CARTESIAN_POINT('Ctrl Pts',(2.59602705447461,0.368763212726337,6.62534075195518));
#22647=CARTESIAN_POINT('Ctrl Pts',(2.6,0.322335278395778,6.67898325810255));
#22648=CARTESIAN_POINT('',(2.6,-0.322364416527282,6.67900379523473));
#22649=CARTESIAN_POINT('Origin',(2.6,0.,6.4));
#22650=CARTESIAN_POINT('Ctrl Pts',(2.6,-0.322364416527282,6.67900379523473));
#22651=CARTESIAN_POINT('Ctrl Pts',(2.59622409987445,-0.278227326350059,
6.7299532665394));
#22652=CARTESIAN_POINT('Ctrl Pts',(2.5924481997489,-0.221801779901377,6.77028569095882));
#22653=CARTESIAN_POINT('Ctrl Pts',(2.58867229962336,-0.159274815469995,
6.79546821970908));
#22654=CARTESIAN_POINT('Ctrl Pts',(2.58469935409796,-0.0934848805420922,
6.8219648990676));
#22655=CARTESIAN_POINT('Ctrl Pts',(2.58072640857257,-0.0209401066261879,
6.83168923038829));
#22656=CARTESIAN_POINT('Ctrl Pts',(2.57675346304718,0.0495052156044451,
6.82345364573744));
#22657=CARTESIAN_POINT('Ctrl Pts',(2.57278051752178,0.119950537835078,6.81521806108658));
#22658=CARTESIAN_POINT('Ctrl Pts',(2.56880757199639,0.18829640838044,6.78902256046417));
#22659=CARTESIAN_POINT('Ctrl Pts',(2.564834626471,0.246200230888236,6.74806486065615));
#22660=CARTESIAN_POINT('Ctrl Pts',(2.5608616809456,0.304104053396033,6.70710716084812));
#22661=CARTESIAN_POINT('Ctrl Pts',(2.55688873542021,0.351565827866263,6.65138726185447));
#22662=CARTESIAN_POINT('Ctrl Pts',(2.55291578989482,0.382792466430557,6.58770623363867));
#22663=CARTESIAN_POINT('Ctrl Pts',(2.54894284436942,0.414019104994851,6.52402520542287));
#22664=CARTESIAN_POINT('Ctrl Pts',(2.54496989884403,0.429010607653208,6.45238304798492));
#22665=CARTESIAN_POINT('Ctrl Pts',(2.54099695331864,0.425937046871258,6.3815245022355));
#22666=CARTESIAN_POINT('Ctrl Pts',(2.53702400779324,0.422863486089309,6.31066595648609));
#22667=CARTESIAN_POINT('Ctrl Pts',(2.53305106226785,0.401724861867054,6.24059102242521));
#22668=CARTESIAN_POINT('Ctrl Pts',(2.52907811674246,0.36510139236472,6.17985305598722));
#22669=CARTESIAN_POINT('Ctrl Pts',(2.52510517121707,0.328477922862385,6.11911508954922));
#22670=CARTESIAN_POINT('Ctrl Pts',(2.52113222569167,0.276369608079971,6.06771409073411));
#22671=CARTESIAN_POINT('Ctrl Pts',(2.51715928016628,0.215136804720175,6.03192410620715));
#22672=CARTESIAN_POINT('Ctrl Pts',(2.51318633464089,0.153904001360379,5.99613412168019));
#22673=CARTESIAN_POINT('Ctrl Pts',(2.50921338911549,0.0835467094232002,
5.97595515144138));
#22674=CARTESIAN_POINT('Ctrl Pts',(2.5052404435901,0.01265278349094,5.97385024536399));
#22675=CARTESIAN_POINT('Ctrl Pts',(2.50126749806471,-0.0582411424413201,
5.9717453392866));
#22676=CARTESIAN_POINT('Ctrl Pts',(2.49729455253931,-0.129671702368662,
5.98771449737062));
#22677=CARTESIAN_POINT('Ctrl Pts',(2.49332160701392,-0.192920046362828,
6.01980851841896));
#22678=CARTESIAN_POINT('Ctrl Pts',(2.48934866148853,-0.256168390356993,
6.05190253946729));
#22679=CARTESIAN_POINT('Ctrl Pts',(2.48537571596313,-0.311234518417982,
6.10012142347994));
#22680=CARTESIAN_POINT('Ctrl Pts',(2.48140277043774,-0.351397028106915,
6.15857954622212));
#22681=CARTESIAN_POINT('Ctrl Pts',(2.47742982491235,-0.391559537795848,
6.21703766896431));
#22682=CARTESIAN_POINT('Ctrl Pts',(2.47345687938695,-0.416818429112726,
6.28573503043603));
#22683=CARTESIAN_POINT('Ctrl Pts',(2.46948393386156,-0.424090588766216,
6.35628639435329));
#22684=CARTESIAN_POINT('Ctrl Pts',(2.46866656688807,-0.425586713766852,
6.37080115536172));
#22685=CARTESIAN_POINT('Ctrl Pts',(2.46784919991458,-0.426321529342654,
6.385394389189));
#22686=CARTESIAN_POINT('Ctrl Pts',(2.46703183294109,-0.426306423912841,
6.39998913682467));
#22687=CARTESIAN_POINT('Origin',(-2.93123464956316,0.,6.4));
#22688=CARTESIAN_POINT('',(-2.11876535043684,0.509867636461186,6.39999091897679));
#22689=CARTESIAN_POINT('',(-2.10623464956316,0.509830151085518,6.39998162138192));
#22690=CARTESIAN_POINT('',(-2.93123464956316,0.5099,6.4));
#22691=CARTESIAN_POINT('',(-2.1,0.492610334572591,6.53165511107542));
#22692=CARTESIAN_POINT('Ctrl Pts',(-2.10623464956316,0.509830060291024,
6.39998159749211));
#22693=CARTESIAN_POINT('Ctrl Pts',(-2.1041564330421,0.509817985963964,6.44437440316355));
#22694=CARTESIAN_POINT('Ctrl Pts',(-2.10207821652105,0.504071192426059,
6.48877233215731));
#22695=CARTESIAN_POINT('Ctrl Pts',(-2.1,0.492610334572592,6.53165511107541));
#22696=CARTESIAN_POINT('',(-2.1,0.360348823959177,6.76081852140067));
#22697=CARTESIAN_POINT('Origin',(-2.1,0.,6.4));
#22698=CARTESIAN_POINT('Ctrl Pts',(-2.11876535043684,0.509867636461186,
6.39999091897678));
#22699=CARTESIAN_POINT('Ctrl Pts',(-2.11628613375011,0.509834194256146,
6.45295246911284));
#22700=CARTESIAN_POINT('Ctrl Pts',(-2.11003101693783,0.489118231027634,
6.58660111045784));
#22701=CARTESIAN_POINT('Ctrl Pts',(-2.10377590012555,0.417372467378852,
6.70381704168278));
#22702=CARTESIAN_POINT('Ctrl Pts',(-2.1,0.360348823959177,6.76081852140067));
#22703=CARTESIAN_POINT('Origin',(-2.93123464956316,0.,6.4));
#22704=CARTESIAN_POINT('',(-2.26876535043684,0.509906762201912,6.4000130523451));
#22705=CARTESIAN_POINT('',(-2.25623464956316,0.509932009041494,6.40000883270604));
#22706=CARTESIAN_POINT('',(-2.93123464956316,0.5099,6.4));
#22707=CARTESIAN_POINT('Ctrl Pts',(-2.25623464956316,0.509932009041494,
6.40000883270604));
#22708=CARTESIAN_POINT('Ctrl Pts',(-2.25580472487222,0.509939444670906,
6.40918965901876));
#22709=CARTESIAN_POINT('Ctrl Pts',(-2.25140185465588,0.507452628870696,
6.50320671872761));
#22710=CARTESIAN_POINT('Ctrl Pts',(-2.24302603891415,0.45226492573298,6.67933176541862));
#22711=CARTESIAN_POINT('Ctrl Pts',(-2.23110720233797,0.263325094846747,
6.86176802153349));
#22712=CARTESIAN_POINT('Ctrl Pts',(-2.2191883657618,0.0101020467317839,
6.93147693256131));
#22713=CARTESIAN_POINT('Ctrl Pts',(-2.20726952918561,-0.245587098572064,
6.87144120673232));
#22714=CARTESIAN_POINT('Ctrl Pts',(-2.19535069260943,-0.441323311848774,
6.69631656607358));
#22715=CARTESIAN_POINT('Ctrl Pts',(-2.18343185603326,-0.529323086465549,
6.44885519432254));
#22716=CARTESIAN_POINT('Ctrl Pts',(-2.17151301945708,-0.488104195118536,
6.18946640393034));
#22717=CARTESIAN_POINT('Ctrl Pts',(-2.1595941828809,-0.327728249264285,
5.98147509599461));
#22718=CARTESIAN_POINT('Ctrl Pts',(-2.14767534630472,-0.0873481558956701,
5.87565064933844));
#22719=CARTESIAN_POINT('Ctrl Pts',(-2.13575650972854,0.174357740366956,
5.89783918404992));
#22720=CARTESIAN_POINT('Ctrl Pts',(-2.12383767315236,0.393492635182685,
6.04259742479108));
#22721=CARTESIAN_POINT('Ctrl Pts',(-2.11399705309723,0.495113210733723,
6.23418199944647));
#22722=CARTESIAN_POINT('Ctrl Pts',(-2.1081293785675,0.509841068565406,6.35950827065745));
#22723=CARTESIAN_POINT('Ctrl Pts',(-2.10623464956316,0.509830060291024,
6.39998159749211));
#22724=CARTESIAN_POINT('Ctrl Pts',(-2.26876535043684,0.509906762201912,
6.4000130523451));
#22725=CARTESIAN_POINT('Ctrl Pts',(-2.26793442558022,0.509925141122153,
6.41775957203382));
#22726=CARTESIAN_POINT('Ctrl Pts',(-2.2631305551982,0.504673506244106,6.52034765288796));
#22727=CARTESIAN_POINT('Ctrl Pts',(-2.2543537392908,0.437620931409163,6.70175770318116));
#22728=CARTESIAN_POINT('Ctrl Pts',(-2.24243490271462,0.239731649313908,
6.87444549491937));
#22729=CARTESIAN_POINT('Ctrl Pts',(-2.23051606613844,-0.0166811816108265,
6.93131114145764));
#22730=CARTESIAN_POINT('Ctrl Pts',(-2.21859722956226,-0.269021783055123,
6.85847254173578));
#22731=CARTESIAN_POINT('Ctrl Pts',(-2.20667839298608,-0.455688500581004,
6.67371112931225));
#22732=CARTESIAN_POINT('Ctrl Pts',(-2.1947595564099,-0.53111204424701,6.42213106706975));
#22733=CARTESIAN_POINT('Ctrl Pts',(-2.18284071983372,-0.476879959029563,
6.1651483330086));
#22734=CARTESIAN_POINT('Ctrl Pts',(-2.17092188325754,-0.306231393425269,
5.96549786619889));
#22735=CARTESIAN_POINT('Ctrl Pts',(-2.15900304668136,-0.0608253588918372,
5.8719184725451));
#22736=CARTESIAN_POINT('Ctrl Pts',(-2.14708421010518,0.199429574813985,
5.90725502825896));
#22737=CARTESIAN_POINT('Ctrl Pts',(-2.135165373529,0.410999230249818,6.06288076079265));
#22738=CARTESIAN_POINT('Ctrl Pts',(-2.12572575363955,0.49909782676439,6.25131475216463));
#22739=CARTESIAN_POINT('Ctrl Pts',(-2.1202590792755,0.50988778540031,6.36808156825251));
#22740=CARTESIAN_POINT('Ctrl Pts',(-2.11876535043684,0.509867636461186,
6.39999091897678));
#22741=CARTESIAN_POINT('Origin',(-2.93123464956316,0.,6.4));
#22742=CARTESIAN_POINT('',(-2.41876535043684,0.509907683680876,6.39998700649049));
#22743=CARTESIAN_POINT('',(-2.40623464956316,0.509881639433629,6.39998778127036));
#22744=CARTESIAN_POINT('',(-2.93123464956316,0.5099,6.4));
#22745=CARTESIAN_POINT('Ctrl Pts',(-2.40623464956316,0.509881639433629,
6.39998778127036));
#22746=CARTESIAN_POINT('Ctrl Pts',(-2.40348007117693,0.50982939809256,6.45882716501453));
#22747=CARTESIAN_POINT('Ctrl Pts',(-2.39675254726532,0.484977325655459,
6.60257394605883));
#22748=CARTESIAN_POINT('Ctrl Pts',(-2.38605207782831,0.352660304885654,
6.79774427841866));
#22749=CARTESIAN_POINT('Ctrl Pts',(-2.37413324125213,0.11918571055855,6.91803915687878));
#22750=CARTESIAN_POINT('Ctrl Pts',(-2.36221440467595,-0.143384627656033,
6.91186975902934));
#22751=CARTESIAN_POINT('Ctrl Pts',(-2.35029556809977,-0.370951756306248,
6.78074216492885));
#22752=CARTESIAN_POINT('Ctrl Pts',(-2.33837673152359,-0.507961743129952,
6.55666738389136));
#22753=CARTESIAN_POINT('Ctrl Pts',(-2.32645789494741,-0.520967562726117,
6.29434679258967));
#22754=CARTESIAN_POINT('Ctrl Pts',(-2.31453905837123,-0.406794220460285,
6.05781837586191));
#22755=CARTESIAN_POINT('Ctrl Pts',(-2.30262022179505,-0.193313835397505,
5.904823705531));
#22756=CARTESIAN_POINT('Ctrl Pts',(-2.29070138521887,0.067358531017915,
5.872712004543));
#22757=CARTESIAN_POINT('Ctrl Pts',(-2.27878254864269,0.311587260629241,
5.96932241712133));
#22758=CARTESIAN_POINT('Ctrl Pts',(-2.26729363675745,0.473685134411606,
6.16379304907585));
#22759=CARTESIAN_POINT('Ctrl Pts',(-2.25977767039761,0.509870731821366,
6.32434939841728));
#22760=CARTESIAN_POINT('Ctrl Pts',(-2.25623464956316,0.509932009041494,
6.40000883270604));
#22761=CARTESIAN_POINT('Ctrl Pts',(-2.41876535043684,0.509907683680876,
6.3999870064905));
#22762=CARTESIAN_POINT('Ctrl Pts',(-2.41560977188494,0.509837930394076,
6.46738208429797));
#22763=CARTESIAN_POINT('Ctrl Pts',(-2.40848124780764,0.479478777569272,
6.61969007117178));
#22764=CARTESIAN_POINT('Ctrl Pts',(-2.39737977820495,0.332178326477852,
6.81500283186379));
#22765=CARTESIAN_POINT('Ctrl Pts',(-2.38546094162877,0.092940867251264,
6.92338493135519));
#22766=CARTESIAN_POINT('Ctrl Pts',(-2.37354210505259,-0.168985416607936,
6.90399773818908));
#22767=CARTESIAN_POINT('Ctrl Pts',(-2.36162326847641,-0.38965879870384,
6.76157407502307));
#22768=CARTESIAN_POINT('Ctrl Pts',(-2.34970443190023,-0.515208255680234,
6.5308825596382));
#22769=CARTESIAN_POINT('Ctrl Pts',(-2.33778559532405,-0.514984518987432,
6.26823985300105));
#22770=CARTESIAN_POINT('Ctrl Pts',(-2.32586675874787,-0.389042207488899,
6.03776257519368));
#22771=CARTESIAN_POINT('Ctrl Pts',(-2.31394792217169,-0.168126493747137,
5.89571508724314));
#22772=CARTESIAN_POINT('Ctrl Pts',(-2.30202908559551,0.0938324405162212,
5.87677417471489));
#22773=CARTESIAN_POINT('Ctrl Pts',(-2.29011024901934,0.332884898468083,
5.98556371357228));
#22774=CARTESIAN_POINT('Ctrl Pts',(-2.27902233729978,0.479672887909896,
6.18088831601448));
#22775=CARTESIAN_POINT('Ctrl Pts',(-2.27190737110561,0.50983726500634,6.33290718685512));
#22776=CARTESIAN_POINT('Ctrl Pts',(-2.26876535043684,0.509906762201912,
6.4000130523451));
#22777=CARTESIAN_POINT('Origin',(-2.93123464956316,0.,6.4));
#22778=CARTESIAN_POINT('',(-2.56876535043684,0.509867809550215,6.40001069114481));
#22779=CARTESIAN_POINT('',(-2.55623464956316,0.509888470297935,6.40001295625876));
#22780=CARTESIAN_POINT('',(-2.93123464956316,0.5099,6.4));
#22781=CARTESIAN_POINT('',(-2.6,0.132288496556896,5.90755938055567));
#22782=CARTESIAN_POINT('Ctrl Pts',(-2.6,0.132288496556895,5.90755938055567));
#22783=CARTESIAN_POINT('Ctrl Pts',(-2.59602705447461,0.214239653399634,
5.92957461427473));
#22784=CARTESIAN_POINT('Ctrl Pts',(-2.58808116342382,0.366850103542102,
6.0153123398751));
#22785=CARTESIAN_POINT('Ctrl Pts',(-2.57766961356943,0.488635125282487,
6.20977428615126));
#22786=CARTESIAN_POINT('Ctrl Pts',(-2.57123100924044,0.509836321405008,
6.34733983573258));
#22787=CARTESIAN_POINT('Ctrl Pts',(-2.56876535043684,0.509867809550215,
6.40001069114481));
#22788=CARTESIAN_POINT('',(-2.6,-0.132303594671782,5.90751949357016));
#22789=CARTESIAN_POINT('Origin',(-2.6,0.,6.4));
#22790=CARTESIAN_POINT('Ctrl Pts',(-2.6,-0.132303594671782,5.90751949357016));
#22791=CARTESIAN_POINT('Ctrl Pts',(-2.59622409987445,-0.0544270437755129,
5.88663631098165));
#22792=CARTESIAN_POINT('Ctrl Pts',(-2.58847525422351,0.115765473878103,
5.88226868015152));
#22793=CARTESIAN_POINT('Ctrl Pts',(-2.57675346304718,0.347023432783479,
5.99732787846002));
#22794=CARTESIAN_POINT('Ctrl Pts',(-2.56594091302711,0.483490786405975,
6.19264042843836));
#22795=CARTESIAN_POINT('Ctrl Pts',(-2.55910130853244,0.509829655724409,
6.3387818547688));
#22796=CARTESIAN_POINT('Ctrl Pts',(-2.55623464956316,0.509888470297935,
6.40001295625876));
#22797=CARTESIAN_POINT('Origin',(2.93123464956316,0.,6.4));
#22798=CARTESIAN_POINT('',(2.11876535043684,-0.509867636461186,6.39999091897679));
#22799=CARTESIAN_POINT('',(2.10623464956316,-0.509830151085518,6.39998162138192));
#22800=CARTESIAN_POINT('',(2.93123464956316,-0.5099,6.4));
#22801=CARTESIAN_POINT('',(2.1,-0.492610334572591,6.53165511107542));
#22802=CARTESIAN_POINT('Ctrl Pts',(2.10623464956316,-0.509830060291024,
6.39998159749211));
#22803=CARTESIAN_POINT('Ctrl Pts',(2.1041564330421,-0.509817985963964,6.44437440316355));
#22804=CARTESIAN_POINT('Ctrl Pts',(2.10207821652105,-0.504071192426059,
6.48877233215731));
#22805=CARTESIAN_POINT('Ctrl Pts',(2.1,-0.492610334572592,6.53165511107541));
#22806=CARTESIAN_POINT('',(2.1,-0.360348823959177,6.76081852140067));
#22807=CARTESIAN_POINT('Origin',(2.1,0.,6.4));
#22808=CARTESIAN_POINT('Ctrl Pts',(2.11876535043684,-0.509867636461186,
6.39999091897678));
#22809=CARTESIAN_POINT('Ctrl Pts',(2.11628613375011,-0.509834194256146,
6.45295246911284));
#22810=CARTESIAN_POINT('Ctrl Pts',(2.11003101693783,-0.489118231027634,
6.58660111045784));
#22811=CARTESIAN_POINT('Ctrl Pts',(2.10377590012555,-0.417372467378852,
6.70381704168278));
#22812=CARTESIAN_POINT('Ctrl Pts',(2.1,-0.360348823959177,6.76081852140067));
#22813=CARTESIAN_POINT('Origin',(2.93123464956316,0.,6.4));
#22814=CARTESIAN_POINT('',(2.26876535043684,-0.509906762201912,6.4000130523451));
#22815=CARTESIAN_POINT('',(2.25623464956316,-0.509932009041494,6.40000883270604));
#22816=CARTESIAN_POINT('',(2.93123464956316,-0.5099,6.4));
#22817=CARTESIAN_POINT('Ctrl Pts',(2.25623464956316,-0.509932009041494,
6.40000883270604));
#22818=CARTESIAN_POINT('Ctrl Pts',(2.25580472487222,-0.509939444670906,
6.40918965901876));
#22819=CARTESIAN_POINT('Ctrl Pts',(2.25140185465588,-0.507452628870696,
6.50320671872761));
#22820=CARTESIAN_POINT('Ctrl Pts',(2.24302603891415,-0.45226492573298,6.67933176541862));
#22821=CARTESIAN_POINT('Ctrl Pts',(2.23110720233797,-0.263325094846747,
6.86176802153349));
#22822=CARTESIAN_POINT('Ctrl Pts',(2.2191883657618,-0.0101020467317839,
6.93147693256131));
#22823=CARTESIAN_POINT('Ctrl Pts',(2.20726952918561,0.245587098572064,6.87144120673232));
#22824=CARTESIAN_POINT('Ctrl Pts',(2.19535069260943,0.441323311848774,6.69631656607358));
#22825=CARTESIAN_POINT('Ctrl Pts',(2.18343185603326,0.529323086465549,6.44885519432254));
#22826=CARTESIAN_POINT('Ctrl Pts',(2.17151301945708,0.488104195118536,6.18946640393034));
#22827=CARTESIAN_POINT('Ctrl Pts',(2.1595941828809,0.327728249264285,5.98147509599461));
#22828=CARTESIAN_POINT('Ctrl Pts',(2.14767534630472,0.0873481558956701,
5.87565064933844));
#22829=CARTESIAN_POINT('Ctrl Pts',(2.13575650972854,-0.174357740366956,
5.89783918404992));
#22830=CARTESIAN_POINT('Ctrl Pts',(2.12383767315236,-0.393492635182685,
6.04259742479108));
#22831=CARTESIAN_POINT('Ctrl Pts',(2.11399705309723,-0.495113210733723,
6.23418199944647));
#22832=CARTESIAN_POINT('Ctrl Pts',(2.1081293785675,-0.509841068565406,6.35950827065745));
#22833=CARTESIAN_POINT('Ctrl Pts',(2.10623464956316,-0.509830060291024,
6.39998159749211));
#22834=CARTESIAN_POINT('Ctrl Pts',(2.26876535043684,-0.509906762201912,
6.4000130523451));
#22835=CARTESIAN_POINT('Ctrl Pts',(2.26793442558022,-0.509925141122153,
6.41775957203382));
#22836=CARTESIAN_POINT('Ctrl Pts',(2.2631305551982,-0.504673506244106,6.52034765288796));
#22837=CARTESIAN_POINT('Ctrl Pts',(2.2543537392908,-0.437620931409163,6.70175770318116));
#22838=CARTESIAN_POINT('Ctrl Pts',(2.24243490271462,-0.239731649313908,
6.87444549491937));
#22839=CARTESIAN_POINT('Ctrl Pts',(2.23051606613844,0.0166811816108265,
6.93131114145764));
#22840=CARTESIAN_POINT('Ctrl Pts',(2.21859722956226,0.269021783055123,6.85847254173578));
#22841=CARTESIAN_POINT('Ctrl Pts',(2.20667839298608,0.455688500581004,6.67371112931225));
#22842=CARTESIAN_POINT('Ctrl Pts',(2.1947595564099,0.53111204424701,6.42213106706975));
#22843=CARTESIAN_POINT('Ctrl Pts',(2.18284071983372,0.476879959029563,6.1651483330086));
#22844=CARTESIAN_POINT('Ctrl Pts',(2.17092188325754,0.306231393425269,5.96549786619889));
#22845=CARTESIAN_POINT('Ctrl Pts',(2.15900304668136,0.0608253588918372,
5.8719184725451));
#22846=CARTESIAN_POINT('Ctrl Pts',(2.14708421010518,-0.199429574813985,
5.90725502825896));
#22847=CARTESIAN_POINT('Ctrl Pts',(2.135165373529,-0.410999230249818,6.06288076079265));
#22848=CARTESIAN_POINT('Ctrl Pts',(2.12572575363955,-0.49909782676439,6.25131475216463));
#22849=CARTESIAN_POINT('Ctrl Pts',(2.1202590792755,-0.50988778540031,6.36808156825251));
#22850=CARTESIAN_POINT('Ctrl Pts',(2.11876535043684,-0.509867636461186,
6.39999091897678));
#22851=CARTESIAN_POINT('Origin',(2.93123464956316,0.,6.4));
#22852=CARTESIAN_POINT('',(2.41876535043684,-0.509907683680876,6.39998700649049));
#22853=CARTESIAN_POINT('',(2.40623464956316,-0.509881639433629,6.39998778127036));
#22854=CARTESIAN_POINT('',(2.93123464956316,-0.5099,6.4));
#22855=CARTESIAN_POINT('Ctrl Pts',(2.40623464956316,-0.509881639433629,
6.39998778127036));
#22856=CARTESIAN_POINT('Ctrl Pts',(2.40348007117693,-0.50982939809256,6.45882716501453));
#22857=CARTESIAN_POINT('Ctrl Pts',(2.39675254726532,-0.484977325655459,
6.60257394605883));
#22858=CARTESIAN_POINT('Ctrl Pts',(2.38605207782831,-0.352660304885654,
6.79774427841866));
#22859=CARTESIAN_POINT('Ctrl Pts',(2.37413324125213,-0.11918571055855,6.91803915687878));
#22860=CARTESIAN_POINT('Ctrl Pts',(2.36221440467595,0.143384627656033,6.91186975902934));
#22861=CARTESIAN_POINT('Ctrl Pts',(2.35029556809977,0.370951756306248,6.78074216492885));
#22862=CARTESIAN_POINT('Ctrl Pts',(2.33837673152359,0.507961743129952,6.55666738389136));
#22863=CARTESIAN_POINT('Ctrl Pts',(2.32645789494741,0.520967562726117,6.29434679258967));
#22864=CARTESIAN_POINT('Ctrl Pts',(2.31453905837123,0.406794220460285,6.05781837586191));
#22865=CARTESIAN_POINT('Ctrl Pts',(2.30262022179505,0.193313835397505,5.904823705531));
#22866=CARTESIAN_POINT('Ctrl Pts',(2.29070138521887,-0.067358531017915,
5.872712004543));
#22867=CARTESIAN_POINT('Ctrl Pts',(2.27878254864269,-0.311587260629241,
5.96932241712133));
#22868=CARTESIAN_POINT('Ctrl Pts',(2.26729363675745,-0.473685134411606,
6.16379304907585));
#22869=CARTESIAN_POINT('Ctrl Pts',(2.25977767039761,-0.509870731821366,
6.32434939841728));
#22870=CARTESIAN_POINT('Ctrl Pts',(2.25623464956316,-0.509932009041494,
6.40000883270604));
#22871=CARTESIAN_POINT('Ctrl Pts',(2.41876535043684,-0.509907683680876,
6.3999870064905));
#22872=CARTESIAN_POINT('Ctrl Pts',(2.41560977188494,-0.509837930394076,
6.46738208429797));
#22873=CARTESIAN_POINT('Ctrl Pts',(2.40848124780764,-0.479478777569272,
6.61969007117178));
#22874=CARTESIAN_POINT('Ctrl Pts',(2.39737977820495,-0.332178326477852,
6.81500283186379));
#22875=CARTESIAN_POINT('Ctrl Pts',(2.38546094162877,-0.092940867251264,
6.92338493135519));
#22876=CARTESIAN_POINT('Ctrl Pts',(2.37354210505259,0.168985416607936,6.90399773818908));
#22877=CARTESIAN_POINT('Ctrl Pts',(2.36162326847641,0.38965879870384,6.76157407502307));
#22878=CARTESIAN_POINT('Ctrl Pts',(2.34970443190023,0.515208255680234,6.5308825596382));
#22879=CARTESIAN_POINT('Ctrl Pts',(2.33778559532405,0.514984518987432,6.26823985300105));
#22880=CARTESIAN_POINT('Ctrl Pts',(2.32586675874787,0.389042207488899,6.03776257519368));
#22881=CARTESIAN_POINT('Ctrl Pts',(2.31394792217169,0.168126493747137,5.89571508724314));
#22882=CARTESIAN_POINT('Ctrl Pts',(2.30202908559551,-0.0938324405162212,
5.87677417471489));
#22883=CARTESIAN_POINT('Ctrl Pts',(2.29011024901934,-0.332884898468083,
5.98556371357228));
#22884=CARTESIAN_POINT('Ctrl Pts',(2.27902233729978,-0.479672887909896,
6.18088831601448));
#22885=CARTESIAN_POINT('Ctrl Pts',(2.27190737110561,-0.50983726500634,6.33290718685512));
#22886=CARTESIAN_POINT('Ctrl Pts',(2.26876535043684,-0.509906762201912,
6.4000130523451));
#22887=CARTESIAN_POINT('Origin',(2.93123464956316,0.,6.4));
#22888=CARTESIAN_POINT('',(2.56876535043684,-0.509867809550215,6.40001069114481));
#22889=CARTESIAN_POINT('',(2.55623464956316,-0.509888470297935,6.40001295625876));
#22890=CARTESIAN_POINT('',(2.93123464956316,-0.5099,6.4));
#22891=CARTESIAN_POINT('',(2.6,-0.132288496556896,5.90755938055567));
#22892=CARTESIAN_POINT('Ctrl Pts',(2.6,-0.132288496556895,5.90755938055567));
#22893=CARTESIAN_POINT('Ctrl Pts',(2.59602705447461,-0.214239653399634,
5.92957461427473));
#22894=CARTESIAN_POINT('Ctrl Pts',(2.58808116342382,-0.366850103542102,
6.0153123398751));
#22895=CARTESIAN_POINT('Ctrl Pts',(2.57766961356943,-0.488635125282487,
6.20977428615126));
#22896=CARTESIAN_POINT('Ctrl Pts',(2.57123100924044,-0.509836321405008,
6.34733983573258));
#22897=CARTESIAN_POINT('Ctrl Pts',(2.56876535043684,-0.509867809550215,
6.40001069114481));
#22898=CARTESIAN_POINT('',(2.6,0.132303594671782,5.90751949357016));
#22899=CARTESIAN_POINT('Origin',(2.6,0.,6.4));
#22900=CARTESIAN_POINT('Ctrl Pts',(2.6,0.132303594671782,5.90751949357016));
#22901=CARTESIAN_POINT('Ctrl Pts',(2.59622409987445,0.0544270437755129,
5.88663631098165));
#22902=CARTESIAN_POINT('Ctrl Pts',(2.58847525422351,-0.115765473878103,
5.88226868015152));
#22903=CARTESIAN_POINT('Ctrl Pts',(2.57675346304718,-0.347023432783479,
5.99732787846002));
#22904=CARTESIAN_POINT('Ctrl Pts',(2.56594091302711,-0.483490786405975,
6.19264042843836));
#22905=CARTESIAN_POINT('Ctrl Pts',(2.55910130853244,-0.509829655724409,
6.3387818547688));
#22906=CARTESIAN_POINT('Ctrl Pts',(2.55623464956316,-0.509888470297935,
6.40001295625876));
#22907=CARTESIAN_POINT('Origin',(2.,-0.574456264653803,6.8));
#22908=CARTESIAN_POINT('',(2.,0.574456264653803,6.8));
#22909=CARTESIAN_POINT('',(2.,0.360555127546398,7.));
#22910=CARTESIAN_POINT('Origin',(2.,0.,6.4));
#22911=CARTESIAN_POINT('',(2.,0.574456264653803,7.));
#22912=CARTESIAN_POINT('',(2.,0.574456264653803,6.8));
#22913=CARTESIAN_POINT('',(2.,0.,7.));
#22914=CARTESIAN_POINT('Origin',(-2.,0.574456264653803,6.8));
#22915=CARTESIAN_POINT('',(-2.,0.574456264653803,6.8));
#22916=CARTESIAN_POINT('',(-2.,0.360555127546398,7.));
#22917=CARTESIAN_POINT('Origin',(-2.,0.,6.4));
#22918=CARTESIAN_POINT('',(-2.,0.574456264653803,7.));
#22919=CARTESIAN_POINT('',(-2.,0.574456264653803,7.));
#22920=CARTESIAN_POINT('',(-2.,0.574456264653803,6.8));
#22921=CARTESIAN_POINT('Origin',(2.33023603954621,-0.574456264653802,6.8));
#22922=CARTESIAN_POINT('',(2.33023603954621,-0.574456264653803,6.8));
#22923=CARTESIAN_POINT('',(2.,-0.574456264653803,6.8));
#22924=CARTESIAN_POINT('',(2.,-0.574456264653803,6.8));
#22925=CARTESIAN_POINT('',(2.,-0.574456264653803,7.));
#22926=CARTESIAN_POINT('',(2.,-0.574456264653803,6.8));
#22927=CARTESIAN_POINT('',(2.33023603954621,-0.574456264653802,7.));
#22928=CARTESIAN_POINT('',(2.33023603954621,-0.574456264653802,7.));
#22929=CARTESIAN_POINT('',(2.33023603954621,-0.574456264653802,6.8));
#22930=CARTESIAN_POINT('Origin',(-2.,-0.574456264653803,6.8));
#22931=CARTESIAN_POINT('',(-2.,-0.574456264653803,6.8));
#22932=CARTESIAN_POINT('',(-2.33023603954621,-0.574456264653803,6.8));
#22933=CARTESIAN_POINT('',(-2.,-0.574456264653803,6.8));
#22934=CARTESIAN_POINT('',(-2.33023603954621,-0.574456264653803,7.));
#22935=CARTESIAN_POINT('',(-2.33023603954621,-0.574456264653803,6.8));
#22936=CARTESIAN_POINT('',(-2.,-0.574456264653803,7.));
#22937=CARTESIAN_POINT('',(-2.,-0.574456264653803,7.));
#22938=CARTESIAN_POINT('',(-2.,-0.574456264653803,6.8));
#22939=CARTESIAN_POINT('Origin',(-2.,0.574456264653803,6.8));
#22940=CARTESIAN_POINT('',(-2.,-0.360555127546398,7.));
#22941=CARTESIAN_POINT('Origin',(-2.,0.,6.4));
#22942=CARTESIAN_POINT('',(-2.,0.574456264653803,7.));
#22943=CARTESIAN_POINT('Origin',(-2.33023603954621,0.574456264653802,6.8));
#22944=CARTESIAN_POINT('',(-2.33023603954621,0.574456264653803,6.8));
#22945=CARTESIAN_POINT('',(-2.,0.574456264653803,6.8));
#22946=CARTESIAN_POINT('',(-2.33023603954621,0.574456264653802,7.));
#22947=CARTESIAN_POINT('',(-2.33023603954621,0.574456264653802,7.));
#22948=CARTESIAN_POINT('',(-2.33023603954621,0.574456264653802,6.8));
#22949=CARTESIAN_POINT('Origin',(2.,0.574456264653803,6.8));
#22950=CARTESIAN_POINT('',(2.33023603954621,0.574456264653803,6.8));
#22951=CARTESIAN_POINT('',(2.,0.574456264653803,6.8));
#22952=CARTESIAN_POINT('',(2.33023603954621,0.574456264653803,7.));
#22953=CARTESIAN_POINT('',(2.33023603954621,0.574456264653803,6.8));
#22954=CARTESIAN_POINT('',(2.,0.574456264653803,7.));
#22955=CARTESIAN_POINT('Origin',(2.,-0.574456264653803,6.8));
#22956=CARTESIAN_POINT('',(2.,-0.360555127546398,7.));
#22957=CARTESIAN_POINT('Origin',(2.,0.,6.4));
#22958=CARTESIAN_POINT('',(2.,0.,7.));
#22959=CARTESIAN_POINT('Origin',(0.,0.,7.));
#22960=CARTESIAN_POINT('',(2.,0.,7.));
#22961=CARTESIAN_POINT('Origin',(0.,0.,7.));
#22962=CARTESIAN_POINT('',(-2.,0.,7.));
#22963=CARTESIAN_POINT('Origin',(0.,0.,7.));
#22964=CARTESIAN_POINT('',(-0.6,7.34788079488412E-17,7.));
#22965=CARTESIAN_POINT('Origin',(0.,0.,7.));
#22966=CARTESIAN_POINT('Origin',(-2.,0.,6.4));
#22967=CARTESIAN_POINT('Origin',(-2.,0.,6.4));
#22968=CARTESIAN_POINT('Origin',(2.93123464956316,0.,6.4));
#22969=CARTESIAN_POINT('Ctrl Pts',(2.55623464956316,-0.509888470297935,
6.40001295625876));
#22970=CARTESIAN_POINT('Ctrl Pts',(2.55512836300704,-0.509911167721204,
6.42364295379955));
#22971=CARTESIAN_POINT('Ctrl Pts',(2.55004913092554,-0.502507177574701,
6.53211994282295));
#22972=CARTESIAN_POINT('Ctrl Pts',(2.54099695331864,-0.426919346618493,
6.7167170754366));
#22973=CARTESIAN_POINT('Ctrl Pts',(2.52907811674246,-0.223174193283009,
6.88245524211623));
#22974=CARTESIAN_POINT('Ctrl Pts',(2.51715928016628,0.0350524704178637,
6.93041600240246));
#22975=CARTESIAN_POINT('Ctrl Pts',(2.5052404435901,0.284722093726431,6.84889099741939));
#22976=CARTESIAN_POINT('Ctrl Pts',(2.49332160701392,0.464885050226796,6.6577822578485));
#22977=CARTESIAN_POINT('Ctrl Pts',(2.48140277043774,0.531559769507257,6.40374342750432));
#22978=CARTESIAN_POINT('Ctrl Pts',(2.46948393386156,0.468469545343797,6.14879075163119));
#22979=CARTESIAN_POINT('Ctrl Pts',(2.45756509728538,0.291016032073294,5.95516354586177));
#22980=CARTESIAN_POINT('Ctrl Pts',(2.4456462607092,0.0425193718295788,5.87013029471448));
#22981=CARTESIAN_POINT('Ctrl Pts',(2.43372742413302,-0.216357163144678,
5.91444940567057));
#22982=CARTESIAN_POINT('Ctrl Pts',(2.42180858755684,-0.422416354717456,
6.07730165027367));
#22983=CARTESIAN_POINT('Ctrl Pts',(2.41264432936689,-0.501564565860727,
6.26308799447805));
#22984=CARTESIAN_POINT('Ctrl Pts',(2.40745301670233,-0.50990474610345,6.37396275616984));
#22985=CARTESIAN_POINT('Ctrl Pts',(2.40623464956316,-0.509881639433629,
6.39998778127036));
#22986=CARTESIAN_POINT('Ctrl Pts',(2.56876535043684,-0.509867809550215,
6.40001069114481));
#22987=CARTESIAN_POINT('Ctrl Pts',(2.56725806371505,-0.509887058630054,
6.4322090151272));
#22988=CARTESIAN_POINT('Ctrl Pts',(2.56177783146786,-0.498968432159698,
6.54926324266892));
#22989=CARTESIAN_POINT('Ctrl Pts',(2.55232465369528,-0.410425773087965,
6.73782039475945));
#22990=CARTESIAN_POINT('Ctrl Pts',(2.54040581711911,-0.19858907062663,6.89308342832313));
#22991=CARTESIAN_POINT('Ctrl Pts',(2.52848698054292,0.0617246536500735,
6.92797742227401));
#22992=CARTESIAN_POINT('Ctrl Pts',(2.51656814396674,0.306971377021502,6.8339796336226));
#22993=CARTESIAN_POINT('Ctrl Pts',(2.50464930739056,0.477279320739804,6.63403891232169));
#22994=CARTESIAN_POINT('Ctrl Pts',(2.49273047081439,0.531073600862929,6.3769640630774));
#22995=CARTESIAN_POINT('Ctrl Pts',(2.48081163423821,0.455221493256117,6.12551290982166));
#22996=CARTESIAN_POINT('Ctrl Pts',(2.46889279766203,0.268240284898955,5.94106977614238));
#22997=CARTESIAN_POINT('Ctrl Pts',(2.45697396108585,0.0157759417689948,
5.86866121228054));
#22998=CARTESIAN_POINT('Ctrl Pts',(2.44505512450967,-0.240539628301038,
5.92596363104932));
#22999=CARTESIAN_POINT('Ctrl Pts',(2.43313628793349,-0.438134411540293,
6.09898832463164));
#23000=CARTESIAN_POINT('Ctrl Pts',(2.42437302990921,-0.504774712912163,
6.28023194354175));
#23001=CARTESIAN_POINT('Ctrl Pts',(2.41958271741033,-0.509925751376541,
6.3825301408573));
#23002=CARTESIAN_POINT('Ctrl Pts',(2.41876535043684,-0.509907683680876,
6.3999870064905));
#23003=CARTESIAN_POINT('Ctrl Pts',(2.6,0.322335278395778,6.67898325810255));
#23004=CARTESIAN_POINT('Ctrl Pts',(2.59602705447461,0.368763212726337,6.62534075195518));
#23005=CARTESIAN_POINT('Ctrl Pts',(2.58808116342382,0.434258099467944,6.4944682619995));
#23006=CARTESIAN_POINT('Ctrl Pts',(2.57616232684764,0.426482264300449,6.27500430516079));
#23007=CARTESIAN_POINT('Ctrl Pts',(2.56424349027146,0.314584469477882,6.08608472387891));
#23008=CARTESIAN_POINT('Ctrl Pts',(2.55232465369528,0.125891708691813,5.97378227942249));
#23009=CARTESIAN_POINT('Ctrl Pts',(2.5404058171191,-0.0935351747046863,
5.96553560214966));
#23010=CARTESIAN_POINT('Ctrl Pts',(2.52848698054292,-0.290127651295543,
6.06334746928321));
#23011=CARTESIAN_POINT('Ctrl Pts',(2.51656814396674,-0.415894108139653,
6.24334485866553));
#23012=CARTESIAN_POINT('Ctrl Pts',(2.50464930739057,-0.440131934448267,
6.46158434769009));
#23013=CARTESIAN_POINT('Ctrl Pts',(2.49273047081439,-0.356924333130935,
6.66479013386668));
#23014=CARTESIAN_POINT('Ctrl Pts',(2.48081163423821,-0.186583954886344,
6.80335491216739));
#23015=CARTESIAN_POINT('Ctrl Pts',(2.46889279766203,0.0293054876233287,
6.8434523275626));
#23016=CARTESIAN_POINT('Ctrl Pts',(2.45697396108585,0.238040848314528,6.77529365012726));
#23017=CARTESIAN_POINT('Ctrl Pts',(2.44505512450967,0.388665418536347,6.61551789864839));
#23018=CARTESIAN_POINT('Ctrl Pts',(2.43313628793349,0.444408569799851,6.40312967865285));
#23019=CARTESIAN_POINT('Ctrl Pts',(2.42121745135731,0.391662222357444,6.18997744149907));
#23020=CARTESIAN_POINT('Ctrl Pts',(2.40929861478113,0.243302872078535,6.0280961357146));
#23021=CARTESIAN_POINT('Ctrl Pts',(2.39737977820495,0.0355481627984888,
5.95700440211175));
#23022=CARTESIAN_POINT('Ctrl Pts',(2.38546094162877,-0.180884602174105,
5.99405723011839));
#23023=CARTESIAN_POINT('Ctrl Pts',(2.37354210505259,-0.353159623487059,
6.13020924399229));
#23024=CARTESIAN_POINT('Ctrl Pts',(2.36162326847641,-0.439220937561425,
6.33222286740014));
#23025=CARTESIAN_POINT('Ctrl Pts',(2.34970443190023,-0.418059163834771,
6.55078231736932));
#23026=CARTESIAN_POINT('Ctrl Pts',(2.33778559532405,-0.29484033726761,6.73253262578912));
#23027=CARTESIAN_POINT('Ctrl Pts',(2.32586675874787,-0.099644770368915,
6.83310471186003));
#23028=CARTESIAN_POINT('Ctrl Pts',(2.3139479221717,0.119876185075048,6.82794680971604));
#23029=CARTESIAN_POINT('Ctrl Pts',(2.30202908559551,0.310132837249173,6.71831807199288));
#23030=CARTESIAN_POINT('Ctrl Pts',(2.29011024901934,0.424679527547163,6.53098118406136));
#23031=CARTESIAN_POINT('Ctrl Pts',(2.27819141244315,0.435552994685514,6.31166902859576));
#23032=CARTESIAN_POINT('Ctrl Pts',(2.26627257586698,0.340098796199685,6.11392032482827));
#23033=CARTESIAN_POINT('Ctrl Pts',(2.2543537392908,0.16161931364965,5.98600969928979));
#23034=CARTESIAN_POINT('Ctrl Pts',(2.24243490271462,-0.0563148495252739,
5.95916283101918));
#23035=CARTESIAN_POINT('Ctrl Pts',(2.23051606613844,-0.260501371261513,
6.03993360741091));
#23036=CARTESIAN_POINT('Ctrl Pts',(2.21859722956226,-0.401094017530737,
6.20860417742001));
#23037=CARTESIAN_POINT('Ctrl Pts',(2.20667839298608,-0.44377116171621,6.42399850480546));
#23038=CARTESIAN_POINT('Ctrl Pts',(2.1947595564099,-0.378114410354912,6.63353428436548));
#23039=CARTESIAN_POINT('Ctrl Pts',(2.18284071983372,-0.220151966921295,
6.78605943828148));
#23040=CARTESIAN_POINT('Ctrl Pts',(2.17092188325754,-0.00844577862671016,
6.84433931427905));
#23041=CARTESIAN_POINT('Ctrl Pts',(2.15900304668136,0.205322181057602,6.79414666881739));
#23042=CARTESIAN_POINT('Ctrl Pts',(2.14708421010518,0.368966714730599,6.64773436383049));
#23043=CARTESIAN_POINT('Ctrl Pts',(2.135165373529,0.442538599255273,6.44084520364718));
#23044=CARTESIAN_POINT('Ctrl Pts',(2.12324653695282,0.408077698331108,6.22398416943617));
#23045=CARTESIAN_POINT('Ctrl Pts',(2.11132770037664,0.273995984823229,6.05009380941852));
#23046=CARTESIAN_POINT('Ctrl Pts',(2.09940886380046,0.0730271011145798,
5.96161967407919));
#23047=CARTESIAN_POINT('Ctrl Pts',(2.08749002722429,-0.145771140848075,
5.98017031606292));
#23048=CARTESIAN_POINT('Ctrl Pts',(2.07557119064811,-0.328978055262558,
6.10119490525287));
#23049=CARTESIAN_POINT('Ctrl Pts',(2.06365235407193,-0.431879950098104,
6.29519514237415));
#23050=CARTESIAN_POINT('Ctrl Pts',(2.05570646302114,-0.430162668703658,
6.44153119316515));
#23051=CARTESIAN_POINT('Ctrl Pts',(2.05173351749575,-0.411845039474987,
6.51006976632957));
#23052=CARTESIAN_POINT('Ctrl Pts',(2.61608882750142,0.34340590883904,6.69722002436839));
#23053=CARTESIAN_POINT('Ctrl Pts',(2.61211588197602,0.392868775775771,6.64007097860578));
#23054=CARTESIAN_POINT('Ctrl Pts',(2.60416999092524,0.462644976561947,6.5006435272299));
#23055=CARTESIAN_POINT('Ctrl Pts',(2.59225115434906,0.454360845343155,6.26683350205768));
#23056=CARTESIAN_POINT('Ctrl Pts',(2.58033231777288,0.335148439802654,6.065564497838));
#23057=CARTESIAN_POINT('Ctrl Pts',(2.5684134811967,0.134121083034322,5.94592099125275));
#23058=CARTESIAN_POINT('Ctrl Pts',(2.55649464462052,-0.0996494452538391,
5.9371352396035));
#23059=CARTESIAN_POINT('Ctrl Pts',(2.54457580804434,-0.309092911791522,
6.04134093900881));
#23060=CARTESIAN_POINT('Ctrl Pts',(2.53265697146816,-0.443080555430665,
6.23310451945562));
#23061=CARTESIAN_POINT('Ctrl Pts',(2.52073813489198,-0.468902776359187,
6.46561003497361));
#23062=CARTESIAN_POINT('Ctrl Pts',(2.5088192983158,-0.380256004293454,6.68209911438999));
#23063=CARTESIAN_POINT('Ctrl Pts',(2.49690046173962,-0.198780701018566,
6.829721688817));
#23064=CARTESIAN_POINT('Ctrl Pts',(2.48498162516344,0.0312211485548406,
6.87244021917589));
#23065=CARTESIAN_POINT('Ctrl Pts',(2.47306278858727,0.253601263451829,6.79982609922463));
#23066=CARTESIAN_POINT('Ctrl Pts',(2.46114395201108,0.414071962433164,6.62960601838176));
#23067=CARTESIAN_POINT('Ctrl Pts',(2.44922511543491,0.473458969702319,6.40333426160334));
#23068=CARTESIAN_POINT('Ctrl Pts',(2.43730627885873,0.417264663352895,6.17624854487645));
#23069=CARTESIAN_POINT('Ctrl Pts',(2.42538744228255,0.259207258743454,6.00378527243032));
#23070=CARTESIAN_POINT('Ctrl Pts',(2.41346860570637,0.0378718991421855,
5.92804636631267));
#23071=CARTESIAN_POINT('Ctrl Pts',(2.40154976913019,-0.192708789164296,
5.96752128863578));
#23072=CARTESIAN_POINT('Ctrl Pts',(2.38963093255401,-0.376245200563858,
6.11257337941941));
#23073=CARTESIAN_POINT('Ctrl Pts',(2.37771209597783,-0.467932228811824,
6.32779236596503));
#23074=CARTESIAN_POINT('Ctrl Pts',(2.36579325940165,-0.445387137950485,
6.56063875785105));
#23075=CARTESIAN_POINT('Ctrl Pts',(2.35387442282547,-0.314113659806958,
6.75426984333229));
#23076=CARTESIAN_POINT('Ctrl Pts',(2.34195558624929,-0.106158417098793,
6.86141619353295));
#23077=CARTESIAN_POINT('Ctrl Pts',(2.33003674967311,0.127712332602043,6.85592112615381));
#23078=CARTESIAN_POINT('Ctrl Pts',(2.31811791309693,0.330405810268198,6.73912610297154));
#23079=CARTESIAN_POINT('Ctrl Pts',(2.30619907652075,0.452440266074759,6.53954325067136));
#23080=CARTESIAN_POINT('Ctrl Pts',(2.29428023994457,0.464024517365714,6.30589494992706));
#23081=CARTESIAN_POINT('Ctrl Pts',(2.28236140336839,0.362330604286552,6.09521967517282));
#23082=CARTESIAN_POINT('Ctrl Pts',(2.27044256679221,0.172184154232268,5.95894770137019));
#23083=CARTESIAN_POINT('Ctrl Pts',(2.25852373021603,-0.0599960766894875,
5.93034588886046));
#23084=CARTESIAN_POINT('Ctrl Pts',(2.24660489363985,-0.277530001050755,
6.01639654398105));
#23085=CARTESIAN_POINT('Ctrl Pts',(2.23468605706368,-0.427313002490913,
6.19609288586657));
#23086=CARTESIAN_POINT('Ctrl Pts',(2.2227672204875,-0.472779895096048,6.42556725529552));
#23087=CARTESIAN_POINT('Ctrl Pts',(2.21084838391132,-0.402831248814268,
6.64880011138319));
#23088=CARTESIAN_POINT('Ctrl Pts',(2.19892954733514,-0.234543009563112,
6.81129563269882));
#23089=CARTESIAN_POINT('Ctrl Pts',(2.18701071075896,-0.00899786799506803,
6.8733851870398));
#23090=CARTESIAN_POINT('Ctrl Pts',(2.17509187418278,0.218743820229089,6.81991151478903));
#23091=CARTESIAN_POINT('Ctrl Pts',(2.1631730376066,0.393085580436657,6.66392843124485));
#23092=CARTESIAN_POINT('Ctrl Pts',(2.15125420103042,0.471466761658698,6.44351520053897));
#23093=CARTESIAN_POINT('Ctrl Pts',(2.13933536445424,0.43475319726025,6.2124782476009));
#23094=CARTESIAN_POINT('Ctrl Pts',(2.12741652787806,0.291906739636914,6.02722090494389));
#23095=CARTESIAN_POINT('Ctrl Pts',(2.11549769130188,0.0778007860416099,
5.93296333249894));
#23096=CARTESIAN_POINT('Ctrl Pts',(2.1035788547257,-0.155300007354369,5.95272660539192));
#23097=CARTESIAN_POINT('Ctrl Pts',(2.09166001814952,-0.350482915235934,
6.08166241176561));
#23098=CARTESIAN_POINT('Ctrl Pts',(2.07974118157334,-0.46011137071598,6.28834418757117));
#23099=CARTESIAN_POINT('Ctrl Pts',(2.07179529052256,-0.458281832910106,
6.44424603228361));
#23100=CARTESIAN_POINT('Ctrl Pts',(2.06782234499716,-0.438766804507522,
6.51726488124485));
#23101=CARTESIAN_POINT('Ctrl Pts',(2.63217765500284,0.364476539282301,6.71545679063422));
#23102=CARTESIAN_POINT('Ctrl Pts',(2.62820470947744,0.416974338825206,6.65480120525638));
#23103=CARTESIAN_POINT('Ctrl Pts',(2.62025881842666,0.49103185365595,6.5068187924603));
#23104=CARTESIAN_POINT('Ctrl Pts',(2.60833998185048,0.482239426385862,6.25866269895458));
#23105=CARTESIAN_POINT('Ctrl Pts',(2.5964211452743,0.355712410127426,6.04504427179708));
#23106=CARTESIAN_POINT('Ctrl Pts',(2.58450230869812,0.142350457376832,5.91805970308301));
#23107=CARTESIAN_POINT('Ctrl Pts',(2.57258347212194,-0.105763715802992,
5.90873487705734));
#23108=CARTESIAN_POINT('Ctrl Pts',(2.56066463554576,-0.3280581722875,6.01933440873442));
#23109=CARTESIAN_POINT('Ctrl Pts',(2.54874579896958,-0.470267002721677,
6.2228641802457));
#23110=CARTESIAN_POINT('Ctrl Pts',(2.5368269623934,-0.497673618270107,6.46963572225713));
#23111=CARTESIAN_POINT('Ctrl Pts',(2.52490812581722,-0.403587675455974,
6.69940809491329));
#23112=CARTESIAN_POINT('Ctrl Pts',(2.51298928924104,-0.210977447150787,
6.85608846546662));
#23113=CARTESIAN_POINT('Ctrl Pts',(2.50107045266486,0.0331368094863519,
6.90142811078917));
#23114=CARTESIAN_POINT('Ctrl Pts',(2.48915161608868,0.26916167858913,6.82435854832202));
#23115=CARTESIAN_POINT('Ctrl Pts',(2.4772327795125,0.43947850632998,6.64369413811513));
#23116=CARTESIAN_POINT('Ctrl Pts',(2.46531394293632,0.502509369604788,6.40353884455383));
#23117=CARTESIAN_POINT('Ctrl Pts',(2.45339510636014,0.442867104348346,6.16251964825382));
#23118=CARTESIAN_POINT('Ctrl Pts',(2.44147626978397,0.275111645408374,5.97947440914605));
#23119=CARTESIAN_POINT('Ctrl Pts',(2.42955743320778,0.0401956354858822,
5.89908833051357));
#23120=CARTESIAN_POINT('Ctrl Pts',(2.41763859663161,-0.204532976154487,
5.94098534715318));
#23121=CARTESIAN_POINT('Ctrl Pts',(2.40571976005543,-0.399330777640657,
6.09493751484654));
#23122=CARTESIAN_POINT('Ctrl Pts',(2.39380092347925,-0.496643520062223,
6.32336186452993));
#23123=CARTESIAN_POINT('Ctrl Pts',(2.38188208690307,-0.472715112066199,
6.57049519833277));
#23124=CARTESIAN_POINT('Ctrl Pts',(2.36996325032689,-0.333386982346306,
6.77600706087547));
#23125=CARTESIAN_POINT('Ctrl Pts',(2.35804441375071,-0.112672063828671,
6.88972767520587));
#23126=CARTESIAN_POINT('Ctrl Pts',(2.34612557717453,0.135548480129038,6.88389544259157));
#23127=CARTESIAN_POINT('Ctrl Pts',(2.33420674059835,0.350678783287223,6.7599341339502));
#23128=CARTESIAN_POINT('Ctrl Pts',(2.32228790402217,0.480201004602356,6.54810531728136));
#23129=CARTESIAN_POINT('Ctrl Pts',(2.31036906744599,0.492496040045916,6.30012087125837));
#23130=CARTESIAN_POINT('Ctrl Pts',(2.29845023086981,0.384562412373419,6.07651902551736));
#23131=CARTESIAN_POINT('Ctrl Pts',(2.28653139429363,0.182748994814887,5.9318857034506));
#23132=CARTESIAN_POINT('Ctrl Pts',(2.27461255771745,-0.0636773038537012,
5.90152894670173));
#23133=CARTESIAN_POINT('Ctrl Pts',(2.26269372114127,-0.294558630839998,
5.99285948055119));
#23134=CARTESIAN_POINT('Ctrl Pts',(2.25077488456509,-0.453531987451089,
6.18358159431314));
#23135=CARTESIAN_POINT('Ctrl Pts',(2.23885604798891,-0.501788628475886,
6.42713600578558));
#23136=CARTESIAN_POINT('Ctrl Pts',(2.22693721141274,-0.427548087273624,
6.6640659384009));
#23137=CARTESIAN_POINT('Ctrl Pts',(2.21501837483655,-0.24893405220493,6.83653182711616));
#23138=CARTESIAN_POINT('Ctrl Pts',(2.20309953826038,-0.00954995736342605,
6.90243105980056));
#23139=CARTESIAN_POINT('Ctrl Pts',(2.1911807016842,0.232165459400577,6.84567636076067));
#23140=CARTESIAN_POINT('Ctrl Pts',(2.17926186510802,0.417204446142715,6.68012249865921));
#23141=CARTESIAN_POINT('Ctrl Pts',(2.16734302853184,0.500394924062124,6.44618519743075));
#23142=CARTESIAN_POINT('Ctrl Pts',(2.15542419195566,0.461428696189393,6.20097232576562));
#23143=CARTESIAN_POINT('Ctrl Pts',(2.14350535537948,0.309817494450599,6.00434800046925));
#23144=CARTESIAN_POINT('Ctrl Pts',(2.1315865188033,0.0825744709686401,5.90430699091869));
#23145=CARTESIAN_POINT('Ctrl Pts',(2.11966768222712,-0.164828873860662,
5.92528289472092));
#23146=CARTESIAN_POINT('Ctrl Pts',(2.10774884565094,-0.371987775209309,
6.06212991827835));
#23147=CARTESIAN_POINT('Ctrl Pts',(2.09583000907476,-0.488342791333856,
6.2814932327682));
#23148=CARTESIAN_POINT('Ctrl Pts',(2.08788411802398,-0.486400997116553,
6.44696087140208));
#23149=CARTESIAN_POINT('Ctrl Pts',(2.08391117249858,-0.465688569540057,
6.52445999616013));
#23150=CARTESIAN_POINT('Ctrl Pts',(2.64826648250425,0.385547169725563,6.73369355690005));
#23151=CARTESIAN_POINT('Ctrl Pts',(2.64429353697886,0.44107990187464,6.66953143190698));
#23152=CARTESIAN_POINT('Ctrl Pts',(2.63634764592807,0.519418730749953,6.5129940576907));
#23153=CARTESIAN_POINT('Ctrl Pts',(2.62442880935189,0.510118007428568,6.25049189585148));
#23154=CARTESIAN_POINT('Ctrl Pts',(2.61250997277571,0.376276380452198,6.02452404575617));
#23155=CARTESIAN_POINT('Ctrl Pts',(2.60059113619954,0.150579831719341,5.89019841491327));
#23156=CARTESIAN_POINT('Ctrl Pts',(2.58867229962336,-0.111877986352145,
5.88033451451117));
#23157=CARTESIAN_POINT('Ctrl Pts',(2.57675346304718,-0.347023432783479,
5.99732787846002));
#23158=CARTESIAN_POINT('Ctrl Pts',(2.564834626471,-0.497453450012689,6.21262384103579));
#23159=CARTESIAN_POINT('Ctrl Pts',(2.55291578989482,-0.526444460181026,
6.47366140954065));
#23160=CARTESIAN_POINT('Ctrl Pts',(2.54099695331864,-0.426919346618493,
6.7167170754366));
#23161=CARTESIAN_POINT('Ctrl Pts',(2.52907811674246,-0.223174193283009,
6.88245524211623));
#23162=CARTESIAN_POINT('Ctrl Pts',(2.51715928016628,0.0350524704178637,
6.93041600240246));
#23163=CARTESIAN_POINT('Ctrl Pts',(2.5052404435901,0.284722093726431,6.84889099741939));
#23164=CARTESIAN_POINT('Ctrl Pts',(2.49332160701392,0.464885050226796,6.6577822578485));
#23165=CARTESIAN_POINT('Ctrl Pts',(2.48140277043774,0.531559769507257,6.40374342750432));
#23166=CARTESIAN_POINT('Ctrl Pts',(2.46948393386156,0.468469545343797,6.14879075163119));
#23167=CARTESIAN_POINT('Ctrl Pts',(2.45756509728538,0.291016032073294,5.95516354586177));
#23168=CARTESIAN_POINT('Ctrl Pts',(2.4456462607092,0.0425193718295788,5.87013029471448));
#23169=CARTESIAN_POINT('Ctrl Pts',(2.43372742413302,-0.216357163144678,
5.91444940567057));
#23170=CARTESIAN_POINT('Ctrl Pts',(2.42180858755684,-0.422416354717456,
6.07730165027367));
#23171=CARTESIAN_POINT('Ctrl Pts',(2.40988975098066,-0.525354811312622,
6.31893136309484));
#23172=CARTESIAN_POINT('Ctrl Pts',(2.39797091440449,-0.500043086181913,
6.58035163881449));
#23173=CARTESIAN_POINT('Ctrl Pts',(2.38605207782831,-0.352660304885654,
6.79774427841866));
#23174=CARTESIAN_POINT('Ctrl Pts',(2.37413324125213,-0.11918571055855,6.91803915687878));
#23175=CARTESIAN_POINT('Ctrl Pts',(2.36221440467595,0.143384627656033,6.91186975902934));
#23176=CARTESIAN_POINT('Ctrl Pts',(2.35029556809977,0.370951756306248,6.78074216492885));
#23177=CARTESIAN_POINT('Ctrl Pts',(2.33837673152359,0.507961743129952,6.55666738389136));
#23178=CARTESIAN_POINT('Ctrl Pts',(2.32645789494741,0.520967562726117,6.29434679258967));
#23179=CARTESIAN_POINT('Ctrl Pts',(2.31453905837123,0.406794220460285,6.05781837586191));
#23180=CARTESIAN_POINT('Ctrl Pts',(2.30262022179505,0.193313835397505,5.904823705531));
#23181=CARTESIAN_POINT('Ctrl Pts',(2.29070138521887,-0.067358531017915,
5.872712004543));
#23182=CARTESIAN_POINT('Ctrl Pts',(2.27878254864269,-0.311587260629241,
5.96932241712133));
#23183=CARTESIAN_POINT('Ctrl Pts',(2.26686371206651,-0.479750972411266,
6.17107030275971));
#23184=CARTESIAN_POINT('Ctrl Pts',(2.25494487549033,-0.530797361855725,
6.42870475627563));
#23185=CARTESIAN_POINT('Ctrl Pts',(2.24302603891415,-0.45226492573298,6.67933176541862));
#23186=CARTESIAN_POINT('Ctrl Pts',(2.23110720233797,-0.263325094846747,
6.86176802153349));
#23187=CARTESIAN_POINT('Ctrl Pts',(2.2191883657618,-0.0101020467317839,
6.93147693256131));
#23188=CARTESIAN_POINT('Ctrl Pts',(2.20726952918561,0.245587098572064,6.87144120673232));
#23189=CARTESIAN_POINT('Ctrl Pts',(2.19535069260943,0.441323311848774,6.69631656607358));
#23190=CARTESIAN_POINT('Ctrl Pts',(2.18343185603326,0.529323086465549,6.44885519432254));
#23191=CARTESIAN_POINT('Ctrl Pts',(2.17151301945708,0.488104195118536,6.18946640393034));
#23192=CARTESIAN_POINT('Ctrl Pts',(2.1595941828809,0.327728249264285,5.98147509599461));
#23193=CARTESIAN_POINT('Ctrl Pts',(2.14767534630472,0.0873481558956701,
5.87565064933844));
#23194=CARTESIAN_POINT('Ctrl Pts',(2.13575650972854,-0.174357740366956,
5.89783918404992));
#23195=CARTESIAN_POINT('Ctrl Pts',(2.12383767315236,-0.393492635182685,
6.04259742479108));
#23196=CARTESIAN_POINT('Ctrl Pts',(2.11191883657618,-0.516574211951732,
6.27464227796523));
#23197=CARTESIAN_POINT('Ctrl Pts',(2.10397294552539,-0.514520161323001,
6.44967571052055));
#23198=CARTESIAN_POINT('Ctrl Pts',(2.1,-0.492610334572592,6.53165511107541));
#23199=CARTESIAN_POINT('Ctrl Pts',(2.1,-0.492610334572592,6.53165511107541));
#23200=CARTESIAN_POINT('Ctrl Pts',(2.1,-0.49635409029725,6.51110955003273));
#23201=CARTESIAN_POINT('Ctrl Pts',(2.1,-0.498800810154946,6.4903688790591));
#23202=CARTESIAN_POINT('Ctrl Pts',(2.1,-0.499959864786037,6.46955396620066));
#23203=CARTESIAN_POINT('Ctrl Pts',(2.1,-0.500651891757826,6.45712618175713));
#23204=CARTESIAN_POINT('Ctrl Pts',(2.1,-0.500884496511186,6.4446719156573));
#23205=CARTESIAN_POINT('Ctrl Pts',(2.1,-0.500656300483376,6.43221745273261));
#23206=CARTESIAN_POINT('Ctrl Pts',(2.1,-0.50051140625946,6.42430942840331));
#23207=CARTESIAN_POINT('Ctrl Pts',(2.1,-0.500180531457043,6.41639915136081));
#23208=CARTESIAN_POINT('Ctrl Pts',(2.1,-0.499663295188048,6.40850057461429));
#23209=CARTESIAN_POINT('Ctrl Pts',(2.1,-0.498282684765909,6.38741764205526));
#23210=CARTESIAN_POINT('Ctrl Pts',(2.1,-0.495579671230594,6.36646338372735));
#23211=CARTESIAN_POINT('Ctrl Pts',(2.1,-0.491553183641479,6.34576661740274));
#23212=CARTESIAN_POINT('Ctrl Pts',(2.1,-0.489189370076283,6.33361625162834));
#23213=CARTESIAN_POINT('Ctrl Pts',(2.1,-0.486369014762183,6.32155472699449));
#23214=CARTESIAN_POINT('Ctrl Pts',(2.1,-0.483088515935984,6.30960963623735));
#23215=CARTESIAN_POINT('Ctrl Pts',(2.1,-0.481387749157045,6.30341673247256));
#23216=CARTESIAN_POINT('Ctrl Pts',(2.1,-0.479562349371169,6.29725234131795));
#23217=CARTESIAN_POINT('Ctrl Pts',(2.1,-0.477614701955683,6.29113018362027));
#23218=CARTESIAN_POINT('Ctrl Pts',(2.1,-0.47691994455268,6.28894631073394));
#23219=CARTESIAN_POINT('Ctrl Pts',(2.1,-0.476209763711948,6.28676817605457));
#23220=CARTESIAN_POINT('Ctrl Pts',(2.1,-0.475484170198335,6.28459593876059));
#23221=CARTESIAN_POINT('Ctrl Pts',(2.1,-0.467396057947338,6.26038224508792));
#23222=CARTESIAN_POINT('Ctrl Pts',(2.1,-0.457396800695749,6.23689933548638));
#23223=CARTESIAN_POINT('Ctrl Pts',(2.1,-0.445625784567883,6.21434556134776));
#23224=CARTESIAN_POINT('Ctrl Pts',(2.1,-0.433955482728322,6.19198476012551));
#23225=CARTESIAN_POINT('Ctrl Pts',(2.1,-0.420542677238036,6.17053620507075));
#23226=CARTESIAN_POINT('Ctrl Pts',(2.1,-0.405485055004202,6.15022640072986));
#23227=CARTESIAN_POINT('Ctrl Pts',(2.1,-0.401547018955012,6.14491475587622));
#23228=CARTESIAN_POINT('Ctrl Pts',(2.1,-0.397496316871279,6.13968122438761));
#23229=CARTESIAN_POINT('Ctrl Pts',(2.1,-0.393334380355557,6.13453037462292));
#23230=CARTESIAN_POINT('Ctrl Pts',(2.1,-0.390073732726515,6.1304949680257));
#23231=CARTESIAN_POINT('Ctrl Pts',(2.1,-0.386745496616124,6.12651133724348));
#23232=CARTESIAN_POINT('Ctrl Pts',(2.1,-0.383357029508834,6.12258887921439));
#23233=CARTESIAN_POINT('Ctrl Pts',(2.1,-0.371904123413349,6.109331101568));
#23234=CARTESIAN_POINT('Ctrl Pts',(2.1,-0.35974458511925,6.09674730862358));
#23235=CARTESIAN_POINT('Ctrl Pts',(2.1,-0.346917810301558,6.08490712758635));
#23236=CARTESIAN_POINT('Ctrl Pts',(2.1,-0.328748103732818,6.06813497572237));
#23237=CARTESIAN_POINT('Ctrl Pts',(2.1,-0.309239814555027,6.0528527033034));
#23238=CARTESIAN_POINT('Ctrl Pts',(2.1,-0.288595198791424,6.03919240881688));
#23239=CARTESIAN_POINT('Ctrl Pts',(2.1,-0.278215530931981,6.03232430716481));
#23240=CARTESIAN_POINT('Ctrl Pts',(2.1,-0.26754829677856,6.02586696377693));
#23241=CARTESIAN_POINT('Ctrl Pts',(2.1,-0.256618135875702,6.01984205852923));
#23242=CARTESIAN_POINT('Ctrl Pts',(2.1,-0.251611498381037,6.01708230807514));
#23243=CARTESIAN_POINT('Ctrl Pts',(2.1,-0.246550009240434,6.01441370455151));
#23244=CARTESIAN_POINT('Ctrl Pts',(2.1,-0.241448312426713,6.01184414666615));
#23245=CARTESIAN_POINT('Ctrl Pts',(2.1,-0.219923137629529,6.00100261988527));
#23246=CARTESIAN_POINT('Ctrl Pts',(2.1,-0.197628752691819,5.99188954333672));
#23247=CARTESIAN_POINT('Ctrl Pts',(2.1,-0.174757433630984,5.98462368929255));
#23248=CARTESIAN_POINT('Ctrl Pts',(2.1,-0.165576347867032,5.98170700447212));
#23249=CARTESIAN_POINT('Ctrl Pts',(2.1,-0.156302149790289,5.97908854410605));
#23250=CARTESIAN_POINT('Ctrl Pts',(2.1,-0.146946980180942,5.97677835925102));
#23251=CARTESIAN_POINT('Ctrl Pts',(2.1,-0.136233092918806,5.97413264985985));
#23252=CARTESIAN_POINT('Ctrl Pts',(2.1,-0.125412970644963,5.971891235028));
#23253=CARTESIAN_POINT('Ctrl Pts',(2.1,-0.11450999527259,5.97005741415271));
#23254=CARTESIAN_POINT('Ctrl Pts',(2.1,-0.107187489851071,5.96882580875667));
#23255=CARTESIAN_POINT('Ctrl Pts',(2.1,-0.0998276196797078,5.96777809712117));
#23256=CARTESIAN_POINT('Ctrl Pts',(2.1,-0.0924376450671474,5.96691584094867));
#23257=CARTESIAN_POINT('Ctrl Pts',(2.1,-0.0866290251654119,5.96623809594594));
#23258=CARTESIAN_POINT('Ctrl Pts',(2.1,-0.0808012215405976,5.96567507726491));
#23259=CARTESIAN_POINT('Ctrl Pts',(2.1,-0.0749735051801638,5.96522838192892));
#23260=CARTESIAN_POINT('Ctrl Pts',(2.1,-0.0505591545770249,5.96335701828132));
#23261=CARTESIAN_POINT('Ctrl Pts',(2.1,-0.0260794227869884,5.96351369057634));
#23262=CARTESIAN_POINT('Ctrl Pts',(2.1,-0.00179128476957419,5.96570484843602));
#23263=CARTESIAN_POINT('Ctrl Pts',(2.1,0.0210365858903797,5.96776426806632));
#23264=CARTESIAN_POINT('Ctrl Pts',(2.1,0.0436964113942735,5.97162157501662));
#23265=CARTESIAN_POINT('Ctrl Pts',(2.1,0.065956881641688,5.97732901798388));
#23266=CARTESIAN_POINT('Ctrl Pts',(2.1,0.0673808531784219,5.97769411522767));
#23267=CARTESIAN_POINT('Ctrl Pts',(2.1,0.0688031806876158,5.97806679811498));
#23268=CARTESIAN_POINT('Ctrl Pts',(2.1,0.0702237992588386,5.97844708639908));
#23269=CARTESIAN_POINT('Ctrl Pts',(2.1,0.0736400801676868,5.97936159760649));
#23270=CARTESIAN_POINT('Ctrl Pts',(2.1,0.0770464797446285,5.9803200895664));
#23271=CARTESIAN_POINT('Ctrl Pts',(2.1,0.0804421690761142,5.98132232055468));
#23272=CARTESIAN_POINT('Ctrl Pts',(2.6,0.322335278395778,6.67898325810255));
#23273=CARTESIAN_POINT('Ctrl Pts',(2.6,0.339120601259259,6.66300806279478));
#23274=CARTESIAN_POINT('Ctrl Pts',(2.6,0.354506984127668,6.64569922647684));
#23275=CARTESIAN_POINT('Ctrl Pts',(2.6,0.368421126683117,6.62729272970921));
#23276=CARTESIAN_POINT('Ctrl Pts',(2.6,0.38257126416386,6.60857404411556));
#23277=CARTESIAN_POINT('Ctrl Pts',(2.6,0.395199756274692,6.58871918836577));
#23278=CARTESIAN_POINT('Ctrl Pts',(2.6,0.406199318727697,6.56793181289168));
#23279=CARTESIAN_POINT('Ctrl Pts',(2.6,0.409616043928294,6.56147476062801));
#23280=CARTESIAN_POINT('Ctrl Pts',(2.6,0.412875324168305,6.55492747138162));
#23281=CARTESIAN_POINT('Ctrl Pts',(2.6,0.415973133660165,6.54829542707107));
#23282=CARTESIAN_POINT('Ctrl Pts',(2.6,0.418485108810516,6.54291758490618));
#23283=CARTESIAN_POINT('Ctrl Pts',(2.6,0.420891069789125,6.53748311927057));
#23284=CARTESIAN_POINT('Ctrl Pts',(2.6,0.423182724471203,6.53201048034897));
#23285=CARTESIAN_POINT('Ctrl Pts',(2.6,0.42826857782987,6.51986509070635));
#23286=CARTESIAN_POINT('Ctrl Pts',(2.6,0.432799982024353,6.50751484134792));
#23287=CARTESIAN_POINT('Ctrl Pts',(2.6,0.436762141475896,6.49499689828687));
#23288=CARTESIAN_POINT('Ctrl Pts',(2.6,0.444013330815057,6.47208768012373));
#23289=CARTESIAN_POINT('Ctrl Pts',(2.6,0.449360985234842,6.44861814961569));
#23290=CARTESIAN_POINT('Ctrl Pts',(2.6,0.452831510630463,6.42482689824574));
#23291=CARTESIAN_POINT('Ctrl Pts',(2.6,0.45503518273379,6.40972021814094));
#23292=CARTESIAN_POINT('Ctrl Pts',(2.6,0.456481100414613,6.39448317547527));
#23293=CARTESIAN_POINT('Ctrl Pts',(2.6,0.457165780866727,6.37917321940029));
#23294=CARTESIAN_POINT('Ctrl Pts',(2.6,0.457426442969031,6.37334462399588));
#23295=CARTESIAN_POINT('Ctrl Pts',(2.6,0.457576507352781,6.36750526353339));
#23296=CARTESIAN_POINT('Ctrl Pts',(2.6,0.457615909648183,6.36167325953747));
#23297=CARTESIAN_POINT('Ctrl Pts',(2.6,0.457783624314556,6.33684951273631));
#23298=CARTESIAN_POINT('Ctrl Pts',(2.6,0.455954126792007,6.3120946330561));
#23299=CARTESIAN_POINT('Ctrl Pts',(2.6,0.452154218947823,6.28765697027383));
#23300=CARTESIAN_POINT('Ctrl Pts',(2.6,0.45115674289519,6.28124208222728));
#23301=CARTESIAN_POINT('Ctrl Pts',(2.6,0.450023226879442,6.27484896612481));
#23302=CARTESIAN_POINT('Ctrl Pts',(2.6,0.448753579228988,6.26848198366457));
#23303=CARTESIAN_POINT('Ctrl Pts',(2.6,0.444848441945282,6.24889864447494));
#23304=CARTESIAN_POINT('Ctrl Pts',(2.6,0.43965712635916,6.22956230418047));
#23305=CARTESIAN_POINT('Ctrl Pts',(2.6,0.433239797159997,6.21057739588651));
#23306=CARTESIAN_POINT('Ctrl Pts',(2.6,0.431489703713964,6.20539995172748));
#23307=CARTESIAN_POINT('Ctrl Pts',(2.6,0.429647959283524,6.200247760375));
#23308=CARTESIAN_POINT('Ctrl Pts',(2.6,0.427716565518185,6.19512580861043));
#23309=CARTESIAN_POINT('Ctrl Pts',(2.6,0.418824441384019,6.17154437652905));
#23310=CARTESIAN_POINT('Ctrl Pts',(2.6,0.408091715271334,6.14874908227563));
#23311=CARTESIAN_POINT('Ctrl Pts',(2.6,0.395672419048227,6.12693682894624));
#23312=CARTESIAN_POINT('Ctrl Pts',(2.6,0.383092367331082,6.10484223759245));
#23313=CARTESIAN_POINT('Ctrl Pts',(2.6,0.368781416403301,6.08375495651898));
#23314=CARTESIAN_POINT('Ctrl Pts',(2.6,0.352848584276632,6.06389024080292));
#23315=CARTESIAN_POINT('Ctrl Pts',(2.6,0.350477674538742,6.06093424104361));
#23316=CARTESIAN_POINT('Ctrl Pts',(2.6,0.348070766049518,6.05800535381594));
#23317=CARTESIAN_POINT('Ctrl Pts',(2.6,0.345628131270321,6.05510433731261));
#23318=CARTESIAN_POINT('Ctrl Pts',(2.6,0.341175445450433,6.04981606615654));
#23319=CARTESIAN_POINT('Ctrl Pts',(2.6,0.336604054215743,6.04462039757467));
#23320=CARTESIAN_POINT('Ctrl Pts',(2.6,0.331917615661801,6.03951989728949));
#23321=CARTESIAN_POINT('Ctrl Pts',(2.6,0.327197865992937,6.03438314274658));
#23322=CARTESIAN_POINT('Ctrl Pts',(2.6,0.322366287452079,6.02934835553984));
#23323=CARTESIAN_POINT('Ctrl Pts',(2.6,0.317432494385971,6.02442266645077));
#23324=CARTESIAN_POINT('Ctrl Pts',(2.6,0.305161639297739,6.01217196679398));
#23325=CARTESIAN_POINT('Ctrl Pts',(2.6,0.292249931632248,6.00058562939064));
#23326=CARTESIAN_POINT('Ctrl Pts',(2.6,0.278765100808516,5.98969663827542));
#23327=CARTESIAN_POINT('Ctrl Pts',(2.6,0.268765025516792,5.98162158472625));
#23328=CARTESIAN_POINT('Ctrl Pts',(2.6,0.258449546075054,5.97393011620472));
#23329=CARTESIAN_POINT('Ctrl Pts',(2.6,0.247843342520938,5.96663792616377));
#23330=CARTESIAN_POINT('Ctrl Pts',(2.6,0.241099106168833,5.96200099336216));
#23331=CARTESIAN_POINT('Ctrl Pts',(2.6,0.234236247932732,5.9575251822992));
#23332=CARTESIAN_POINT('Ctrl Pts',(2.6,0.227275760973999,5.95322352477529));
#23333=CARTESIAN_POINT('Ctrl Pts',(2.6,0.204751973270828,5.93930357615464));
#23334=CARTESIAN_POINT('Ctrl Pts',(2.6,0.181175137781382,5.92718033261133));
#23335=CARTESIAN_POINT('Ctrl Pts',(2.6,0.156760783265524,5.91698457674055));
#23336=CARTESIAN_POINT('Ctrl Pts',(2.6,0.152585729857118,5.91524101947092));
#23337=CARTESIAN_POINT('Ctrl Pts',(2.6,0.148386104006604,5.91355392287942));
#23338=CARTESIAN_POINT('Ctrl Pts',(2.6,0.144162892324896,5.91192406382743));
#23339=CARTESIAN_POINT('Ctrl Pts',(2.6,0.140229927621667,5.91040621944599));
#23340=CARTESIAN_POINT('Ctrl Pts',(2.6,0.136276507298105,5.90893801577657));
#23341=CARTESIAN_POINT('Ctrl Pts',(2.6,0.132303594671778,5.90751949357016));
#23342=CARTESIAN_POINT('Ctrl Pts',(2.3579681670589,-0.426284649716722,6.39998978457651));
#23343=CARTESIAN_POINT('Ctrl Pts',(2.35918653419807,-0.426303967962151,
6.37823165906101));
#23344=CARTESIAN_POINT('Ctrl Pts',(2.36040490133724,-0.424667502862756,
6.35647641245579));
#23345=CARTESIAN_POINT('Ctrl Pts',(2.36162326847641,-0.421350422927922,
6.33498050516036));
#23346=CARTESIAN_POINT('Ctrl Pts',(2.3655962140018,-0.41053383286997,6.26488499293085));
#23347=CARTESIAN_POINT('Ctrl Pts',(2.3695691595272,-0.381846728178515,6.19754711846157));
#23348=CARTESIAN_POINT('Ctrl Pts',(2.37354210505259,-0.338790672280628,
6.14118617891461));
#23349=CARTESIAN_POINT('Ctrl Pts',(2.37751505057798,-0.295734616382741,
6.08482523936765));
#23350=CARTESIAN_POINT('Ctrl Pts',(2.38148799610338,-0.238309609278423,
6.03944123474302));
#23351=CARTESIAN_POINT('Ctrl Pts',(2.38546094162877,-0.173524978230831,
6.01057376109627));
#23352=CARTESIAN_POINT('Ctrl Pts',(2.38943388715416,-0.10874034718324,5.98170628744951));
#23353=CARTESIAN_POINT('Ctrl Pts',(2.39340683267956,-0.036596092192376,
5.96935534478063));
#23354=CARTESIAN_POINT('Ctrl Pts',(2.39737977820495,0.0341018201830637,
5.97502849571334));
#23355=CARTESIAN_POINT('Ctrl Pts',(2.40135272373034,0.104799732558504,5.98070164664604));
#23356=CARTESIAN_POINT('Ctrl Pts',(2.40532566925574,0.174051302318518,6.00439889118032));
#23357=CARTESIAN_POINT('Ctrl Pts',(2.40929861478113,0.233403645578344,6.0432277310782));
#23358=CARTESIAN_POINT('Ctrl Pts',(2.41327156030652,0.29275598883817,6.08205657097609));
#23359=CARTESIAN_POINT('Ctrl Pts',(2.41724450583192,0.342209105597808,6.13601700623758));
#23360=CARTESIAN_POINT('Ctrl Pts',(2.42121745135731,0.375726721884694,6.19852259672729));
#23361=CARTESIAN_POINT('Ctrl Pts',(2.4251903968827,0.40924433817158,6.261028187217));
#23362=CARTESIAN_POINT('Ctrl Pts',(2.4291633424081,0.426826453985716,6.33207893293493));
#23363=CARTESIAN_POINT('Ctrl Pts',(2.43313628793349,0.426326986682199,6.40300234245982));
#23364=CARTESIAN_POINT('Ctrl Pts',(2.43710923345888,0.425827519378683,6.4739257519847));
#23365=CARTESIAN_POINT('Ctrl Pts',(2.44108217898427,0.407246468957515,6.54472182531654));
#23366=CARTESIAN_POINT('Ctrl Pts',(2.44505512450967,0.372851848709961,6.60674915389561));
#23367=CARTESIAN_POINT('Ctrl Pts',(2.44902807003506,0.338457228462407,6.66877648247468));
#23368=CARTESIAN_POINT('Ctrl Pts',(2.45300101556045,0.288249038388467,6.72203506630097));
#23369=CARTESIAN_POINT('Ctrl Pts',(2.45697396108585,0.228355716569631,6.76002413778667));
#23370=CARTESIAN_POINT('Ctrl Pts',(2.46094690661124,0.168462394750795,6.79801320927237));
#23371=CARTESIAN_POINT('Ctrl Pts',(2.46491985213663,0.0988839411870617,
6.82073276841748));
#23372=CARTESIAN_POINT('Ctrl Pts',(2.46889279766203,0.0281131406535831,
6.82540964542417));
#23373=CARTESIAN_POINT('Ctrl Pts',(2.47286574318742,-0.0426576598798955,
6.83008652243086));
#23374=CARTESIAN_POINT('Ctrl Pts',(2.47683868871281,-0.11462080738312,6.81672071729912));
#23375=CARTESIAN_POINT('Ctrl Pts',(2.48081163423821,-0.178992444175497,
6.78694368501647));
#23376=CARTESIAN_POINT('Ctrl Pts',(2.4847845797636,-0.243364080967874,6.75716665273382));
#23377=CARTESIAN_POINT('Ctrl Pts',(2.48875752528899,-0.300144207049405,
6.71097839330025));
#23378=CARTESIAN_POINT('Ctrl Pts',(2.49273047081439,-0.342402203643058,
6.65401663255403));
#23379=CARTESIAN_POINT('Ctrl Pts',(2.49670341633978,-0.384660200236712,
6.59705487180782));
#23380=CARTESIAN_POINT('Ctrl Pts',(2.50067636186517,-0.41239606734249,6.52931960974896));
#23381=CARTESIAN_POINT('Ctrl Pts',(2.50464930739057,-0.422224363177276,
6.45907873054876));
#23382=CARTESIAN_POINT('Ctrl Pts',(2.50575559394668,-0.424961101318294,
6.4395198063571));
#23383=CARTESIAN_POINT('Ctrl Pts',(2.50686188050279,-0.426309336731809,
6.41976660365709));
#23384=CARTESIAN_POINT('Ctrl Pts',(2.50796816705891,-0.426290360635438,
6.40001083203199));
#23385=CARTESIAN_POINT('Ctrl Pts',(2.6,-0.132288496556895,5.90755938055567));
#23386=CARTESIAN_POINT('Ctrl Pts',(2.59602705447461,-0.214239653399634,
5.92957461427473));
#23387=CARTESIAN_POINT('Ctrl Pts',(2.58808116342382,-0.366850103542102,
6.0153123398751));
#23388=CARTESIAN_POINT('Ctrl Pts',(2.57616232684764,-0.506266020658281,
6.23792666630748));
#23389=CARTESIAN_POINT('Ctrl Pts',(2.56424349027146,-0.522062886964902,
6.50008215105946));
#23390=CARTESIAN_POINT('Ctrl Pts',(2.55232465369528,-0.410425773087965,
6.73782039475945));
#23391=CARTESIAN_POINT('Ctrl Pts',(2.54040581711911,-0.19858907062663,6.89308342832313));
#23392=CARTESIAN_POINT('Ctrl Pts',(2.52848698054292,0.0617246536500735,
6.92797742227401));
#23393=CARTESIAN_POINT('Ctrl Pts',(2.51656814396674,0.306971377021502,6.8339796336226));
#23394=CARTESIAN_POINT('Ctrl Pts',(2.50464930739056,0.477279320739804,6.63403891232169));
#23395=CARTESIAN_POINT('Ctrl Pts',(2.49273047081439,0.531073600862929,6.3769640630774));
#23396=CARTESIAN_POINT('Ctrl Pts',(2.48081163423821,0.455221493256117,6.12551290982166));
#23397=CARTESIAN_POINT('Ctrl Pts',(2.46889279766203,0.268240284898955,5.94106977614238));
#23398=CARTESIAN_POINT('Ctrl Pts',(2.45697396108585,0.0157759417689948,
5.86866121228054));
#23399=CARTESIAN_POINT('Ctrl Pts',(2.44505512450967,-0.240539628301038,
5.92596363104932));
#23400=CARTESIAN_POINT('Ctrl Pts',(2.43313628793349,-0.438134411540293,
6.09898832463164));
#23401=CARTESIAN_POINT('Ctrl Pts',(2.42121745135731,-0.528771348081292,
6.34549630925116));
#23402=CARTESIAN_POINT('Ctrl Pts',(2.40929861478113,-0.490324055555984,
6.60530979488368));
#23403=CARTESIAN_POINT('Ctrl Pts',(2.39737977820495,-0.332178326477852,
6.81500283186379));
#23404=CARTESIAN_POINT('Ctrl Pts',(2.38546094162877,-0.092940867251264,
6.92338493135519));
#23405=CARTESIAN_POINT('Ctrl Pts',(2.37354210505259,0.168985416607936,6.90399773818908));
#23406=CARTESIAN_POINT('Ctrl Pts',(2.36162326847641,0.38965879870384,6.76157407502307));
#23407=CARTESIAN_POINT('Ctrl Pts',(2.34970443190023,0.515208255680234,6.5308825596382));
#23408=CARTESIAN_POINT('Ctrl Pts',(2.33778559532405,0.514984518987432,6.26823985300105));
#23409=CARTESIAN_POINT('Ctrl Pts',(2.32586675874787,0.389042207488899,6.03776257519368));
#23410=CARTESIAN_POINT('Ctrl Pts',(2.31394792217169,0.168126493747137,5.89571508724314));
#23411=CARTESIAN_POINT('Ctrl Pts',(2.30202908559551,-0.0938324405162212,
5.87677417471489));
#23412=CARTESIAN_POINT('Ctrl Pts',(2.29011024901934,-0.332884898468083,
5.98556371357228));
#23413=CARTESIAN_POINT('Ctrl Pts',(2.27819141244316,-0.490673136844557,
6.19552588451105));
#23414=CARTESIAN_POINT('Ctrl Pts',(2.26627257586698,-0.528677721240565,
6.45540449655913));
#23415=CARTESIAN_POINT('Ctrl Pts',(2.2543537392908,-0.437620931409163,6.70175770318116));
#23416=CARTESIAN_POINT('Ctrl Pts',(2.24243490271462,-0.239731649313908,
6.87444549491937));
#23417=CARTESIAN_POINT('Ctrl Pts',(2.23051606613844,0.0166811816108265,
6.93131114145764));
#23418=CARTESIAN_POINT('Ctrl Pts',(2.21859722956226,0.269021783055123,6.85847254173578));
#23419=CARTESIAN_POINT('Ctrl Pts',(2.20667839298608,0.455688500581004,6.67371112931225));
#23420=CARTESIAN_POINT('Ctrl Pts',(2.1947595564099,0.53111204424701,6.42213106706975));
#23421=CARTESIAN_POINT('Ctrl Pts',(2.18284071983372,0.476879959029563,6.1651483330086));
#23422=CARTESIAN_POINT('Ctrl Pts',(2.17092188325754,0.306231393425269,5.96549786619889));
#23423=CARTESIAN_POINT('Ctrl Pts',(2.15900304668136,0.0608253588918372,
5.8719184725451));
#23424=CARTESIAN_POINT('Ctrl Pts',(2.14708421010518,-0.199429574813985,
5.90725502825896));
#23425=CARTESIAN_POINT('Ctrl Pts',(2.135165373529,-0.410999230249818,6.06288076079265));
#23426=CARTESIAN_POINT('Ctrl Pts',(2.12324653695282,-0.522235994732442,
6.30080495423084));
#23427=CARTESIAN_POINT('Ctrl Pts',(2.11132770037665,-0.505982491766854,
6.56294356165447));
#23428=CARTESIAN_POINT('Ctrl Pts',(2.09940886380046,-0.366211204665212,
6.78530674521469));
#23429=CARTESIAN_POINT('Ctrl Pts',(2.08749002722428,-0.137033499838515,
6.91360287657764));
#23430=CARTESIAN_POINT('Ctrl Pts',(2.07557119064811,0.125581190928044,6.91652919922544));
#23431=CARTESIAN_POINT('Ctrl Pts',(2.06365235407193,0.357565218298462,6.79333282215497));
#23432=CARTESIAN_POINT('Ctrl Pts',(2.05570646302114,0.453961018087142,6.64722068416873));
#23433=CARTESIAN_POINT('Ctrl Pts',(2.05173351749575,0.481760682217403,6.56704686488953));
#23434=CARTESIAN_POINT('Ctrl Pts',(2.61608882750142,-0.12505876634041,5.9344718704462));
#23435=CARTESIAN_POINT('Ctrl Pts',(2.61211588197602,-0.202531190940192,
5.95528394436993));
#23436=CARTESIAN_POINT('Ctrl Pts',(2.60416999092524,-0.346801290927786,
6.03633599705392));
#23437=CARTESIAN_POINT('Ctrl Pts',(2.59225115434906,-0.478597955464431,
6.24678417477103));
#23438=CARTESIAN_POINT('Ctrl Pts',(2.58033231777288,-0.493531503458158,
6.49461253752179));
#23439=CARTESIAN_POINT('Ctrl Pts',(2.5684134811967,-0.387995496151209,6.71935809169225));
#23440=CARTESIAN_POINT('Ctrl Pts',(2.55649464462052,-0.187735931903752,
6.86613580813106));
#23441=CARTESIAN_POINT('Ctrl Pts',(2.54457580804434,0.0583513248632879,
6.89912280208567));
#23442=CARTESIAN_POINT('Ctrl Pts',(2.53265697146816,0.290195010989602,6.81026210902899));
#23443=CARTESIAN_POINT('Ctrl Pts',(2.52073813489198,0.451195414605367,6.62124839583474));
#23444=CARTESIAN_POINT('Ctrl Pts',(2.5088192983158,0.50204977067914,6.37822300556726));
#23445=CARTESIAN_POINT('Ctrl Pts',(2.49690046173962,0.430343074719011,6.14051396933589));
#23446=CARTESIAN_POINT('Ctrl Pts',(2.48498162516344,0.253580621031822,5.96615088140125));
#23447=CARTESIAN_POINT('Ctrl Pts',(2.47306278858726,0.0149137670080035,
5.89769953525455));
#23448=CARTESIAN_POINT('Ctrl Pts',(2.46114395201109,-0.227393839632693,
5.95187030585109));
#23449=CARTESIAN_POINT('Ctrl Pts',(2.44922511543491,-0.414189823186519,
6.11543898558529));
#23450=CARTESIAN_POINT('Ctrl Pts',(2.43730627885873,-0.499873338864062,
6.34847500347002));
#23451=CARTESIAN_POINT('Ctrl Pts',(2.42538744228255,-0.463527238503961,
6.59408936025449));
#23452=CARTESIAN_POINT('Ctrl Pts',(2.41346860570637,-0.314024369431667,
6.79232241299485));
#23453=CARTESIAN_POINT('Ctrl Pts',(2.40154976913019,-0.0878615337203718,
6.89478129648476));
#23454=CARTESIAN_POINT('Ctrl Pts',(2.38963093255401,0.159750154250334,6.87645363744213));
#23455=CARTESIAN_POINT('Ctrl Pts',(2.37771209597783,0.368363462643409,6.74181360390328));
#23456=CARTESIAN_POINT('Ctrl Pts',(2.36579325940165,0.487051486264749,6.52372966561601));
#23457=CARTESIAN_POINT('Ctrl Pts',(2.35387442282547,0.486839977059375,6.27544070825967));
#23458=CARTESIAN_POINT('Ctrl Pts',(2.34195558624929,0.367780568902201,6.05755929920087));
#23459=CARTESIAN_POINT('Ctrl Pts',(2.33003674967311,0.158938172587915,5.92327488243597));
#23460=CARTESIAN_POINT('Ctrl Pts',(2.31811791309693,-0.0887043814019138,
5.90536911424148));
#23461=CARTESIAN_POINT('Ctrl Pts',(2.30619907652075,-0.314692326387328,
6.0082131700313));
#23462=CARTESIAN_POINT('Ctrl Pts',(2.29428023994457,-0.463857242067669,
6.20670064822607));
#23463=CARTESIAN_POINT('Ctrl Pts',(2.28236140336839,-0.499784828846167,
6.45237657218681));
#23464=CARTESIAN_POINT('Ctrl Pts',(2.27044256679221,-0.413704405380657,
6.68526627088336));
#23465=CARTESIAN_POINT('Ctrl Pts',(2.25852373021604,-0.226630017698138,
6.84851646087657));
#23466=CARTESIAN_POINT('Ctrl Pts',(2.24660489363986,0.0157695343710637,
6.90227432938608));
#23467=CARTESIAN_POINT('Ctrl Pts',(2.23468605706368,0.254319409345632,6.83341644937185));
#23468=CARTESIAN_POINT('Ctrl Pts',(2.2227672204875,0.430784559515061,6.65875247702062));
#23469=CARTESIAN_POINT('Ctrl Pts',(2.21084838391132,0.502086113084658,6.42092157683831));
#23470=CARTESIAN_POINT('Ctrl Pts',(2.19892954733514,0.450817878507322,6.1779832675451));
#23471=CARTESIAN_POINT('Ctrl Pts',(2.18701071075896,0.289495468413598,5.98924394607454));
#23472=CARTESIAN_POINT('Ctrl Pts',(2.17509187418278,0.05750117767764,5.90077878221055));
#23473=CARTESIAN_POINT('Ctrl Pts',(2.1631730376066,-0.188530501496047,5.93418415137954));
#23474=CARTESIAN_POINT('Ctrl Pts',(2.15125420103042,-0.388537613168766,
6.08130474484033));
#23475=CARTESIAN_POINT('Ctrl Pts',(2.13933536445424,-0.493695150671756,
6.30622608636544));
#23476=CARTESIAN_POINT('Ctrl Pts',(2.12741652787806,-0.478329921778157,
6.55403849415475));
#23477=CARTESIAN_POINT('Ctrl Pts',(2.11549769130188,-0.346197308665989,
6.76424925426879));
#23478=CARTESIAN_POINT('Ctrl Pts',(2.1035788547257,-0.129544449314556,6.88553384311886));
#23479=CARTESIAN_POINT('Ctrl Pts',(2.09166001814953,0.11871802327322,6.88830023860881));
#23480=CARTESIAN_POINT('Ctrl Pts',(2.07974118157334,0.338023836164873,6.77183669616154));
#23481=CARTESIAN_POINT('Ctrl Pts',(2.07179529052256,0.429151486079503,6.63370976752069));
#23482=CARTESIAN_POINT('Ctrl Pts',(2.06782234499716,0.455431864126683,6.55791754678483));
#23483=CARTESIAN_POINT('Ctrl Pts',(2.63217765500284,-0.117829036123926,
5.96138436033673));
#23484=CARTESIAN_POINT('Ctrl Pts',(2.62820470947744,-0.190822728480749,
5.98099327446513));
#23485=CARTESIAN_POINT('Ctrl Pts',(2.62025881842666,-0.326752478313469,
6.05735965423274));
#23486=CARTESIAN_POINT('Ctrl Pts',(2.60833998185048,-0.450929890270581,
6.25564168323458));
#23487=CARTESIAN_POINT('Ctrl Pts',(2.5964211452743,-0.465000119951414,6.48914292398412));
#23488=CARTESIAN_POINT('Ctrl Pts',(2.58450230869812,-0.365565219214455,
6.70089578862506));
#23489=CARTESIAN_POINT('Ctrl Pts',(2.57258347212194,-0.176882793180874,
6.83918818793898));
#23490=CARTESIAN_POINT('Ctrl Pts',(2.56066463554576,0.0549779960765018,
6.87026818189733));
#23491=CARTESIAN_POINT('Ctrl Pts',(2.54874579896958,0.273418644957702,6.78654458443538));
#23492=CARTESIAN_POINT('Ctrl Pts',(2.5368269623934,0.42511150847093,6.60845787934779));
#23493=CARTESIAN_POINT('Ctrl Pts',(2.52490812581722,0.473025940495352,6.37948194805711));
#23494=CARTESIAN_POINT('Ctrl Pts',(2.51298928924104,0.405464656181905,6.15551502885011));
#23495=CARTESIAN_POINT('Ctrl Pts',(2.50107045266486,0.23892095716469,5.99123198666013));
#23496=CARTESIAN_POINT('Ctrl Pts',(2.48915161608868,0.014051592247013,5.92673785822857));
#23497=CARTESIAN_POINT('Ctrl Pts',(2.4772327795125,-0.214248050964349,5.97777698065287));
#23498=CARTESIAN_POINT('Ctrl Pts',(2.46531394293632,-0.390245234832745,
6.13188964653893));
#23499=CARTESIAN_POINT('Ctrl Pts',(2.45339510636014,-0.470975329646833,
6.35145369768889));
#23500=CARTESIAN_POINT('Ctrl Pts',(2.44147626978396,-0.436730421451937,
6.5828689256253));
#23501=CARTESIAN_POINT('Ctrl Pts',(2.42955743320779,-0.295870412385483,
6.76964199412591));
#23502=CARTESIAN_POINT('Ctrl Pts',(2.41763859663161,-0.0827822001894799,
6.86617766161433));
#23503=CARTESIAN_POINT('Ctrl Pts',(2.40571976005543,0.150514891892733,6.84890953669518));
#23504=CARTESIAN_POINT('Ctrl Pts',(2.39380092347925,0.347068126582978,6.7220531327835));
#23505=CARTESIAN_POINT('Ctrl Pts',(2.38188208690307,0.458894716849264,6.51657677159381));
#23506=CARTESIAN_POINT('Ctrl Pts',(2.36996325032689,0.458695435131318,6.28264156351829));
#23507=CARTESIAN_POINT('Ctrl Pts',(2.35804441375071,0.346518930315503,6.07735602320807));
#23508=CARTESIAN_POINT('Ctrl Pts',(2.34612557717453,0.149749851428694,5.9508346776288));
#23509=CARTESIAN_POINT('Ctrl Pts',(2.33420674059835,-0.0835763222876063,
5.93396405376808));
#23510=CARTESIAN_POINT('Ctrl Pts',(2.32228790402217,-0.296499754306572,
6.03086262649031));
#23511=CARTESIAN_POINT('Ctrl Pts',(2.31036906744599,-0.437041347290782,
6.2178754119411));
#23512=CARTESIAN_POINT('Ctrl Pts',(2.29845023086981,-0.470891936451769,
6.44934864781448));
#23513=CARTESIAN_POINT('Ctrl Pts',(2.28653139429363,-0.389787879352151,
6.66877483858555));
#23514=CARTESIAN_POINT('Ctrl Pts',(2.27461255771745,-0.213528386082369,
6.82258742683378));
#23515=CARTESIAN_POINT('Ctrl Pts',(2.26269372114127,0.0148578871313011,
6.87323751731453));
#23516=CARTESIAN_POINT('Ctrl Pts',(2.2507748845651,0.239617035636141,6.80836035700791));
#23517=CARTESIAN_POINT('Ctrl Pts',(2.23885604798891,0.405880618449119,6.64379382472899));
#23518=CARTESIAN_POINT('Ctrl Pts',(2.22693721141274,0.473060181922306,6.41971208660688));
#23519=CARTESIAN_POINT('Ctrl Pts',(2.21501837483656,0.424755797985082,6.1908182020816));
#23520=CARTESIAN_POINT('Ctrl Pts',(2.20309953826038,0.272759543401928,6.01299002595018));
#23521=CARTESIAN_POINT('Ctrl Pts',(2.1911807016842,0.0541769964634428,5.92963909187599));
#23522=CARTESIAN_POINT('Ctrl Pts',(2.17926186510802,-0.17763142817811,5.96111327450012));
#23523=CARTESIAN_POINT('Ctrl Pts',(2.16734302853184,-0.366075996087714,
6.099728728888));
#23524=CARTESIAN_POINT('Ctrl Pts',(2.15542419195566,-0.465154306611069,
6.31164721850004));
#23525=CARTESIAN_POINT('Ctrl Pts',(2.14350535537948,-0.450677351789461,
6.54513342665504));
#23526=CARTESIAN_POINT('Ctrl Pts',(2.1315865188033,-0.326183412666766,6.74319176332289));
#23527=CARTESIAN_POINT('Ctrl Pts',(2.11966768222712,-0.122055398790597,
6.85746480966008));
#23528=CARTESIAN_POINT('Ctrl Pts',(2.10774884565094,0.111854855618396,6.8600712779922));
#23529=CARTESIAN_POINT('Ctrl Pts',(2.09583000907476,0.318482454031284,6.7503405701681));
#23530=CARTESIAN_POINT('Ctrl Pts',(2.08788411802398,0.404341954071864,6.62019885087265));
#23531=CARTESIAN_POINT('Ctrl Pts',(2.08391117249858,0.429103046035963,6.54878822868013));
#23532=CARTESIAN_POINT('Ctrl Pts',(2.64826648250425,-0.110599305907441,
5.98829685022726));
#23533=CARTESIAN_POINT('Ctrl Pts',(2.64429353697886,-0.179114266021306,
6.00670260456034));
#23534=CARTESIAN_POINT('Ctrl Pts',(2.63634764592807,-0.306703665699153,
6.07838331141156));
#23535=CARTESIAN_POINT('Ctrl Pts',(2.6244288093519,-0.423261825076731,6.26449919169813));
#23536=CARTESIAN_POINT('Ctrl Pts',(2.61250997277572,-0.436468736444671,
6.48367331044645));
#23537=CARTESIAN_POINT('Ctrl Pts',(2.60059113619953,-0.3431349422777,6.68243348555786));
#23538=CARTESIAN_POINT('Ctrl Pts',(2.58867229962336,-0.166029654457996,
6.81224056774691));
#23539=CARTESIAN_POINT('Ctrl Pts',(2.57675346304718,0.0516046672897163,
6.84141356170898));
#23540=CARTESIAN_POINT('Ctrl Pts',(2.564834626471,0.256642278925802,6.76282705984177));
#23541=CARTESIAN_POINT('Ctrl Pts',(2.55291578989482,0.399027602336494,6.59566736286083));
#23542=CARTESIAN_POINT('Ctrl Pts',(2.54099695331864,0.444002110311564,6.38074089054697));
#23543=CARTESIAN_POINT('Ctrl Pts',(2.52907811674246,0.380586237644799,6.17051608836433));
#23544=CARTESIAN_POINT('Ctrl Pts',(2.51715928016628,0.224261293297557,6.016313091919));
#23545=CARTESIAN_POINT('Ctrl Pts',(2.5052404435901,0.0131894174860218,5.95577618120258));
#23546=CARTESIAN_POINT('Ctrl Pts',(2.49332160701392,-0.201102262296004,
6.00368365545465));
#23547=CARTESIAN_POINT('Ctrl Pts',(2.48140277043774,-0.366300646478971,
6.14834030749258));
#23548=CARTESIAN_POINT('Ctrl Pts',(2.46948393386156,-0.442077320429603,
6.35443239190776));
#23549=CARTESIAN_POINT('Ctrl Pts',(2.45756509728538,-0.409933604399914,
6.57164849099611));
#23550=CARTESIAN_POINT('Ctrl Pts',(2.4456462607092,-0.277716455339298,6.74696157525698));
#23551=CARTESIAN_POINT('Ctrl Pts',(2.43372742413302,-0.0777028666585877,
6.8375740267439));
#23552=CARTESIAN_POINT('Ctrl Pts',(2.42180858755684,0.141279629535131,6.82136543594824));
#23553=CARTESIAN_POINT('Ctrl Pts',(2.40988975098066,0.325772790522547,6.70229266166372));
#23554=CARTESIAN_POINT('Ctrl Pts',(2.39797091440449,0.430737947433779,6.50942387757162));
#23555=CARTESIAN_POINT('Ctrl Pts',(2.38605207782831,0.43055089320326,6.28984241877691));
#23556=CARTESIAN_POINT('Ctrl Pts',(2.37413324125213,0.325257291728805,6.09715274721527));
#23557=CARTESIAN_POINT('Ctrl Pts',(2.36221440467595,0.140561530269473,5.97839447282163));
#23558=CARTESIAN_POINT('Ctrl Pts',(2.35029556809977,-0.0784482631732989,
5.96255899329468));
#23559=CARTESIAN_POINT('Ctrl Pts',(2.33837673152359,-0.278307182225817,
6.05351208294933));
#23560=CARTESIAN_POINT('Ctrl Pts',(2.32645789494741,-0.410225452513894,
6.22905017565613));
#23561=CARTESIAN_POINT('Ctrl Pts',(2.31453905837123,-0.44199904405737,6.44632072344216));
#23562=CARTESIAN_POINT('Ctrl Pts',(2.30262022179505,-0.365871353323644,
6.65228340628776));
#23563=CARTESIAN_POINT('Ctrl Pts',(2.29070138521887,-0.200426754466599,
6.79665839279099));
#23564=CARTESIAN_POINT('Ctrl Pts',(2.27878254864269,0.0139462398915382,
6.84420070524297));
#23565=CARTESIAN_POINT('Ctrl Pts',(2.26686371206651,0.22491466192665,6.78330426464398));
#23566=CARTESIAN_POINT('Ctrl Pts',(2.25494487549033,0.380976677383177,6.62883517243736));
#23567=CARTESIAN_POINT('Ctrl Pts',(2.24302603891415,0.444034250759953,6.41850259637544));
#23568=CARTESIAN_POINT('Ctrl Pts',(2.23110720233797,0.398693717462841,6.2036531366181));
#23569=CARTESIAN_POINT('Ctrl Pts',(2.2191883657618,0.256023618390257,6.03673610582583));
#23570=CARTESIAN_POINT('Ctrl Pts',(2.20726952918561,0.0508528152492455,
5.95849940154143));
#23571=CARTESIAN_POINT('Ctrl Pts',(2.19535069260944,-0.166732354860172,
5.9880423976207));
#23572=CARTESIAN_POINT('Ctrl Pts',(2.18343185603326,-0.343614379006663,
6.11815271293568));
#23573=CARTESIAN_POINT('Ctrl Pts',(2.17151301945708,-0.436613462550383,
6.31706835063465));
#23574=CARTESIAN_POINT('Ctrl Pts',(2.1595941828809,-0.423024781800764,6.53622835915532));
#23575=CARTESIAN_POINT('Ctrl Pts',(2.14767534630472,-0.306169516667542,
6.72213427237698));
#23576=CARTESIAN_POINT('Ctrl Pts',(2.13575650972854,-0.114566348266639,
6.8293957762013));
#23577=CARTESIAN_POINT('Ctrl Pts',(2.12383767315236,0.104991687963572,6.83184231737557));
#23578=CARTESIAN_POINT('Ctrl Pts',(2.11191883657618,0.298941071897694,6.72884444417467));
#23579=CARTESIAN_POINT('Ctrl Pts',(2.10397294552539,0.379532422064226,6.60668793422461));
#23580=CARTESIAN_POINT('Ctrl Pts',(2.1,0.402774227945242,6.53965891057542));
#23581=CARTESIAN_POINT('Ctrl Pts',(2.1,0.402774227945242,6.53965891057542));
#23582=CARTESIAN_POINT('Ctrl Pts',(2.1,0.398484638758285,6.55741240483299));
#23583=CARTESIAN_POINT('Ctrl Pts',(2.1,0.393037299189535,6.57484669319261));
#23584=CARTESIAN_POINT('Ctrl Pts',(2.1,0.386509552509357,6.59187123411703));
#23585=CARTESIAN_POINT('Ctrl Pts',(2.1,0.381753507363848,6.60427512924121));
#23586=CARTESIAN_POINT('Ctrl Pts',(2.1,0.376423475271725,6.61646161573661));
#23587=CARTESIAN_POINT('Ctrl Pts',(2.1,0.370542725187782,6.62839523023791));
#23588=CARTESIAN_POINT('Ctrl Pts',(2.1,0.367213725298235,6.63515066122709));
#23589=CARTESIAN_POINT('Ctrl Pts',(2.1,0.363707525435473,6.6418256648993));
#23590=CARTESIAN_POINT('Ctrl Pts',(2.1,0.360036351586671,6.64839942538541));
#23591=CARTESIAN_POINT('Ctrl Pts',(2.1,0.35176296808893,6.66321409877431));
#23592=CARTESIAN_POINT('Ctrl Pts',(2.1,0.342644371178579,6.67753242868165));
#23593=CARTESIAN_POINT('Ctrl Pts',(2.1,0.332730966942087,6.69128302674014));
#23594=CARTESIAN_POINT('Ctrl Pts',(2.1,0.326097681493147,6.70048386631449));
#23595=CARTESIAN_POINT('Ctrl Pts',(2.1,0.319108257560132,6.70943048957354));
#23596=CARTESIAN_POINT('Ctrl Pts',(2.1,0.311774677324918,6.7181003705903));
#23597=CARTESIAN_POINT('Ctrl Pts',(2.1,0.308148267079993,6.7223875733389));
#23598=CARTESIAN_POINT('Ctrl Pts',(2.1,0.304437253383367,6.7266073471557));
#23599=CARTESIAN_POINT('Ctrl Pts',(2.1,0.30065086413981,6.73074867775903));
#23600=CARTESIAN_POINT('Ctrl Pts',(2.1,0.284450150446919,6.74846806873983));
#23601=CARTESIAN_POINT('Ctrl Pts',(2.1,0.26684239953173,6.76479115222895));
#23602=CARTESIAN_POINT('Ctrl Pts',(2.1,0.24806300232608,6.77963444611442));
#23603=CARTESIAN_POINT('Ctrl Pts',(2.1,0.229015002355758,6.79469004445943));
#23604=CARTESIAN_POINT('Ctrl Pts',(2.1,0.208760629118366,6.80822418203225));
#23605=CARTESIAN_POINT('Ctrl Pts',(2.1,0.187501868003905,6.82011881527523));
#23606=CARTESIAN_POINT('Ctrl Pts',(2.1,0.182121127272195,6.8231294299218));
#23607=CARTESIAN_POINT('Ctrl Pts',(2.1,0.176675868974013,6.82603481851803));
#23608=CARTESIAN_POINT('Ctrl Pts',(2.1,0.171169051786272,6.82883264150109));
#23609=CARTESIAN_POINT('Ctrl Pts',(2.1,0.165595855256536,6.83166418952754));
#23610=CARTESIAN_POINT('Ctrl Pts',(2.1,0.159966248284264,6.83438207494035));
#23611=CARTESIAN_POINT('Ctrl Pts',(2.1,0.154290568068188,6.83698163141168));
#23612=CARTESIAN_POINT('Ctrl Pts',(2.1,0.139973144289019,6.84353925097815));
#23613=CARTESIAN_POINT('Ctrl Pts',(2.1,0.1253500812197,6.84935087179354));
#23614=CARTESIAN_POINT('Ctrl Pts',(2.1,0.110478871969928,6.85439100862466));
#23615=CARTESIAN_POINT('Ctrl Pts',(2.1,0.091606231881728,6.86078730678786));
#23616=CARTESIAN_POINT('Ctrl Pts',(2.1,0.0723341026865624,6.8659419398207));
#23617=CARTESIAN_POINT('Ctrl Pts',(2.1,0.0527866493565085,6.86986556285165));
#23618=CARTESIAN_POINT('Ctrl Pts',(2.1,0.0364584381349322,6.87314301002196));
#23619=CARTESIAN_POINT('Ctrl Pts',(2.1,0.0199377431301133,6.87556121981262));
#23620=CARTESIAN_POINT('Ctrl Pts',(2.1,0.00329277923049777,6.87711561177094));
#23621=CARTESIAN_POINT('Ctrl Pts',(2.1,-0.00380833581134274,6.87777875025432));
#23622=CARTESIAN_POINT('Ctrl Pts',(2.1,-0.010934154274537,6.87828439261757));
#23623=CARTESIAN_POINT('Ctrl Pts',(2.1,-0.0180564268157742,6.87863124049195));
#23624=CARTESIAN_POINT('Ctrl Pts',(2.1,-0.0436614570733077,6.87987818102488));
#23625=CARTESIAN_POINT('Ctrl Pts',(2.1,-0.0692830486968658,6.87908401838085));
#23626=CARTESIAN_POINT('Ctrl Pts',(2.1,-0.0946701039420577,6.87627112264398));
#23627=CARTESIAN_POINT('Ctrl Pts',(2.1,-0.105116630998588,6.87511364332475));
#23628=CARTESIAN_POINT('Ctrl Pts',(2.1,-0.115523671677657,6.87361376587106));
#23629=CARTESIAN_POINT('Ctrl Pts',(2.1,-0.125874323021446,6.87177056809269));
#23630=CARTESIAN_POINT('Ctrl Pts',(2.1,-0.138413824297786,6.86953758969098));
#23631=CARTESIAN_POINT('Ctrl Pts',(2.1,-0.150870601134534,6.86680082502239));
#23632=CARTESIAN_POINT('Ctrl Pts',(2.1,-0.163219456840939,6.86357425405869));
#23633=CARTESIAN_POINT('Ctrl Pts',(2.1,-0.170695776276485,6.8616208038136));
#23634=CARTESIAN_POINT('Ctrl Pts',(2.1,-0.178132534318461,6.85948775559199));
#23635=CARTESIAN_POINT('Ctrl Pts',(2.1,-0.185524032856684,6.85717764382782));
#23636=CARTESIAN_POINT('Ctrl Pts',(2.1,-0.191333634449564,6.85536193231609));
#23637=CARTESIAN_POINT('Ctrl Pts',(2.1,-0.197115271577026,6.85343663586951));
#23638=CARTESIAN_POINT('Ctrl Pts',(2.1,-0.202852164838079,6.85140831852427));
#23639=CARTESIAN_POINT('Ctrl Pts',(2.1,-0.227408324506361,6.84272632248192));
#23640=CARTESIAN_POINT('Ctrl Pts',(2.1,-0.251209399850707,6.83214163505072));
#23641=CARTESIAN_POINT('Ctrl Pts',(2.1,-0.274050638756253,6.81980030995607));
#23642=CARTESIAN_POINT('Ctrl Pts',(2.1,-0.297081928279728,6.80735629881755));
#23643=CARTESIAN_POINT('Ctrl Pts',(2.1,-0.319138676313367,6.79312590368834));
#23644=CARTESIAN_POINT('Ctrl Pts',(2.1,-0.33999937244817,6.77720843590635));
#23645=CARTESIAN_POINT('Ctrl Pts',(2.1,-0.343569976374306,6.77448393560256));
#23646=CARTESIAN_POINT('Ctrl Pts',(2.1,-0.347105483833496,6.77170989850117));
#23647=CARTESIAN_POINT('Ctrl Pts',(2.1,-0.350604705166974,6.76888668926355));
#23648=CARTESIAN_POINT('Ctrl Pts',(2.1,-0.353884815611532,6.76624026103711));
#23649=CARTESIAN_POINT('Ctrl Pts',(2.1,-0.357133041678995,6.76355062538503));
#23650=CARTESIAN_POINT('Ctrl Pts',(2.1,-0.360348823959175,6.76081852140068));
#23651=CARTESIAN_POINT('Ctrl Pts',(2.46703183294109,-0.426306423912841,
6.39998913682467));
#23652=CARTESIAN_POINT('Ctrl Pts',(2.46387625438919,-0.426248106936643,
6.45633454115753));
#23653=CARTESIAN_POINT('Ctrl Pts',(2.46072067583729,-0.415012427400236,
6.51270250838063));
#23654=CARTESIAN_POINT('Ctrl Pts',(2.45756509728538,-0.39325469889476,6.56466465519153));
#23655=CARTESIAN_POINT('Ctrl Pts',(2.45359215175999,-0.365861221379708,
6.63008618574973));
#23656=CARTESIAN_POINT('Ctrl Pts',(2.4496192062346,-0.321788838359503,6.68852388050336));
#23657=CARTESIAN_POINT('Ctrl Pts',(2.4456462607092,-0.266417048735948,6.73284480312799));
#23658=CARTESIAN_POINT('Ctrl Pts',(2.44167331518381,-0.211045259112394,
6.77716572575262));
#23659=CARTESIAN_POINT('Ctrl Pts',(2.43770036965842,-0.144374062885491,
6.80736987624826));
#23660=CARTESIAN_POINT('Ctrl Pts',(2.43372742413302,-0.0745413820730864,
6.8197705196968));
#23661=CARTESIAN_POINT('Ctrl Pts',(2.42975447860763,-0.00470870126068151,
6.83217116314535));
#23662=CARTESIAN_POINT('Ctrl Pts',(2.42578153308224,0.0682854641372245,
6.82676829954679));
#23663=CARTESIAN_POINT('Ctrl Pts',(2.42180858755684,0.135531407000747,6.80422140536676));
#23664=CARTESIAN_POINT('Ctrl Pts',(2.41783564203145,0.202777349864269,6.78167451118673));
#23665=CARTESIAN_POINT('Ctrl Pts',(2.41386269650606,0.264275070193409,6.74198358642523));
#23666=CARTESIAN_POINT('Ctrl Pts',(2.40988975098066,0.312518123176517,6.68999332669579));
#23667=CARTESIAN_POINT('Ctrl Pts',(2.40591680545527,0.360761176159625,6.63800306696635));
#23668=CARTESIAN_POINT('Ctrl Pts',(2.40194385992988,0.395749561796702,6.57371347226898));
#23669=CARTESIAN_POINT('Ctrl Pts',(2.39797091440449,0.413212578910154,6.50497176512118));
#23670=CARTESIAN_POINT('Ctrl Pts',(2.39399796887909,0.430675596023606,6.43623005797338));
#23671=CARTESIAN_POINT('Ctrl Pts',(2.3900250233537,0.430613244613433,6.36303623837515));
#23672=CARTESIAN_POINT('Ctrl Pts',(2.38605207782831,0.413033135329271,6.29432438331576));
#23673=CARTESIAN_POINT('Ctrl Pts',(2.38207913230291,0.395453026045109,6.22561252825636));
#23674=CARTESIAN_POINT('Ctrl Pts',(2.37810618677752,0.360355158886957,6.16138263773582));
#23675=CARTESIAN_POINT('Ctrl Pts',(2.37413324125213,0.312023598397992,6.10947464674327));
#23676=CARTESIAN_POINT('Ctrl Pts',(2.37016029572673,0.263692037909028,6.05756665575072));
#23677=CARTESIAN_POINT('Ctrl Pts',(2.36618735020134,0.20212678408925,6.01798056428618));
#23678=CARTESIAN_POINT('Ctrl Pts',(2.36221440467595,0.1348425249389,5.99554827196608));
#23679=CARTESIAN_POINT('Ctrl Pts',(2.35824145915055,0.0675582657885491,
5.97311597964598));
#23680=CARTESIAN_POINT('Ctrl Pts',(2.35426851362516,-0.00544499869237483,
5.96783748647033));
#23681=CARTESIAN_POINT('Ctrl Pts',(2.35029556809977,-0.0752564507749232,
5.98035708815828));
#23682=CARTESIAN_POINT('Ctrl Pts',(2.34632262257437,-0.145067902857471,
5.99287668984623));
#23683=CARTESIAN_POINT('Ctrl Pts',(2.34234967704898,-0.211687542541645,
6.02319438639778));
#23684=CARTESIAN_POINT('Ctrl Pts',(2.33837673152359,-0.266983740765077,
6.06760958345802));
#23685=CARTESIAN_POINT('Ctrl Pts',(2.33440378599819,-0.322279938988509,
6.11202478051826));
#23686=CARTESIAN_POINT('Ctrl Pts',(2.3304308404728,-0.366252695751201,6.17053747808719));
#23687=CARTESIAN_POINT('Ctrl Pts',(2.32645789494741,-0.393534672723127,
6.236005584836));
#23688=CARTESIAN_POINT('Ctrl Pts',(2.32331587427864,-0.415110738889366,
6.28778131224916));
#23689=CARTESIAN_POINT('Ctrl Pts',(2.32017385360987,-0.4262475506417,6.34390730291496));
#23690=CARTESIAN_POINT('Ctrl Pts',(2.31703183294109,-0.426305653513777,
6.40001091236462));
#23691=CARTESIAN_POINT('Ctrl Pts',(2.6,-0.132288496556895,5.90755938055567));
#23692=CARTESIAN_POINT('Ctrl Pts',(2.6,-0.157089924837099,5.91642640455182));
#23693=CARTESIAN_POINT('Ctrl Pts',(2.6,-0.181088073064976,5.9272189255245));
#23694=CARTESIAN_POINT('Ctrl Pts',(2.6,-0.204091900162786,5.93978802247808));
#23695=CARTESIAN_POINT('Ctrl Pts',(2.6,-0.226981614101412,5.95229476896469));
#23696=CARTESIAN_POINT('Ctrl Pts',(2.6,-0.248887897831876,5.96656143458844));
#23697=CARTESIAN_POINT('Ctrl Pts',(2.6,-0.269590200964406,5.98248076289354));
#23698=CARTESIAN_POINT('Ctrl Pts',(2.6,-0.276528918772376,5.98781638792494));
#23699=CARTESIAN_POINT('Ctrl Pts',(2.6,-0.283332046569503,5.99333793609881));
#23700=CARTESIAN_POINT('Ctrl Pts',(2.6,-0.289990147837974,5.99904209573216));
#23701=CARTESIAN_POINT('Ctrl Pts',(2.6,-0.296028106433828,6.00421496383698));
#23702=CARTESIAN_POINT('Ctrl Pts',(2.6,-0.301949771037903,6.00954116989861));
#23703=CARTESIAN_POINT('Ctrl Pts',(2.6,-0.307727671725424,6.01499858003089));
#23704=CARTESIAN_POINT('Ctrl Pts',(2.6,-0.318182122624537,6.02487313990129));
#23705=CARTESIAN_POINT('Ctrl Pts',(2.6,-0.32817930410564,6.03518740593773));
#23706=CARTESIAN_POINT('Ctrl Pts',(2.6,-0.337684947200095,6.04592058651842));
#23707=CARTESIAN_POINT('Ctrl Pts',(2.6,-0.35463663907465,6.06506138196275));
#23708=CARTESIAN_POINT('Ctrl Pts',(2.6,-0.370027957593029,6.08553349763026));
#23709=CARTESIAN_POINT('Ctrl Pts',(2.6,-0.383735216002276,6.10712564152075));
#23710=CARTESIAN_POINT('Ctrl Pts',(2.6,-0.39189872132373,6.11998507528124));
#23711=CARTESIAN_POINT('Ctrl Pts',(2.6,-0.399464029634324,6.13324224816933));
#23712=CARTESIAN_POINT('Ctrl Pts',(2.6,-0.406396423774992,6.1468545793287));
#23713=CARTESIAN_POINT('Ctrl Pts',(2.6,-0.409857954474058,6.15365158210118));
#23714=CARTESIAN_POINT('Ctrl Pts',(2.6,-0.413162930739684,6.16054073803517));
#23715=CARTESIAN_POINT('Ctrl Pts',(2.6,-0.416296070484027,6.16749212337976));
#23716=CARTESIAN_POINT('Ctrl Pts',(2.6,-0.426533299061843,6.19020509710957));
#23717=CARTESIAN_POINT('Ctrl Pts',(2.6,-0.434966161858725,6.21362881910558));
#23718=CARTESIAN_POINT('Ctrl Pts',(2.6,-0.441477406647537,6.23756556523482));
#23719=CARTESIAN_POINT('Ctrl Pts',(2.6,-0.443239379224161,6.24404295805621));
#23720=CARTESIAN_POINT('Ctrl Pts',(2.6,-0.444860350146518,6.25055797543335));
#23721=CARTESIAN_POINT('Ctrl Pts',(2.6,-0.44633733619218,6.25710677385474));
#23722=CARTESIAN_POINT('Ctrl Pts',(2.6,-0.450544524902758,6.27576099937518));
#23723=CARTESIAN_POINT('Ctrl Pts',(2.6,-0.453584703119787,6.29468965910361));
#23724=CARTESIAN_POINT('Ctrl Pts',(2.6,-0.455444326288054,6.31378084410223));
#23725=CARTESIAN_POINT('Ctrl Pts',(2.6,-0.456025440853221,6.31974665796081));
#23726=CARTESIAN_POINT('Ctrl Pts',(2.6,-0.456491144811005,6.32572830613997));
#23727=CARTESIAN_POINT('Ctrl Pts',(2.6,-0.456840676091559,6.33172224529114));
#23728=CARTESIAN_POINT('Ctrl Pts',(2.6,-0.457162778165346,6.33724581453417));
#23729=CARTESIAN_POINT('Ctrl Pts',(2.6,-0.457385661676131,6.34277019876787));
#23730=CARTESIAN_POINT('Ctrl Pts',(2.6,-0.457509644065614,6.34829248285953));
#23731=CARTESIAN_POINT('Ctrl Pts',(2.6,-0.458052816417877,6.37248585461552));
#23732=CARTESIAN_POINT('Ctrl Pts',(2.6,-0.456701759624391,6.39664121290135));
#23733=CARTESIAN_POINT('Ctrl Pts',(2.6,-0.453453339531317,6.42053138158929));
#23734=CARTESIAN_POINT('Ctrl Pts',(2.6,-0.450523324248874,6.44207987511851));
#23735=CARTESIAN_POINT('Ctrl Pts',(2.6,-0.446048919178311,6.46341331208366));
#23736=CARTESIAN_POINT('Ctrl Pts',(2.6,-0.439994176553064,6.48435098741415));
#23737=CARTESIAN_POINT('Ctrl Pts',(2.6,-0.438094472520504,6.49092028172105));
#23738=CARTESIAN_POINT('Ctrl Pts',(2.6,-0.436038962655861,6.4974504658391));
#23739=CARTESIAN_POINT('Ctrl Pts',(2.6,-0.43382941905493,6.50393615250028));
#23740=CARTESIAN_POINT('Ctrl Pts',(2.6,-0.431714290768034,6.5101447013206));
#23741=CARTESIAN_POINT('Ctrl Pts',(2.6,-0.42946061872238,6.5163046335942));
#23742=CARTESIAN_POINT('Ctrl Pts',(2.6,-0.427072414698455,6.5224077707279));
#23743=CARTESIAN_POINT('Ctrl Pts',(2.6,-0.421492488317325,6.53666746360122));
#23744=CARTESIAN_POINT('Ctrl Pts',(2.6,-0.415176231857449,6.5506245268354));
#23745=CARTESIAN_POINT('Ctrl Pts',(2.6,-0.408152204549093,6.56422236660796));
#23746=CARTESIAN_POINT('Ctrl Pts',(2.6,-0.402591346359437,6.57498765201209));
#23747=CARTESIAN_POINT('Ctrl Pts',(2.6,-0.396586710322636,6.58552771963742));
#23748=CARTESIAN_POINT('Ctrl Pts',(2.6,-0.390149689096489,6.59581166017504));
#23749=CARTESIAN_POINT('Ctrl Pts',(2.6,-0.386403333843806,6.6017969277853));
#23750=CARTESIAN_POINT('Ctrl Pts',(2.6,-0.382511806820547,6.60769294534655));
#23751=CARTESIAN_POINT('Ctrl Pts',(2.6,-0.378483683496843,6.61348517016826));
#23752=CARTESIAN_POINT('Ctrl Pts',(2.6,-0.365269544048599,6.63248639241469));
#23753=CARTESIAN_POINT('Ctrl Pts',(2.6,-0.350570496167934,6.65040177272496));
#23754=CARTESIAN_POINT('Ctrl Pts',(2.6,-0.334470605331163,6.66701291851188));
#23755=CARTESIAN_POINT('Ctrl Pts',(2.6,-0.332980284132811,6.66855056512987));
#23756=CARTESIAN_POINT('Ctrl Pts',(2.6,-0.331477939680677,6.67007700481367));
#23757=CARTESIAN_POINT('Ctrl Pts',(2.6,-0.329963627179693,6.67159204424712));
#23758=CARTESIAN_POINT('Ctrl Pts',(2.6,-0.327462974104075,6.67409389773937));
#23759=CARTESIAN_POINT('Ctrl Pts',(2.6,-0.324929685151723,6.67656466471947));
#23760=CARTESIAN_POINT('Ctrl Pts',(2.6,-0.322364416527274,6.67900379523474));
#23761=CARTESIAN_POINT('Origin',(-2.93123464956316,0.,6.4));
#23762=CARTESIAN_POINT('Ctrl Pts',(-2.55623464956316,0.509888470297935,
6.40001295625876));
#23763=CARTESIAN_POINT('Ctrl Pts',(-2.55512836300704,0.509911167721204,
6.42364295379955));
#23764=CARTESIAN_POINT('Ctrl Pts',(-2.55004913092554,0.502507177574701,
6.53211994282295));
#23765=CARTESIAN_POINT('Ctrl Pts',(-2.54099695331864,0.426919346618493,
6.7167170754366));
#23766=CARTESIAN_POINT('Ctrl Pts',(-2.52907811674246,0.223174193283009,
6.88245524211623));
#23767=CARTESIAN_POINT('Ctrl Pts',(-2.51715928016628,-0.0350524704178637,
6.93041600240246));
#23768=CARTESIAN_POINT('Ctrl Pts',(-2.5052404435901,-0.284722093726431,
6.84889099741939));
#23769=CARTESIAN_POINT('Ctrl Pts',(-2.49332160701392,-0.464885050226796,
6.6577822578485));
#23770=CARTESIAN_POINT('Ctrl Pts',(-2.48140277043774,-0.531559769507257,
6.40374342750432));
#23771=CARTESIAN_POINT('Ctrl Pts',(-2.46948393386156,-0.468469545343797,
6.14879075163119));
#23772=CARTESIAN_POINT('Ctrl Pts',(-2.45756509728538,-0.291016032073294,
5.95516354586177));
#23773=CARTESIAN_POINT('Ctrl Pts',(-2.4456462607092,-0.0425193718295788,
5.87013029471448));
#23774=CARTESIAN_POINT('Ctrl Pts',(-2.43372742413302,0.216357163144678,
5.91444940567057));
#23775=CARTESIAN_POINT('Ctrl Pts',(-2.42180858755684,0.422416354717456,
6.07730165027367));
#23776=CARTESIAN_POINT('Ctrl Pts',(-2.41264432936689,0.501564565860727,
6.26308799447805));
#23777=CARTESIAN_POINT('Ctrl Pts',(-2.40745301670233,0.50990474610345,6.37396275616984));
#23778=CARTESIAN_POINT('Ctrl Pts',(-2.40623464956316,0.509881639433629,
6.39998778127036));
#23779=CARTESIAN_POINT('Ctrl Pts',(-2.56876535043684,0.509867809550215,
6.40001069114481));
#23780=CARTESIAN_POINT('Ctrl Pts',(-2.56725806371505,0.509887058630054,
6.4322090151272));
#23781=CARTESIAN_POINT('Ctrl Pts',(-2.56177783146786,0.498968432159698,
6.54926324266892));
#23782=CARTESIAN_POINT('Ctrl Pts',(-2.55232465369528,0.410425773087965,
6.73782039475945));
#23783=CARTESIAN_POINT('Ctrl Pts',(-2.54040581711911,0.19858907062663,6.89308342832313));
#23784=CARTESIAN_POINT('Ctrl Pts',(-2.52848698054292,-0.0617246536500735,
6.92797742227401));
#23785=CARTESIAN_POINT('Ctrl Pts',(-2.51656814396674,-0.306971377021502,
6.8339796336226));
#23786=CARTESIAN_POINT('Ctrl Pts',(-2.50464930739056,-0.477279320739804,
6.63403891232169));
#23787=CARTESIAN_POINT('Ctrl Pts',(-2.49273047081439,-0.531073600862929,
6.3769640630774));
#23788=CARTESIAN_POINT('Ctrl Pts',(-2.48081163423821,-0.455221493256117,
6.12551290982166));
#23789=CARTESIAN_POINT('Ctrl Pts',(-2.46889279766203,-0.268240284898955,
5.94106977614238));
#23790=CARTESIAN_POINT('Ctrl Pts',(-2.45697396108585,-0.0157759417689948,
5.86866121228054));
#23791=CARTESIAN_POINT('Ctrl Pts',(-2.44505512450967,0.240539628301038,
5.92596363104932));
#23792=CARTESIAN_POINT('Ctrl Pts',(-2.43313628793349,0.438134411540293,
6.09898832463164));
#23793=CARTESIAN_POINT('Ctrl Pts',(-2.42437302990921,0.504774712912163,
6.28023194354175));
#23794=CARTESIAN_POINT('Ctrl Pts',(-2.41958271741033,0.509925751376541,
6.3825301408573));
#23795=CARTESIAN_POINT('Ctrl Pts',(-2.41876535043684,0.509907683680876,
6.3999870064905));
#23796=CARTESIAN_POINT('Ctrl Pts',(-2.6,-0.322335278395778,6.67898325810255));
#23797=CARTESIAN_POINT('Ctrl Pts',(-2.59602705447461,-0.368763212726337,
6.62534075195518));
#23798=CARTESIAN_POINT('Ctrl Pts',(-2.58808116342382,-0.434258099467944,
6.4944682619995));
#23799=CARTESIAN_POINT('Ctrl Pts',(-2.57616232684764,-0.426482264300449,
6.27500430516079));
#23800=CARTESIAN_POINT('Ctrl Pts',(-2.56424349027146,-0.314584469477882,
6.08608472387891));
#23801=CARTESIAN_POINT('Ctrl Pts',(-2.55232465369528,-0.125891708691813,
5.97378227942249));
#23802=CARTESIAN_POINT('Ctrl Pts',(-2.5404058171191,0.0935351747046863,
5.96553560214966));
#23803=CARTESIAN_POINT('Ctrl Pts',(-2.52848698054292,0.290127651295543,
6.06334746928321));
#23804=CARTESIAN_POINT('Ctrl Pts',(-2.51656814396674,0.415894108139653,
6.24334485866553));
#23805=CARTESIAN_POINT('Ctrl Pts',(-2.50464930739057,0.440131934448267,
6.46158434769009));
#23806=CARTESIAN_POINT('Ctrl Pts',(-2.49273047081439,0.356924333130935,
6.66479013386668));
#23807=CARTESIAN_POINT('Ctrl Pts',(-2.48081163423821,0.186583954886344,
6.80335491216739));
#23808=CARTESIAN_POINT('Ctrl Pts',(-2.46889279766203,-0.0293054876233287,
6.8434523275626));
#23809=CARTESIAN_POINT('Ctrl Pts',(-2.45697396108585,-0.238040848314528,
6.77529365012726));
#23810=CARTESIAN_POINT('Ctrl Pts',(-2.44505512450967,-0.388665418536347,
6.61551789864839));
#23811=CARTESIAN_POINT('Ctrl Pts',(-2.43313628793349,-0.444408569799851,
6.40312967865285));
#23812=CARTESIAN_POINT('Ctrl Pts',(-2.42121745135731,-0.391662222357444,
6.18997744149907));
#23813=CARTESIAN_POINT('Ctrl Pts',(-2.40929861478113,-0.243302872078535,
6.0280961357146));
#23814=CARTESIAN_POINT('Ctrl Pts',(-2.39737977820495,-0.0355481627984888,
5.95700440211175));
#23815=CARTESIAN_POINT('Ctrl Pts',(-2.38546094162877,0.180884602174105,
5.99405723011839));
#23816=CARTESIAN_POINT('Ctrl Pts',(-2.37354210505259,0.353159623487059,
6.13020924399229));
#23817=CARTESIAN_POINT('Ctrl Pts',(-2.36162326847641,0.439220937561425,
6.33222286740014));
#23818=CARTESIAN_POINT('Ctrl Pts',(-2.34970443190023,0.418059163834771,
6.55078231736932));
#23819=CARTESIAN_POINT('Ctrl Pts',(-2.33778559532405,0.29484033726761,6.73253262578912));
#23820=CARTESIAN_POINT('Ctrl Pts',(-2.32586675874787,0.099644770368915,
6.83310471186003));
#23821=CARTESIAN_POINT('Ctrl Pts',(-2.3139479221717,-0.119876185075048,
6.82794680971604));
#23822=CARTESIAN_POINT('Ctrl Pts',(-2.30202908559551,-0.310132837249173,
6.71831807199288));
#23823=CARTESIAN_POINT('Ctrl Pts',(-2.29011024901934,-0.424679527547163,
6.53098118406136));
#23824=CARTESIAN_POINT('Ctrl Pts',(-2.27819141244315,-0.435552994685514,
6.31166902859576));
#23825=CARTESIAN_POINT('Ctrl Pts',(-2.26627257586698,-0.340098796199685,
6.11392032482827));
#23826=CARTESIAN_POINT('Ctrl Pts',(-2.2543537392908,-0.16161931364965,5.98600969928979));
#23827=CARTESIAN_POINT('Ctrl Pts',(-2.24243490271462,0.0563148495252739,
5.95916283101918));
#23828=CARTESIAN_POINT('Ctrl Pts',(-2.23051606613844,0.260501371261513,
6.03993360741091));
#23829=CARTESIAN_POINT('Ctrl Pts',(-2.21859722956226,0.401094017530737,
6.20860417742001));
#23830=CARTESIAN_POINT('Ctrl Pts',(-2.20667839298608,0.44377116171621,6.42399850480546));
#23831=CARTESIAN_POINT('Ctrl Pts',(-2.1947595564099,0.378114410354912,6.63353428436548));
#23832=CARTESIAN_POINT('Ctrl Pts',(-2.18284071983372,0.220151966921295,
6.78605943828148));
#23833=CARTESIAN_POINT('Ctrl Pts',(-2.17092188325754,0.00844577862671016,
6.84433931427905));
#23834=CARTESIAN_POINT('Ctrl Pts',(-2.15900304668136,-0.205322181057602,
6.79414666881739));
#23835=CARTESIAN_POINT('Ctrl Pts',(-2.14708421010518,-0.368966714730599,
6.64773436383049));
#23836=CARTESIAN_POINT('Ctrl Pts',(-2.135165373529,-0.442538599255273,6.44084520364718));
#23837=CARTESIAN_POINT('Ctrl Pts',(-2.12324653695282,-0.408077698331108,
6.22398416943617));
#23838=CARTESIAN_POINT('Ctrl Pts',(-2.11132770037664,-0.273995984823229,
6.05009380941852));
#23839=CARTESIAN_POINT('Ctrl Pts',(-2.09940886380046,-0.0730271011145798,
5.96161967407919));
#23840=CARTESIAN_POINT('Ctrl Pts',(-2.08749002722429,0.145771140848075,
5.98017031606292));
#23841=CARTESIAN_POINT('Ctrl Pts',(-2.07557119064811,0.328978055262558,
6.10119490525287));
#23842=CARTESIAN_POINT('Ctrl Pts',(-2.06365235407193,0.431879950098104,
6.29519514237415));
#23843=CARTESIAN_POINT('Ctrl Pts',(-2.05570646302114,0.430162668703658,
6.44153119316515));
#23844=CARTESIAN_POINT('Ctrl Pts',(-2.05173351749575,0.411845039474987,
6.51006976632957));
#23845=CARTESIAN_POINT('Ctrl Pts',(-2.61608882750142,-0.34340590883904,
6.69722002436839));
#23846=CARTESIAN_POINT('Ctrl Pts',(-2.61211588197602,-0.392868775775771,
6.64007097860578));
#23847=CARTESIAN_POINT('Ctrl Pts',(-2.60416999092524,-0.462644976561947,
6.5006435272299));
#23848=CARTESIAN_POINT('Ctrl Pts',(-2.59225115434906,-0.454360845343155,
6.26683350205768));
#23849=CARTESIAN_POINT('Ctrl Pts',(-2.58033231777288,-0.335148439802654,
6.065564497838));
#23850=CARTESIAN_POINT('Ctrl Pts',(-2.5684134811967,-0.134121083034322,
5.94592099125275));
#23851=CARTESIAN_POINT('Ctrl Pts',(-2.55649464462052,0.0996494452538391,
5.9371352396035));
#23852=CARTESIAN_POINT('Ctrl Pts',(-2.54457580804434,0.309092911791522,
6.04134093900881));
#23853=CARTESIAN_POINT('Ctrl Pts',(-2.53265697146816,0.443080555430665,
6.23310451945562));
#23854=CARTESIAN_POINT('Ctrl Pts',(-2.52073813489198,0.468902776359187,
6.46561003497361));
#23855=CARTESIAN_POINT('Ctrl Pts',(-2.5088192983158,0.380256004293454,6.68209911438999));
#23856=CARTESIAN_POINT('Ctrl Pts',(-2.49690046173962,0.198780701018566,
6.829721688817));
#23857=CARTESIAN_POINT('Ctrl Pts',(-2.48498162516344,-0.0312211485548406,
6.87244021917589));
#23858=CARTESIAN_POINT('Ctrl Pts',(-2.47306278858727,-0.253601263451829,
6.79982609922463));
#23859=CARTESIAN_POINT('Ctrl Pts',(-2.46114395201108,-0.414071962433164,
6.62960601838176));
#23860=CARTESIAN_POINT('Ctrl Pts',(-2.44922511543491,-0.473458969702319,
6.40333426160334));
#23861=CARTESIAN_POINT('Ctrl Pts',(-2.43730627885873,-0.417264663352895,
6.17624854487645));
#23862=CARTESIAN_POINT('Ctrl Pts',(-2.42538744228255,-0.259207258743454,
6.00378527243032));
#23863=CARTESIAN_POINT('Ctrl Pts',(-2.41346860570637,-0.0378718991421855,
5.92804636631267));
#23864=CARTESIAN_POINT('Ctrl Pts',(-2.40154976913019,0.192708789164296,
5.96752128863578));
#23865=CARTESIAN_POINT('Ctrl Pts',(-2.38963093255401,0.376245200563858,
6.11257337941941));
#23866=CARTESIAN_POINT('Ctrl Pts',(-2.37771209597783,0.467932228811824,
6.32779236596503));
#23867=CARTESIAN_POINT('Ctrl Pts',(-2.36579325940165,0.445387137950485,
6.56063875785105));
#23868=CARTESIAN_POINT('Ctrl Pts',(-2.35387442282547,0.314113659806958,
6.75426984333229));
#23869=CARTESIAN_POINT('Ctrl Pts',(-2.34195558624929,0.106158417098793,
6.86141619353295));
#23870=CARTESIAN_POINT('Ctrl Pts',(-2.33003674967311,-0.127712332602043,
6.85592112615381));
#23871=CARTESIAN_POINT('Ctrl Pts',(-2.31811791309693,-0.330405810268198,
6.73912610297154));
#23872=CARTESIAN_POINT('Ctrl Pts',(-2.30619907652075,-0.452440266074759,
6.53954325067136));
#23873=CARTESIAN_POINT('Ctrl Pts',(-2.29428023994457,-0.464024517365714,
6.30589494992706));
#23874=CARTESIAN_POINT('Ctrl Pts',(-2.28236140336839,-0.362330604286552,
6.09521967517282));
#23875=CARTESIAN_POINT('Ctrl Pts',(-2.27044256679221,-0.172184154232268,
5.95894770137019));
#23876=CARTESIAN_POINT('Ctrl Pts',(-2.25852373021603,0.0599960766894875,
5.93034588886046));
#23877=CARTESIAN_POINT('Ctrl Pts',(-2.24660489363985,0.277530001050755,
6.01639654398105));
#23878=CARTESIAN_POINT('Ctrl Pts',(-2.23468605706368,0.427313002490913,
6.19609288586657));
#23879=CARTESIAN_POINT('Ctrl Pts',(-2.2227672204875,0.472779895096048,6.42556725529552));
#23880=CARTESIAN_POINT('Ctrl Pts',(-2.21084838391132,0.402831248814268,
6.64880011138319));
#23881=CARTESIAN_POINT('Ctrl Pts',(-2.19892954733514,0.234543009563112,
6.81129563269882));
#23882=CARTESIAN_POINT('Ctrl Pts',(-2.18701071075896,0.00899786799506803,
6.8733851870398));
#23883=CARTESIAN_POINT('Ctrl Pts',(-2.17509187418278,-0.218743820229089,
6.81991151478903));
#23884=CARTESIAN_POINT('Ctrl Pts',(-2.1631730376066,-0.393085580436657,
6.66392843124485));
#23885=CARTESIAN_POINT('Ctrl Pts',(-2.15125420103042,-0.471466761658698,
6.44351520053897));
#23886=CARTESIAN_POINT('Ctrl Pts',(-2.13933536445424,-0.43475319726025,
6.2124782476009));
#23887=CARTESIAN_POINT('Ctrl Pts',(-2.12741652787806,-0.291906739636914,
6.02722090494389));
#23888=CARTESIAN_POINT('Ctrl Pts',(-2.11549769130188,-0.0778007860416099,
5.93296333249894));
#23889=CARTESIAN_POINT('Ctrl Pts',(-2.1035788547257,0.155300007354369,5.95272660539192));
#23890=CARTESIAN_POINT('Ctrl Pts',(-2.09166001814952,0.350482915235934,
6.08166241176561));
#23891=CARTESIAN_POINT('Ctrl Pts',(-2.07974118157334,0.46011137071598,6.28834418757117));
#23892=CARTESIAN_POINT('Ctrl Pts',(-2.07179529052256,0.458281832910106,
6.44424603228361));
#23893=CARTESIAN_POINT('Ctrl Pts',(-2.06782234499716,0.438766804507522,
6.51726488124485));
#23894=CARTESIAN_POINT('Ctrl Pts',(-2.63217765500284,-0.364476539282301,
6.71545679063422));
#23895=CARTESIAN_POINT('Ctrl Pts',(-2.62820470947744,-0.416974338825206,
6.65480120525638));
#23896=CARTESIAN_POINT('Ctrl Pts',(-2.62025881842666,-0.49103185365595,
6.5068187924603));
#23897=CARTESIAN_POINT('Ctrl Pts',(-2.60833998185048,-0.482239426385862,
6.25866269895458));
#23898=CARTESIAN_POINT('Ctrl Pts',(-2.5964211452743,-0.355712410127426,
6.04504427179708));
#23899=CARTESIAN_POINT('Ctrl Pts',(-2.58450230869812,-0.142350457376832,
5.91805970308301));
#23900=CARTESIAN_POINT('Ctrl Pts',(-2.57258347212194,0.105763715802992,
5.90873487705734));
#23901=CARTESIAN_POINT('Ctrl Pts',(-2.56066463554576,0.3280581722875,6.01933440873442));
#23902=CARTESIAN_POINT('Ctrl Pts',(-2.54874579896958,0.470267002721677,
6.2228641802457));
#23903=CARTESIAN_POINT('Ctrl Pts',(-2.5368269623934,0.497673618270107,6.46963572225713));
#23904=CARTESIAN_POINT('Ctrl Pts',(-2.52490812581722,0.403587675455974,
6.69940809491329));
#23905=CARTESIAN_POINT('Ctrl Pts',(-2.51298928924104,0.210977447150787,
6.85608846546662));
#23906=CARTESIAN_POINT('Ctrl Pts',(-2.50107045266486,-0.0331368094863519,
6.90142811078917));
#23907=CARTESIAN_POINT('Ctrl Pts',(-2.48915161608868,-0.26916167858913,
6.82435854832202));
#23908=CARTESIAN_POINT('Ctrl Pts',(-2.4772327795125,-0.43947850632998,6.64369413811513));
#23909=CARTESIAN_POINT('Ctrl Pts',(-2.46531394293632,-0.502509369604788,
6.40353884455383));
#23910=CARTESIAN_POINT('Ctrl Pts',(-2.45339510636014,-0.442867104348346,
6.16251964825382));
#23911=CARTESIAN_POINT('Ctrl Pts',(-2.44147626978397,-0.275111645408374,
5.97947440914605));
#23912=CARTESIAN_POINT('Ctrl Pts',(-2.42955743320778,-0.0401956354858822,
5.89908833051357));
#23913=CARTESIAN_POINT('Ctrl Pts',(-2.41763859663161,0.204532976154487,
5.94098534715318));
#23914=CARTESIAN_POINT('Ctrl Pts',(-2.40571976005543,0.399330777640657,
6.09493751484654));
#23915=CARTESIAN_POINT('Ctrl Pts',(-2.39380092347925,0.496643520062223,
6.32336186452993));
#23916=CARTESIAN_POINT('Ctrl Pts',(-2.38188208690307,0.472715112066199,
6.57049519833277));
#23917=CARTESIAN_POINT('Ctrl Pts',(-2.36996325032689,0.333386982346306,
6.77600706087547));
#23918=CARTESIAN_POINT('Ctrl Pts',(-2.35804441375071,0.112672063828671,
6.88972767520587));
#23919=CARTESIAN_POINT('Ctrl Pts',(-2.34612557717453,-0.135548480129038,
6.88389544259157));
#23920=CARTESIAN_POINT('Ctrl Pts',(-2.33420674059835,-0.350678783287223,
6.7599341339502));
#23921=CARTESIAN_POINT('Ctrl Pts',(-2.32228790402217,-0.480201004602356,
6.54810531728136));
#23922=CARTESIAN_POINT('Ctrl Pts',(-2.31036906744599,-0.492496040045916,
6.30012087125837));
#23923=CARTESIAN_POINT('Ctrl Pts',(-2.29845023086981,-0.384562412373419,
6.07651902551736));
#23924=CARTESIAN_POINT('Ctrl Pts',(-2.28653139429363,-0.182748994814887,
5.9318857034506));
#23925=CARTESIAN_POINT('Ctrl Pts',(-2.27461255771745,0.0636773038537012,
5.90152894670173));
#23926=CARTESIAN_POINT('Ctrl Pts',(-2.26269372114127,0.294558630839998,
5.99285948055119));
#23927=CARTESIAN_POINT('Ctrl Pts',(-2.25077488456509,0.453531987451089,
6.18358159431314));
#23928=CARTESIAN_POINT('Ctrl Pts',(-2.23885604798891,0.501788628475886,
6.42713600578558));
#23929=CARTESIAN_POINT('Ctrl Pts',(-2.22693721141274,0.427548087273624,
6.6640659384009));
#23930=CARTESIAN_POINT('Ctrl Pts',(-2.21501837483655,0.24893405220493,6.83653182711616));
#23931=CARTESIAN_POINT('Ctrl Pts',(-2.20309953826038,0.00954995736342605,
6.90243105980056));
#23932=CARTESIAN_POINT('Ctrl Pts',(-2.1911807016842,-0.232165459400577,
6.84567636076067));
#23933=CARTESIAN_POINT('Ctrl Pts',(-2.17926186510802,-0.417204446142715,
6.68012249865921));
#23934=CARTESIAN_POINT('Ctrl Pts',(-2.16734302853184,-0.500394924062124,
6.44618519743075));
#23935=CARTESIAN_POINT('Ctrl Pts',(-2.15542419195566,-0.461428696189393,
6.20097232576562));
#23936=CARTESIAN_POINT('Ctrl Pts',(-2.14350535537948,-0.309817494450599,
6.00434800046925));
#23937=CARTESIAN_POINT('Ctrl Pts',(-2.1315865188033,-0.0825744709686401,
5.90430699091869));
#23938=CARTESIAN_POINT('Ctrl Pts',(-2.11966768222712,0.164828873860662,
5.92528289472092));
#23939=CARTESIAN_POINT('Ctrl Pts',(-2.10774884565094,0.371987775209309,
6.06212991827835));
#23940=CARTESIAN_POINT('Ctrl Pts',(-2.09583000907476,0.488342791333856,
6.2814932327682));
#23941=CARTESIAN_POINT('Ctrl Pts',(-2.08788411802398,0.486400997116553,
6.44696087140208));
#23942=CARTESIAN_POINT('Ctrl Pts',(-2.08391117249858,0.465688569540057,
6.52445999616013));
#23943=CARTESIAN_POINT('Ctrl Pts',(-2.64826648250425,-0.385547169725563,
6.73369355690005));
#23944=CARTESIAN_POINT('Ctrl Pts',(-2.64429353697886,-0.44107990187464,
6.66953143190698));
#23945=CARTESIAN_POINT('Ctrl Pts',(-2.63634764592807,-0.519418730749953,
6.5129940576907));
#23946=CARTESIAN_POINT('Ctrl Pts',(-2.62442880935189,-0.510118007428568,
6.25049189585148));
#23947=CARTESIAN_POINT('Ctrl Pts',(-2.61250997277571,-0.376276380452198,
6.02452404575617));
#23948=CARTESIAN_POINT('Ctrl Pts',(-2.60059113619954,-0.150579831719341,
5.89019841491327));
#23949=CARTESIAN_POINT('Ctrl Pts',(-2.58867229962336,0.111877986352145,
5.88033451451117));
#23950=CARTESIAN_POINT('Ctrl Pts',(-2.57675346304718,0.347023432783479,
5.99732787846002));
#23951=CARTESIAN_POINT('Ctrl Pts',(-2.564834626471,0.497453450012689,6.21262384103579));
#23952=CARTESIAN_POINT('Ctrl Pts',(-2.55291578989482,0.526444460181026,
6.47366140954065));
#23953=CARTESIAN_POINT('Ctrl Pts',(-2.54099695331864,0.426919346618493,
6.7167170754366));
#23954=CARTESIAN_POINT('Ctrl Pts',(-2.52907811674246,0.223174193283009,
6.88245524211623));
#23955=CARTESIAN_POINT('Ctrl Pts',(-2.51715928016628,-0.0350524704178637,
6.93041600240246));
#23956=CARTESIAN_POINT('Ctrl Pts',(-2.5052404435901,-0.284722093726431,
6.84889099741939));
#23957=CARTESIAN_POINT('Ctrl Pts',(-2.49332160701392,-0.464885050226796,
6.6577822578485));
#23958=CARTESIAN_POINT('Ctrl Pts',(-2.48140277043774,-0.531559769507257,
6.40374342750432));
#23959=CARTESIAN_POINT('Ctrl Pts',(-2.46948393386156,-0.468469545343797,
6.14879075163119));
#23960=CARTESIAN_POINT('Ctrl Pts',(-2.45756509728538,-0.291016032073294,
5.95516354586177));
#23961=CARTESIAN_POINT('Ctrl Pts',(-2.4456462607092,-0.0425193718295788,
5.87013029471448));
#23962=CARTESIAN_POINT('Ctrl Pts',(-2.43372742413302,0.216357163144678,
5.91444940567057));
#23963=CARTESIAN_POINT('Ctrl Pts',(-2.42180858755684,0.422416354717456,
6.07730165027367));
#23964=CARTESIAN_POINT('Ctrl Pts',(-2.40988975098066,0.525354811312622,
6.31893136309484));
#23965=CARTESIAN_POINT('Ctrl Pts',(-2.39797091440449,0.500043086181913,
6.58035163881449));
#23966=CARTESIAN_POINT('Ctrl Pts',(-2.38605207782831,0.352660304885654,
6.79774427841866));
#23967=CARTESIAN_POINT('Ctrl Pts',(-2.37413324125213,0.11918571055855,6.91803915687878));
#23968=CARTESIAN_POINT('Ctrl Pts',(-2.36221440467595,-0.143384627656033,
6.91186975902934));
#23969=CARTESIAN_POINT('Ctrl Pts',(-2.35029556809977,-0.370951756306248,
6.78074216492885));
#23970=CARTESIAN_POINT('Ctrl Pts',(-2.33837673152359,-0.507961743129952,
6.55666738389136));
#23971=CARTESIAN_POINT('Ctrl Pts',(-2.32645789494741,-0.520967562726117,
6.29434679258967));
#23972=CARTESIAN_POINT('Ctrl Pts',(-2.31453905837123,-0.406794220460285,
6.05781837586191));
#23973=CARTESIAN_POINT('Ctrl Pts',(-2.30262022179505,-0.193313835397505,
5.904823705531));
#23974=CARTESIAN_POINT('Ctrl Pts',(-2.29070138521887,0.067358531017915,
5.872712004543));
#23975=CARTESIAN_POINT('Ctrl Pts',(-2.27878254864269,0.311587260629241,
5.96932241712133));
#23976=CARTESIAN_POINT('Ctrl Pts',(-2.26686371206651,0.479750972411266,
6.17107030275971));
#23977=CARTESIAN_POINT('Ctrl Pts',(-2.25494487549033,0.530797361855725,
6.42870475627563));
#23978=CARTESIAN_POINT('Ctrl Pts',(-2.24302603891415,0.45226492573298,6.67933176541862));
#23979=CARTESIAN_POINT('Ctrl Pts',(-2.23110720233797,0.263325094846747,
6.86176802153349));
#23980=CARTESIAN_POINT('Ctrl Pts',(-2.2191883657618,0.0101020467317839,
6.93147693256131));
#23981=CARTESIAN_POINT('Ctrl Pts',(-2.20726952918561,-0.245587098572064,
6.87144120673232));
#23982=CARTESIAN_POINT('Ctrl Pts',(-2.19535069260943,-0.441323311848774,
6.69631656607358));
#23983=CARTESIAN_POINT('Ctrl Pts',(-2.18343185603326,-0.529323086465549,
6.44885519432254));
#23984=CARTESIAN_POINT('Ctrl Pts',(-2.17151301945708,-0.488104195118536,
6.18946640393034));
#23985=CARTESIAN_POINT('Ctrl Pts',(-2.1595941828809,-0.327728249264285,
5.98147509599461));
#23986=CARTESIAN_POINT('Ctrl Pts',(-2.14767534630472,-0.0873481558956701,
5.87565064933844));
#23987=CARTESIAN_POINT('Ctrl Pts',(-2.13575650972854,0.174357740366956,
5.89783918404992));
#23988=CARTESIAN_POINT('Ctrl Pts',(-2.12383767315236,0.393492635182685,
6.04259742479108));
#23989=CARTESIAN_POINT('Ctrl Pts',(-2.11191883657618,0.516574211951732,
6.27464227796523));
#23990=CARTESIAN_POINT('Ctrl Pts',(-2.10397294552539,0.514520161323001,
6.44967571052055));
#23991=CARTESIAN_POINT('Ctrl Pts',(-2.1,0.492610334572592,6.53165511107541));
#23992=CARTESIAN_POINT('Ctrl Pts',(-2.1,0.492610334572592,6.53165511107541));
#23993=CARTESIAN_POINT('Ctrl Pts',(-2.1,0.49635409029725,6.51110955003273));
#23994=CARTESIAN_POINT('Ctrl Pts',(-2.1,0.498800810154946,6.4903688790591));
#23995=CARTESIAN_POINT('Ctrl Pts',(-2.1,0.499959864786037,6.46955396620066));
#23996=CARTESIAN_POINT('Ctrl Pts',(-2.1,0.500651891757826,6.45712618175713));
#23997=CARTESIAN_POINT('Ctrl Pts',(-2.1,0.500884496511186,6.4446719156573));
#23998=CARTESIAN_POINT('Ctrl Pts',(-2.1,0.500656300483376,6.43221745273261));
#23999=CARTESIAN_POINT('Ctrl Pts',(-2.1,0.50051140625946,6.42430942840331));
#24000=CARTESIAN_POINT('Ctrl Pts',(-2.1,0.500180531457043,6.41639915136081));
#24001=CARTESIAN_POINT('Ctrl Pts',(-2.1,0.499663295188048,6.40850057461429));
#24002=CARTESIAN_POINT('Ctrl Pts',(-2.1,0.498282684765909,6.38741764205526));
#24003=CARTESIAN_POINT('Ctrl Pts',(-2.1,0.495579671230594,6.36646338372735));
#24004=CARTESIAN_POINT('Ctrl Pts',(-2.1,0.491553183641479,6.34576661740274));
#24005=CARTESIAN_POINT('Ctrl Pts',(-2.1,0.489189370076283,6.33361625162834));
#24006=CARTESIAN_POINT('Ctrl Pts',(-2.1,0.486369014762183,6.32155472699449));
#24007=CARTESIAN_POINT('Ctrl Pts',(-2.1,0.483088515935984,6.30960963623735));
#24008=CARTESIAN_POINT('Ctrl Pts',(-2.1,0.481387749157045,6.30341673247256));
#24009=CARTESIAN_POINT('Ctrl Pts',(-2.1,0.479562349371169,6.29725234131795));
#24010=CARTESIAN_POINT('Ctrl Pts',(-2.1,0.477614701955683,6.29113018362027));
#24011=CARTESIAN_POINT('Ctrl Pts',(-2.1,0.47691994455268,6.28894631073394));
#24012=CARTESIAN_POINT('Ctrl Pts',(-2.1,0.476209763711948,6.28676817605457));
#24013=CARTESIAN_POINT('Ctrl Pts',(-2.1,0.475484170198335,6.28459593876059));
#24014=CARTESIAN_POINT('Ctrl Pts',(-2.1,0.467396057947338,6.26038224508792));
#24015=CARTESIAN_POINT('Ctrl Pts',(-2.1,0.457396800695749,6.23689933548638));
#24016=CARTESIAN_POINT('Ctrl Pts',(-2.1,0.445625784567883,6.21434556134776));
#24017=CARTESIAN_POINT('Ctrl Pts',(-2.1,0.433955482728322,6.19198476012551));
#24018=CARTESIAN_POINT('Ctrl Pts',(-2.1,0.420542677238036,6.17053620507075));
#24019=CARTESIAN_POINT('Ctrl Pts',(-2.1,0.405485055004202,6.15022640072986));
#24020=CARTESIAN_POINT('Ctrl Pts',(-2.1,0.401547018955012,6.14491475587622));
#24021=CARTESIAN_POINT('Ctrl Pts',(-2.1,0.397496316871279,6.13968122438761));
#24022=CARTESIAN_POINT('Ctrl Pts',(-2.1,0.393334380355557,6.13453037462292));
#24023=CARTESIAN_POINT('Ctrl Pts',(-2.1,0.390073732726515,6.1304949680257));
#24024=CARTESIAN_POINT('Ctrl Pts',(-2.1,0.386745496616124,6.12651133724348));
#24025=CARTESIAN_POINT('Ctrl Pts',(-2.1,0.383357029508834,6.12258887921439));
#24026=CARTESIAN_POINT('Ctrl Pts',(-2.1,0.371904123413349,6.109331101568));
#24027=CARTESIAN_POINT('Ctrl Pts',(-2.1,0.35974458511925,6.09674730862358));
#24028=CARTESIAN_POINT('Ctrl Pts',(-2.1,0.346917810301558,6.08490712758635));
#24029=CARTESIAN_POINT('Ctrl Pts',(-2.1,0.328748103732818,6.06813497572237));
#24030=CARTESIAN_POINT('Ctrl Pts',(-2.1,0.309239814555027,6.0528527033034));
#24031=CARTESIAN_POINT('Ctrl Pts',(-2.1,0.288595198791424,6.03919240881688));
#24032=CARTESIAN_POINT('Ctrl Pts',(-2.1,0.278215530931981,6.03232430716481));
#24033=CARTESIAN_POINT('Ctrl Pts',(-2.1,0.26754829677856,6.02586696377693));
#24034=CARTESIAN_POINT('Ctrl Pts',(-2.1,0.256618135875702,6.01984205852923));
#24035=CARTESIAN_POINT('Ctrl Pts',(-2.1,0.251611498381037,6.01708230807514));
#24036=CARTESIAN_POINT('Ctrl Pts',(-2.1,0.246550009240434,6.01441370455151));
#24037=CARTESIAN_POINT('Ctrl Pts',(-2.1,0.241448312426713,6.01184414666615));
#24038=CARTESIAN_POINT('Ctrl Pts',(-2.1,0.219923137629529,6.00100261988527));
#24039=CARTESIAN_POINT('Ctrl Pts',(-2.1,0.197628752691819,5.99188954333672));
#24040=CARTESIAN_POINT('Ctrl Pts',(-2.1,0.174757433630984,5.98462368929255));
#24041=CARTESIAN_POINT('Ctrl Pts',(-2.1,0.165576347867032,5.98170700447212));
#24042=CARTESIAN_POINT('Ctrl Pts',(-2.1,0.156302149790289,5.97908854410605));
#24043=CARTESIAN_POINT('Ctrl Pts',(-2.1,0.146946980180942,5.97677835925102));
#24044=CARTESIAN_POINT('Ctrl Pts',(-2.1,0.136233092918806,5.97413264985985));
#24045=CARTESIAN_POINT('Ctrl Pts',(-2.1,0.125412970644963,5.971891235028));
#24046=CARTESIAN_POINT('Ctrl Pts',(-2.1,0.11450999527259,5.97005741415271));
#24047=CARTESIAN_POINT('Ctrl Pts',(-2.1,0.107187489851071,5.96882580875667));
#24048=CARTESIAN_POINT('Ctrl Pts',(-2.1,0.0998276196797078,5.96777809712117));
#24049=CARTESIAN_POINT('Ctrl Pts',(-2.1,0.0924376450671474,5.96691584094867));
#24050=CARTESIAN_POINT('Ctrl Pts',(-2.1,0.0866290251654119,5.96623809594594));
#24051=CARTESIAN_POINT('Ctrl Pts',(-2.1,0.0808012215405976,5.96567507726491));
#24052=CARTESIAN_POINT('Ctrl Pts',(-2.1,0.0749735051801638,5.96522838192892));
#24053=CARTESIAN_POINT('Ctrl Pts',(-2.1,0.0505591545770249,5.96335701828132));
#24054=CARTESIAN_POINT('Ctrl Pts',(-2.1,0.0260794227869884,5.96351369057634));
#24055=CARTESIAN_POINT('Ctrl Pts',(-2.1,0.00179128476957419,5.96570484843602));
#24056=CARTESIAN_POINT('Ctrl Pts',(-2.1,-0.0210365858903797,5.96776426806632));
#24057=CARTESIAN_POINT('Ctrl Pts',(-2.1,-0.0436964113942735,5.97162157501662));
#24058=CARTESIAN_POINT('Ctrl Pts',(-2.1,-0.065956881641688,5.97732901798388));
#24059=CARTESIAN_POINT('Ctrl Pts',(-2.1,-0.0673808531784219,5.97769411522767));
#24060=CARTESIAN_POINT('Ctrl Pts',(-2.1,-0.0688031806876158,5.97806679811498));
#24061=CARTESIAN_POINT('Ctrl Pts',(-2.1,-0.0702237992588386,5.97844708639908));
#24062=CARTESIAN_POINT('Ctrl Pts',(-2.1,-0.0736400801676868,5.97936159760649));
#24063=CARTESIAN_POINT('Ctrl Pts',(-2.1,-0.0770464797446285,5.9803200895664));
#24064=CARTESIAN_POINT('Ctrl Pts',(-2.1,-0.0804421690761142,5.98132232055468));
#24065=CARTESIAN_POINT('Ctrl Pts',(-2.6,-0.322335278395778,6.67898325810255));
#24066=CARTESIAN_POINT('Ctrl Pts',(-2.6,-0.339120601259259,6.66300806279478));
#24067=CARTESIAN_POINT('Ctrl Pts',(-2.6,-0.354506984127668,6.64569922647684));
#24068=CARTESIAN_POINT('Ctrl Pts',(-2.6,-0.368421126683117,6.62729272970921));
#24069=CARTESIAN_POINT('Ctrl Pts',(-2.6,-0.38257126416386,6.60857404411556));
#24070=CARTESIAN_POINT('Ctrl Pts',(-2.6,-0.395199756274692,6.58871918836577));
#24071=CARTESIAN_POINT('Ctrl Pts',(-2.6,-0.406199318727697,6.56793181289168));
#24072=CARTESIAN_POINT('Ctrl Pts',(-2.6,-0.409616043928294,6.56147476062801));
#24073=CARTESIAN_POINT('Ctrl Pts',(-2.6,-0.412875324168305,6.55492747138162));
#24074=CARTESIAN_POINT('Ctrl Pts',(-2.6,-0.415973133660165,6.54829542707107));
#24075=CARTESIAN_POINT('Ctrl Pts',(-2.6,-0.418485108810516,6.54291758490618));
#24076=CARTESIAN_POINT('Ctrl Pts',(-2.6,-0.420891069789125,6.53748311927057));
#24077=CARTESIAN_POINT('Ctrl Pts',(-2.6,-0.423182724471203,6.53201048034897));
#24078=CARTESIAN_POINT('Ctrl Pts',(-2.6,-0.42826857782987,6.51986509070635));
#24079=CARTESIAN_POINT('Ctrl Pts',(-2.6,-0.432799982024353,6.50751484134792));
#24080=CARTESIAN_POINT('Ctrl Pts',(-2.6,-0.436762141475896,6.49499689828687));
#24081=CARTESIAN_POINT('Ctrl Pts',(-2.6,-0.444013330815057,6.47208768012373));
#24082=CARTESIAN_POINT('Ctrl Pts',(-2.6,-0.449360985234842,6.44861814961569));
#24083=CARTESIAN_POINT('Ctrl Pts',(-2.6,-0.452831510630463,6.42482689824574));
#24084=CARTESIAN_POINT('Ctrl Pts',(-2.6,-0.45503518273379,6.40972021814094));
#24085=CARTESIAN_POINT('Ctrl Pts',(-2.6,-0.456481100414613,6.39448317547527));
#24086=CARTESIAN_POINT('Ctrl Pts',(-2.6,-0.457165780866727,6.37917321940029));
#24087=CARTESIAN_POINT('Ctrl Pts',(-2.6,-0.457426442969031,6.37334462399588));
#24088=CARTESIAN_POINT('Ctrl Pts',(-2.6,-0.457576507352781,6.36750526353339));
#24089=CARTESIAN_POINT('Ctrl Pts',(-2.6,-0.457615909648183,6.36167325953747));
#24090=CARTESIAN_POINT('Ctrl Pts',(-2.6,-0.457783624314556,6.33684951273631));
#24091=CARTESIAN_POINT('Ctrl Pts',(-2.6,-0.455954126792007,6.3120946330561));
#24092=CARTESIAN_POINT('Ctrl Pts',(-2.6,-0.452154218947823,6.28765697027383));
#24093=CARTESIAN_POINT('Ctrl Pts',(-2.6,-0.45115674289519,6.28124208222728));
#24094=CARTESIAN_POINT('Ctrl Pts',(-2.6,-0.450023226879442,6.27484896612481));
#24095=CARTESIAN_POINT('Ctrl Pts',(-2.6,-0.448753579228988,6.26848198366457));
#24096=CARTESIAN_POINT('Ctrl Pts',(-2.6,-0.444848441945282,6.24889864447494));
#24097=CARTESIAN_POINT('Ctrl Pts',(-2.6,-0.43965712635916,6.22956230418047));
#24098=CARTESIAN_POINT('Ctrl Pts',(-2.6,-0.433239797159997,6.21057739588651));
#24099=CARTESIAN_POINT('Ctrl Pts',(-2.6,-0.431489703713964,6.20539995172748));
#24100=CARTESIAN_POINT('Ctrl Pts',(-2.6,-0.429647959283524,6.200247760375));
#24101=CARTESIAN_POINT('Ctrl Pts',(-2.6,-0.427716565518185,6.19512580861043));
#24102=CARTESIAN_POINT('Ctrl Pts',(-2.6,-0.418824441384019,6.17154437652905));
#24103=CARTESIAN_POINT('Ctrl Pts',(-2.6,-0.408091715271334,6.14874908227563));
#24104=CARTESIAN_POINT('Ctrl Pts',(-2.6,-0.395672419048227,6.12693682894624));
#24105=CARTESIAN_POINT('Ctrl Pts',(-2.6,-0.383092367331082,6.10484223759245));
#24106=CARTESIAN_POINT('Ctrl Pts',(-2.6,-0.368781416403301,6.08375495651898));
#24107=CARTESIAN_POINT('Ctrl Pts',(-2.6,-0.352848584276632,6.06389024080292));
#24108=CARTESIAN_POINT('Ctrl Pts',(-2.6,-0.350477674538742,6.06093424104361));
#24109=CARTESIAN_POINT('Ctrl Pts',(-2.6,-0.348070766049518,6.05800535381594));
#24110=CARTESIAN_POINT('Ctrl Pts',(-2.6,-0.345628131270321,6.05510433731261));
#24111=CARTESIAN_POINT('Ctrl Pts',(-2.6,-0.341175445450433,6.04981606615654));
#24112=CARTESIAN_POINT('Ctrl Pts',(-2.6,-0.336604054215743,6.04462039757467));
#24113=CARTESIAN_POINT('Ctrl Pts',(-2.6,-0.331917615661801,6.03951989728949));
#24114=CARTESIAN_POINT('Ctrl Pts',(-2.6,-0.327197865992937,6.03438314274658));
#24115=CARTESIAN_POINT('Ctrl Pts',(-2.6,-0.322366287452079,6.02934835553984));
#24116=CARTESIAN_POINT('Ctrl Pts',(-2.6,-0.317432494385971,6.02442266645077));
#24117=CARTESIAN_POINT('Ctrl Pts',(-2.6,-0.305161639297739,6.01217196679398));
#24118=CARTESIAN_POINT('Ctrl Pts',(-2.6,-0.292249931632248,6.00058562939064));
#24119=CARTESIAN_POINT('Ctrl Pts',(-2.6,-0.278765100808516,5.98969663827542));
#24120=CARTESIAN_POINT('Ctrl Pts',(-2.6,-0.268765025516792,5.98162158472625));
#24121=CARTESIAN_POINT('Ctrl Pts',(-2.6,-0.258449546075054,5.97393011620472));
#24122=CARTESIAN_POINT('Ctrl Pts',(-2.6,-0.247843342520938,5.96663792616377));
#24123=CARTESIAN_POINT('Ctrl Pts',(-2.6,-0.241099106168833,5.96200099336216));
#24124=CARTESIAN_POINT('Ctrl Pts',(-2.6,-0.234236247932732,5.9575251822992));
#24125=CARTESIAN_POINT('Ctrl Pts',(-2.6,-0.227275760973999,5.95322352477529));
#24126=CARTESIAN_POINT('Ctrl Pts',(-2.6,-0.204751973270828,5.93930357615464));
#24127=CARTESIAN_POINT('Ctrl Pts',(-2.6,-0.181175137781382,5.92718033261133));
#24128=CARTESIAN_POINT('Ctrl Pts',(-2.6,-0.156760783265524,5.91698457674055));
#24129=CARTESIAN_POINT('Ctrl Pts',(-2.6,-0.152585729857118,5.91524101947092));
#24130=CARTESIAN_POINT('Ctrl Pts',(-2.6,-0.148386104006604,5.91355392287942));
#24131=CARTESIAN_POINT('Ctrl Pts',(-2.6,-0.144162892324896,5.91192406382743));
#24132=CARTESIAN_POINT('Ctrl Pts',(-2.6,-0.140229927621667,5.91040621944599));
#24133=CARTESIAN_POINT('Ctrl Pts',(-2.6,-0.136276507298105,5.90893801577657));
#24134=CARTESIAN_POINT('Ctrl Pts',(-2.6,-0.132303594671778,5.90751949357016));
#24135=CARTESIAN_POINT('Ctrl Pts',(-2.3579681670589,0.426284649716722,6.39998978457651));
#24136=CARTESIAN_POINT('Ctrl Pts',(-2.35918653419807,0.426303967962151,
6.37823165906101));
#24137=CARTESIAN_POINT('Ctrl Pts',(-2.36040490133724,0.424667502862756,
6.35647641245579));
#24138=CARTESIAN_POINT('Ctrl Pts',(-2.36162326847641,0.421350422927922,
6.33498050516036));
#24139=CARTESIAN_POINT('Ctrl Pts',(-2.3655962140018,0.41053383286997,6.26488499293085));
#24140=CARTESIAN_POINT('Ctrl Pts',(-2.3695691595272,0.381846728178515,6.19754711846157));
#24141=CARTESIAN_POINT('Ctrl Pts',(-2.37354210505259,0.338790672280628,
6.14118617891461));
#24142=CARTESIAN_POINT('Ctrl Pts',(-2.37751505057798,0.295734616382741,
6.08482523936765));
#24143=CARTESIAN_POINT('Ctrl Pts',(-2.38148799610338,0.238309609278423,
6.03944123474302));
#24144=CARTESIAN_POINT('Ctrl Pts',(-2.38546094162877,0.173524978230831,
6.01057376109627));
#24145=CARTESIAN_POINT('Ctrl Pts',(-2.38943388715416,0.10874034718324,5.98170628744951));
#24146=CARTESIAN_POINT('Ctrl Pts',(-2.39340683267956,0.036596092192376,
5.96935534478063));
#24147=CARTESIAN_POINT('Ctrl Pts',(-2.39737977820495,-0.0341018201830637,
5.97502849571334));
#24148=CARTESIAN_POINT('Ctrl Pts',(-2.40135272373034,-0.104799732558504,
5.98070164664604));
#24149=CARTESIAN_POINT('Ctrl Pts',(-2.40532566925574,-0.174051302318518,
6.00439889118032));
#24150=CARTESIAN_POINT('Ctrl Pts',(-2.40929861478113,-0.233403645578344,
6.0432277310782));
#24151=CARTESIAN_POINT('Ctrl Pts',(-2.41327156030652,-0.29275598883817,
6.08205657097609));
#24152=CARTESIAN_POINT('Ctrl Pts',(-2.41724450583192,-0.342209105597808,
6.13601700623758));
#24153=CARTESIAN_POINT('Ctrl Pts',(-2.42121745135731,-0.375726721884694,
6.19852259672729));
#24154=CARTESIAN_POINT('Ctrl Pts',(-2.4251903968827,-0.40924433817158,6.261028187217));
#24155=CARTESIAN_POINT('Ctrl Pts',(-2.4291633424081,-0.426826453985716,
6.33207893293493));
#24156=CARTESIAN_POINT('Ctrl Pts',(-2.43313628793349,-0.426326986682199,
6.40300234245982));
#24157=CARTESIAN_POINT('Ctrl Pts',(-2.43710923345888,-0.425827519378683,
6.4739257519847));
#24158=CARTESIAN_POINT('Ctrl Pts',(-2.44108217898427,-0.407246468957515,
6.54472182531654));
#24159=CARTESIAN_POINT('Ctrl Pts',(-2.44505512450967,-0.372851848709961,
6.60674915389561));
#24160=CARTESIAN_POINT('Ctrl Pts',(-2.44902807003506,-0.338457228462407,
6.66877648247468));
#24161=CARTESIAN_POINT('Ctrl Pts',(-2.45300101556045,-0.288249038388467,
6.72203506630097));
#24162=CARTESIAN_POINT('Ctrl Pts',(-2.45697396108585,-0.228355716569631,
6.76002413778667));
#24163=CARTESIAN_POINT('Ctrl Pts',(-2.46094690661124,-0.168462394750795,
6.79801320927237));
#24164=CARTESIAN_POINT('Ctrl Pts',(-2.46491985213663,-0.0988839411870617,
6.82073276841748));
#24165=CARTESIAN_POINT('Ctrl Pts',(-2.46889279766203,-0.0281131406535831,
6.82540964542417));
#24166=CARTESIAN_POINT('Ctrl Pts',(-2.47286574318742,0.0426576598798955,
6.83008652243086));
#24167=CARTESIAN_POINT('Ctrl Pts',(-2.47683868871281,0.11462080738312,6.81672071729912));
#24168=CARTESIAN_POINT('Ctrl Pts',(-2.48081163423821,0.178992444175497,
6.78694368501647));
#24169=CARTESIAN_POINT('Ctrl Pts',(-2.4847845797636,0.243364080967874,6.75716665273382));
#24170=CARTESIAN_POINT('Ctrl Pts',(-2.48875752528899,0.300144207049405,
6.71097839330025));
#24171=CARTESIAN_POINT('Ctrl Pts',(-2.49273047081439,0.342402203643058,
6.65401663255403));
#24172=CARTESIAN_POINT('Ctrl Pts',(-2.49670341633978,0.384660200236712,
6.59705487180782));
#24173=CARTESIAN_POINT('Ctrl Pts',(-2.50067636186517,0.41239606734249,6.52931960974896));
#24174=CARTESIAN_POINT('Ctrl Pts',(-2.50464930739057,0.422224363177276,
6.45907873054876));
#24175=CARTESIAN_POINT('Ctrl Pts',(-2.50575559394668,0.424961101318294,
6.4395198063571));
#24176=CARTESIAN_POINT('Ctrl Pts',(-2.50686188050279,0.426309336731809,
6.41976660365709));
#24177=CARTESIAN_POINT('Ctrl Pts',(-2.50796816705891,0.426290360635438,
6.40001083203199));
#24178=CARTESIAN_POINT('Ctrl Pts',(-2.6,0.132288496556895,5.90755938055567));
#24179=CARTESIAN_POINT('Ctrl Pts',(-2.59602705447461,0.214239653399634,
5.92957461427473));
#24180=CARTESIAN_POINT('Ctrl Pts',(-2.58808116342382,0.366850103542102,
6.0153123398751));
#24181=CARTESIAN_POINT('Ctrl Pts',(-2.57616232684764,0.506266020658281,
6.23792666630748));
#24182=CARTESIAN_POINT('Ctrl Pts',(-2.56424349027146,0.522062886964902,
6.50008215105946));
#24183=CARTESIAN_POINT('Ctrl Pts',(-2.55232465369528,0.410425773087965,
6.73782039475945));
#24184=CARTESIAN_POINT('Ctrl Pts',(-2.54040581711911,0.19858907062663,6.89308342832313));
#24185=CARTESIAN_POINT('Ctrl Pts',(-2.52848698054292,-0.0617246536500735,
6.92797742227401));
#24186=CARTESIAN_POINT('Ctrl Pts',(-2.51656814396674,-0.306971377021502,
6.8339796336226));
#24187=CARTESIAN_POINT('Ctrl Pts',(-2.50464930739056,-0.477279320739804,
6.63403891232169));
#24188=CARTESIAN_POINT('Ctrl Pts',(-2.49273047081439,-0.531073600862929,
6.3769640630774));
#24189=CARTESIAN_POINT('Ctrl Pts',(-2.48081163423821,-0.455221493256117,
6.12551290982166));
#24190=CARTESIAN_POINT('Ctrl Pts',(-2.46889279766203,-0.268240284898955,
5.94106977614238));
#24191=CARTESIAN_POINT('Ctrl Pts',(-2.45697396108585,-0.0157759417689948,
5.86866121228054));
#24192=CARTESIAN_POINT('Ctrl Pts',(-2.44505512450967,0.240539628301038,
5.92596363104932));
#24193=CARTESIAN_POINT('Ctrl Pts',(-2.43313628793349,0.438134411540293,
6.09898832463164));
#24194=CARTESIAN_POINT('Ctrl Pts',(-2.42121745135731,0.528771348081292,
6.34549630925116));
#24195=CARTESIAN_POINT('Ctrl Pts',(-2.40929861478113,0.490324055555984,
6.60530979488368));
#24196=CARTESIAN_POINT('Ctrl Pts',(-2.39737977820495,0.332178326477852,
6.81500283186379));
#24197=CARTESIAN_POINT('Ctrl Pts',(-2.38546094162877,0.092940867251264,
6.92338493135519));
#24198=CARTESIAN_POINT('Ctrl Pts',(-2.37354210505259,-0.168985416607936,
6.90399773818908));
#24199=CARTESIAN_POINT('Ctrl Pts',(-2.36162326847641,-0.38965879870384,
6.76157407502307));
#24200=CARTESIAN_POINT('Ctrl Pts',(-2.34970443190023,-0.515208255680234,
6.5308825596382));
#24201=CARTESIAN_POINT('Ctrl Pts',(-2.33778559532405,-0.514984518987432,
6.26823985300105));
#24202=CARTESIAN_POINT('Ctrl Pts',(-2.32586675874787,-0.389042207488899,
6.03776257519368));
#24203=CARTESIAN_POINT('Ctrl Pts',(-2.31394792217169,-0.168126493747137,
5.89571508724314));
#24204=CARTESIAN_POINT('Ctrl Pts',(-2.30202908559551,0.0938324405162212,
5.87677417471489));
#24205=CARTESIAN_POINT('Ctrl Pts',(-2.29011024901934,0.332884898468083,
5.98556371357228));
#24206=CARTESIAN_POINT('Ctrl Pts',(-2.27819141244316,0.490673136844557,
6.19552588451105));
#24207=CARTESIAN_POINT('Ctrl Pts',(-2.26627257586698,0.528677721240565,
6.45540449655913));
#24208=CARTESIAN_POINT('Ctrl Pts',(-2.2543537392908,0.437620931409163,6.70175770318116));
#24209=CARTESIAN_POINT('Ctrl Pts',(-2.24243490271462,0.239731649313908,
6.87444549491937));
#24210=CARTESIAN_POINT('Ctrl Pts',(-2.23051606613844,-0.0166811816108265,
6.93131114145764));
#24211=CARTESIAN_POINT('Ctrl Pts',(-2.21859722956226,-0.269021783055123,
6.85847254173578));
#24212=CARTESIAN_POINT('Ctrl Pts',(-2.20667839298608,-0.455688500581004,
6.67371112931225));
#24213=CARTESIAN_POINT('Ctrl Pts',(-2.1947595564099,-0.53111204424701,6.42213106706975));
#24214=CARTESIAN_POINT('Ctrl Pts',(-2.18284071983372,-0.476879959029563,
6.1651483330086));
#24215=CARTESIAN_POINT('Ctrl Pts',(-2.17092188325754,-0.306231393425269,
5.96549786619889));
#24216=CARTESIAN_POINT('Ctrl Pts',(-2.15900304668136,-0.0608253588918372,
5.8719184725451));
#24217=CARTESIAN_POINT('Ctrl Pts',(-2.14708421010518,0.199429574813985,
5.90725502825896));
#24218=CARTESIAN_POINT('Ctrl Pts',(-2.135165373529,0.410999230249818,6.06288076079265));
#24219=CARTESIAN_POINT('Ctrl Pts',(-2.12324653695282,0.522235994732442,
6.30080495423084));
#24220=CARTESIAN_POINT('Ctrl Pts',(-2.11132770037665,0.505982491766854,
6.56294356165447));
#24221=CARTESIAN_POINT('Ctrl Pts',(-2.09940886380046,0.366211204665212,
6.78530674521469));
#24222=CARTESIAN_POINT('Ctrl Pts',(-2.08749002722428,0.137033499838515,
6.91360287657764));
#24223=CARTESIAN_POINT('Ctrl Pts',(-2.07557119064811,-0.125581190928044,
6.91652919922544));
#24224=CARTESIAN_POINT('Ctrl Pts',(-2.06365235407193,-0.357565218298462,
6.79333282215497));
#24225=CARTESIAN_POINT('Ctrl Pts',(-2.05570646302114,-0.453961018087142,
6.64722068416873));
#24226=CARTESIAN_POINT('Ctrl Pts',(-2.05173351749575,-0.481760682217403,
6.56704686488953));
#24227=CARTESIAN_POINT('Ctrl Pts',(-2.61608882750142,0.12505876634041,5.9344718704462));
#24228=CARTESIAN_POINT('Ctrl Pts',(-2.61211588197602,0.202531190940192,
5.95528394436993));
#24229=CARTESIAN_POINT('Ctrl Pts',(-2.60416999092524,0.346801290927786,
6.03633599705392));
#24230=CARTESIAN_POINT('Ctrl Pts',(-2.59225115434906,0.478597955464431,
6.24678417477103));
#24231=CARTESIAN_POINT('Ctrl Pts',(-2.58033231777288,0.493531503458158,
6.49461253752179));
#24232=CARTESIAN_POINT('Ctrl Pts',(-2.5684134811967,0.387995496151209,6.71935809169225));
#24233=CARTESIAN_POINT('Ctrl Pts',(-2.55649464462052,0.187735931903752,
6.86613580813106));
#24234=CARTESIAN_POINT('Ctrl Pts',(-2.54457580804434,-0.0583513248632879,
6.89912280208567));
#24235=CARTESIAN_POINT('Ctrl Pts',(-2.53265697146816,-0.290195010989602,
6.81026210902899));
#24236=CARTESIAN_POINT('Ctrl Pts',(-2.52073813489198,-0.451195414605367,
6.62124839583474));
#24237=CARTESIAN_POINT('Ctrl Pts',(-2.5088192983158,-0.50204977067914,6.37822300556726));
#24238=CARTESIAN_POINT('Ctrl Pts',(-2.49690046173962,-0.430343074719011,
6.14051396933589));
#24239=CARTESIAN_POINT('Ctrl Pts',(-2.48498162516344,-0.253580621031822,
5.96615088140125));
#24240=CARTESIAN_POINT('Ctrl Pts',(-2.47306278858726,-0.0149137670080035,
5.89769953525455));
#24241=CARTESIAN_POINT('Ctrl Pts',(-2.46114395201109,0.227393839632693,
5.95187030585109));
#24242=CARTESIAN_POINT('Ctrl Pts',(-2.44922511543491,0.414189823186519,
6.11543898558529));
#24243=CARTESIAN_POINT('Ctrl Pts',(-2.43730627885873,0.499873338864062,
6.34847500347002));
#24244=CARTESIAN_POINT('Ctrl Pts',(-2.42538744228255,0.463527238503961,
6.59408936025449));
#24245=CARTESIAN_POINT('Ctrl Pts',(-2.41346860570637,0.314024369431667,
6.79232241299485));
#24246=CARTESIAN_POINT('Ctrl Pts',(-2.40154976913019,0.0878615337203718,
6.89478129648476));
#24247=CARTESIAN_POINT('Ctrl Pts',(-2.38963093255401,-0.159750154250334,
6.87645363744213));
#24248=CARTESIAN_POINT('Ctrl Pts',(-2.37771209597783,-0.368363462643409,
6.74181360390328));
#24249=CARTESIAN_POINT('Ctrl Pts',(-2.36579325940165,-0.487051486264749,
6.52372966561601));
#24250=CARTESIAN_POINT('Ctrl Pts',(-2.35387442282547,-0.486839977059375,
6.27544070825967));
#24251=CARTESIAN_POINT('Ctrl Pts',(-2.34195558624929,-0.367780568902201,
6.05755929920087));
#24252=CARTESIAN_POINT('Ctrl Pts',(-2.33003674967311,-0.158938172587915,
5.92327488243597));
#24253=CARTESIAN_POINT('Ctrl Pts',(-2.31811791309693,0.0887043814019138,
5.90536911424148));
#24254=CARTESIAN_POINT('Ctrl Pts',(-2.30619907652075,0.314692326387328,
6.0082131700313));
#24255=CARTESIAN_POINT('Ctrl Pts',(-2.29428023994457,0.463857242067669,
6.20670064822607));
#24256=CARTESIAN_POINT('Ctrl Pts',(-2.28236140336839,0.499784828846167,
6.45237657218681));
#24257=CARTESIAN_POINT('Ctrl Pts',(-2.27044256679221,0.413704405380657,
6.68526627088336));
#24258=CARTESIAN_POINT('Ctrl Pts',(-2.25852373021604,0.226630017698138,
6.84851646087657));
#24259=CARTESIAN_POINT('Ctrl Pts',(-2.24660489363986,-0.0157695343710637,
6.90227432938608));
#24260=CARTESIAN_POINT('Ctrl Pts',(-2.23468605706368,-0.254319409345632,
6.83341644937185));
#24261=CARTESIAN_POINT('Ctrl Pts',(-2.2227672204875,-0.430784559515061,
6.65875247702062));
#24262=CARTESIAN_POINT('Ctrl Pts',(-2.21084838391132,-0.502086113084658,
6.42092157683831));
#24263=CARTESIAN_POINT('Ctrl Pts',(-2.19892954733514,-0.450817878507322,
6.1779832675451));
#24264=CARTESIAN_POINT('Ctrl Pts',(-2.18701071075896,-0.289495468413598,
5.98924394607454));
#24265=CARTESIAN_POINT('Ctrl Pts',(-2.17509187418278,-0.05750117767764,
5.90077878221055));
#24266=CARTESIAN_POINT('Ctrl Pts',(-2.1631730376066,0.188530501496047,5.93418415137954));
#24267=CARTESIAN_POINT('Ctrl Pts',(-2.15125420103042,0.388537613168766,
6.08130474484033));
#24268=CARTESIAN_POINT('Ctrl Pts',(-2.13933536445424,0.493695150671756,
6.30622608636544));
#24269=CARTESIAN_POINT('Ctrl Pts',(-2.12741652787806,0.478329921778157,
6.55403849415475));
#24270=CARTESIAN_POINT('Ctrl Pts',(-2.11549769130188,0.346197308665989,
6.76424925426879));
#24271=CARTESIAN_POINT('Ctrl Pts',(-2.1035788547257,0.129544449314556,6.88553384311886));
#24272=CARTESIAN_POINT('Ctrl Pts',(-2.09166001814953,-0.11871802327322,
6.88830023860881));
#24273=CARTESIAN_POINT('Ctrl Pts',(-2.07974118157334,-0.338023836164873,
6.77183669616154));
#24274=CARTESIAN_POINT('Ctrl Pts',(-2.07179529052256,-0.429151486079503,
6.63370976752069));
#24275=CARTESIAN_POINT('Ctrl Pts',(-2.06782234499716,-0.455431864126683,
6.55791754678483));
#24276=CARTESIAN_POINT('Ctrl Pts',(-2.63217765500284,0.117829036123926,
5.96138436033673));
#24277=CARTESIAN_POINT('Ctrl Pts',(-2.62820470947744,0.190822728480749,
5.98099327446513));
#24278=CARTESIAN_POINT('Ctrl Pts',(-2.62025881842666,0.326752478313469,
6.05735965423274));
#24279=CARTESIAN_POINT('Ctrl Pts',(-2.60833998185048,0.450929890270581,
6.25564168323458));
#24280=CARTESIAN_POINT('Ctrl Pts',(-2.5964211452743,0.465000119951414,6.48914292398412));
#24281=CARTESIAN_POINT('Ctrl Pts',(-2.58450230869812,0.365565219214455,
6.70089578862506));
#24282=CARTESIAN_POINT('Ctrl Pts',(-2.57258347212194,0.176882793180874,
6.83918818793898));
#24283=CARTESIAN_POINT('Ctrl Pts',(-2.56066463554576,-0.0549779960765018,
6.87026818189733));
#24284=CARTESIAN_POINT('Ctrl Pts',(-2.54874579896958,-0.273418644957702,
6.78654458443538));
#24285=CARTESIAN_POINT('Ctrl Pts',(-2.5368269623934,-0.42511150847093,6.60845787934779));
#24286=CARTESIAN_POINT('Ctrl Pts',(-2.52490812581722,-0.473025940495352,
6.37948194805711));
#24287=CARTESIAN_POINT('Ctrl Pts',(-2.51298928924104,-0.405464656181905,
6.15551502885011));
#24288=CARTESIAN_POINT('Ctrl Pts',(-2.50107045266486,-0.23892095716469,
5.99123198666013));
#24289=CARTESIAN_POINT('Ctrl Pts',(-2.48915161608868,-0.014051592247013,
5.92673785822857));
#24290=CARTESIAN_POINT('Ctrl Pts',(-2.4772327795125,0.214248050964349,5.97777698065287));
#24291=CARTESIAN_POINT('Ctrl Pts',(-2.46531394293632,0.390245234832745,
6.13188964653893));
#24292=CARTESIAN_POINT('Ctrl Pts',(-2.45339510636014,0.470975329646833,
6.35145369768889));
#24293=CARTESIAN_POINT('Ctrl Pts',(-2.44147626978396,0.436730421451937,
6.5828689256253));
#24294=CARTESIAN_POINT('Ctrl Pts',(-2.42955743320779,0.295870412385483,
6.76964199412591));
#24295=CARTESIAN_POINT('Ctrl Pts',(-2.41763859663161,0.0827822001894799,
6.86617766161433));
#24296=CARTESIAN_POINT('Ctrl Pts',(-2.40571976005543,-0.150514891892733,
6.84890953669518));
#24297=CARTESIAN_POINT('Ctrl Pts',(-2.39380092347925,-0.347068126582978,
6.7220531327835));
#24298=CARTESIAN_POINT('Ctrl Pts',(-2.38188208690307,-0.458894716849264,
6.51657677159381));
#24299=CARTESIAN_POINT('Ctrl Pts',(-2.36996325032689,-0.458695435131318,
6.28264156351829));
#24300=CARTESIAN_POINT('Ctrl Pts',(-2.35804441375071,-0.346518930315503,
6.07735602320807));
#24301=CARTESIAN_POINT('Ctrl Pts',(-2.34612557717453,-0.149749851428694,
5.9508346776288));
#24302=CARTESIAN_POINT('Ctrl Pts',(-2.33420674059835,0.0835763222876063,
5.93396405376808));
#24303=CARTESIAN_POINT('Ctrl Pts',(-2.32228790402217,0.296499754306572,
6.03086262649031));
#24304=CARTESIAN_POINT('Ctrl Pts',(-2.31036906744599,0.437041347290782,
6.2178754119411));
#24305=CARTESIAN_POINT('Ctrl Pts',(-2.29845023086981,0.470891936451769,
6.44934864781448));
#24306=CARTESIAN_POINT('Ctrl Pts',(-2.28653139429363,0.389787879352151,
6.66877483858555));
#24307=CARTESIAN_POINT('Ctrl Pts',(-2.27461255771745,0.213528386082369,
6.82258742683378));
#24308=CARTESIAN_POINT('Ctrl Pts',(-2.26269372114127,-0.0148578871313011,
6.87323751731453));
#24309=CARTESIAN_POINT('Ctrl Pts',(-2.2507748845651,-0.239617035636141,
6.80836035700791));
#24310=CARTESIAN_POINT('Ctrl Pts',(-2.23885604798891,-0.405880618449119,
6.64379382472899));
#24311=CARTESIAN_POINT('Ctrl Pts',(-2.22693721141274,-0.473060181922306,
6.41971208660688));
#24312=CARTESIAN_POINT('Ctrl Pts',(-2.21501837483656,-0.424755797985082,
6.1908182020816));
#24313=CARTESIAN_POINT('Ctrl Pts',(-2.20309953826038,-0.272759543401928,
6.01299002595018));
#24314=CARTESIAN_POINT('Ctrl Pts',(-2.1911807016842,-0.0541769964634428,
5.92963909187599));
#24315=CARTESIAN_POINT('Ctrl Pts',(-2.17926186510802,0.17763142817811,5.96111327450012));
#24316=CARTESIAN_POINT('Ctrl Pts',(-2.16734302853184,0.366075996087714,
6.099728728888));
#24317=CARTESIAN_POINT('Ctrl Pts',(-2.15542419195566,0.465154306611069,
6.31164721850004));
#24318=CARTESIAN_POINT('Ctrl Pts',(-2.14350535537948,0.450677351789461,
6.54513342665504));
#24319=CARTESIAN_POINT('Ctrl Pts',(-2.1315865188033,0.326183412666766,6.74319176332289));
#24320=CARTESIAN_POINT('Ctrl Pts',(-2.11966768222712,0.122055398790597,
6.85746480966008));
#24321=CARTESIAN_POINT('Ctrl Pts',(-2.10774884565094,-0.111854855618396,
6.8600712779922));
#24322=CARTESIAN_POINT('Ctrl Pts',(-2.09583000907476,-0.318482454031284,
6.7503405701681));
#24323=CARTESIAN_POINT('Ctrl Pts',(-2.08788411802398,-0.404341954071864,
6.62019885087265));
#24324=CARTESIAN_POINT('Ctrl Pts',(-2.08391117249858,-0.429103046035963,
6.54878822868013));
#24325=CARTESIAN_POINT('Ctrl Pts',(-2.64826648250425,0.110599305907441,
5.98829685022726));
#24326=CARTESIAN_POINT('Ctrl Pts',(-2.64429353697886,0.179114266021306,
6.00670260456034));
#24327=CARTESIAN_POINT('Ctrl Pts',(-2.63634764592807,0.306703665699153,
6.07838331141156));
#24328=CARTESIAN_POINT('Ctrl Pts',(-2.6244288093519,0.423261825076731,6.26449919169813));
#24329=CARTESIAN_POINT('Ctrl Pts',(-2.61250997277572,0.436468736444671,
6.48367331044645));
#24330=CARTESIAN_POINT('Ctrl Pts',(-2.60059113619953,0.3431349422777,6.68243348555786));
#24331=CARTESIAN_POINT('Ctrl Pts',(-2.58867229962336,0.166029654457996,
6.81224056774691));
#24332=CARTESIAN_POINT('Ctrl Pts',(-2.57675346304718,-0.0516046672897163,
6.84141356170898));
#24333=CARTESIAN_POINT('Ctrl Pts',(-2.564834626471,-0.256642278925802,6.76282705984177));
#24334=CARTESIAN_POINT('Ctrl Pts',(-2.55291578989482,-0.399027602336494,
6.59566736286083));
#24335=CARTESIAN_POINT('Ctrl Pts',(-2.54099695331864,-0.444002110311564,
6.38074089054697));
#24336=CARTESIAN_POINT('Ctrl Pts',(-2.52907811674246,-0.380586237644799,
6.17051608836433));
#24337=CARTESIAN_POINT('Ctrl Pts',(-2.51715928016628,-0.224261293297557,
6.016313091919));
#24338=CARTESIAN_POINT('Ctrl Pts',(-2.5052404435901,-0.0131894174860218,
5.95577618120258));
#24339=CARTESIAN_POINT('Ctrl Pts',(-2.49332160701392,0.201102262296004,
6.00368365545465));
#24340=CARTESIAN_POINT('Ctrl Pts',(-2.48140277043774,0.366300646478971,
6.14834030749258));
#24341=CARTESIAN_POINT('Ctrl Pts',(-2.46948393386156,0.442077320429603,
6.35443239190776));
#24342=CARTESIAN_POINT('Ctrl Pts',(-2.45756509728538,0.409933604399914,
6.57164849099611));
#24343=CARTESIAN_POINT('Ctrl Pts',(-2.4456462607092,0.277716455339298,6.74696157525698));
#24344=CARTESIAN_POINT('Ctrl Pts',(-2.43372742413302,0.0777028666585877,
6.8375740267439));
#24345=CARTESIAN_POINT('Ctrl Pts',(-2.42180858755684,-0.141279629535131,
6.82136543594824));
#24346=CARTESIAN_POINT('Ctrl Pts',(-2.40988975098066,-0.325772790522547,
6.70229266166372));
#24347=CARTESIAN_POINT('Ctrl Pts',(-2.39797091440449,-0.430737947433779,
6.50942387757162));
#24348=CARTESIAN_POINT('Ctrl Pts',(-2.38605207782831,-0.43055089320326,
6.28984241877691));
#24349=CARTESIAN_POINT('Ctrl Pts',(-2.37413324125213,-0.325257291728805,
6.09715274721527));
#24350=CARTESIAN_POINT('Ctrl Pts',(-2.36221440467595,-0.140561530269473,
5.97839447282163));
#24351=CARTESIAN_POINT('Ctrl Pts',(-2.35029556809977,0.0784482631732989,
5.96255899329468));
#24352=CARTESIAN_POINT('Ctrl Pts',(-2.33837673152359,0.278307182225817,
6.05351208294933));
#24353=CARTESIAN_POINT('Ctrl Pts',(-2.32645789494741,0.410225452513894,
6.22905017565613));
#24354=CARTESIAN_POINT('Ctrl Pts',(-2.31453905837123,0.44199904405737,6.44632072344216));
#24355=CARTESIAN_POINT('Ctrl Pts',(-2.30262022179505,0.365871353323644,
6.65228340628776));
#24356=CARTESIAN_POINT('Ctrl Pts',(-2.29070138521887,0.200426754466599,
6.79665839279099));
#24357=CARTESIAN_POINT('Ctrl Pts',(-2.27878254864269,-0.0139462398915382,
6.84420070524297));
#24358=CARTESIAN_POINT('Ctrl Pts',(-2.26686371206651,-0.22491466192665,
6.78330426464398));
#24359=CARTESIAN_POINT('Ctrl Pts',(-2.25494487549033,-0.380976677383177,
6.62883517243736));
#24360=CARTESIAN_POINT('Ctrl Pts',(-2.24302603891415,-0.444034250759953,
6.41850259637544));
#24361=CARTESIAN_POINT('Ctrl Pts',(-2.23110720233797,-0.398693717462841,
6.2036531366181));
#24362=CARTESIAN_POINT('Ctrl Pts',(-2.2191883657618,-0.256023618390257,
6.03673610582583));
#24363=CARTESIAN_POINT('Ctrl Pts',(-2.20726952918561,-0.0508528152492455,
5.95849940154143));
#24364=CARTESIAN_POINT('Ctrl Pts',(-2.19535069260944,0.166732354860172,
5.9880423976207));
#24365=CARTESIAN_POINT('Ctrl Pts',(-2.18343185603326,0.343614379006663,
6.11815271293568));
#24366=CARTESIAN_POINT('Ctrl Pts',(-2.17151301945708,0.436613462550383,
6.31706835063465));
#24367=CARTESIAN_POINT('Ctrl Pts',(-2.1595941828809,0.423024781800764,6.53622835915532));
#24368=CARTESIAN_POINT('Ctrl Pts',(-2.14767534630472,0.306169516667542,
6.72213427237698));
#24369=CARTESIAN_POINT('Ctrl Pts',(-2.13575650972854,0.114566348266639,
6.8293957762013));
#24370=CARTESIAN_POINT('Ctrl Pts',(-2.12383767315236,-0.104991687963572,
6.83184231737557));
#24371=CARTESIAN_POINT('Ctrl Pts',(-2.11191883657618,-0.298941071897694,
6.72884444417467));
#24372=CARTESIAN_POINT('Ctrl Pts',(-2.10397294552539,-0.379532422064226,
6.60668793422461));
#24373=CARTESIAN_POINT('Ctrl Pts',(-2.1,-0.402774227945242,6.53965891057542));
#24374=CARTESIAN_POINT('Ctrl Pts',(-2.1,-0.402774227945242,6.53965891057542));
#24375=CARTESIAN_POINT('Ctrl Pts',(-2.1,-0.398484638758285,6.55741240483299));
#24376=CARTESIAN_POINT('Ctrl Pts',(-2.1,-0.393037299189535,6.57484669319261));
#24377=CARTESIAN_POINT('Ctrl Pts',(-2.1,-0.386509552509357,6.59187123411703));
#24378=CARTESIAN_POINT('Ctrl Pts',(-2.1,-0.381753507363848,6.60427512924121));
#24379=CARTESIAN_POINT('Ctrl Pts',(-2.1,-0.376423475271725,6.61646161573661));
#24380=CARTESIAN_POINT('Ctrl Pts',(-2.1,-0.370542725187782,6.62839523023791));
#24381=CARTESIAN_POINT('Ctrl Pts',(-2.1,-0.367213725298235,6.63515066122709));
#24382=CARTESIAN_POINT('Ctrl Pts',(-2.1,-0.363707525435473,6.6418256648993));
#24383=CARTESIAN_POINT('Ctrl Pts',(-2.1,-0.360036351586671,6.64839942538541));
#24384=CARTESIAN_POINT('Ctrl Pts',(-2.1,-0.35176296808893,6.66321409877431));
#24385=CARTESIAN_POINT('Ctrl Pts',(-2.1,-0.342644371178579,6.67753242868165));
#24386=CARTESIAN_POINT('Ctrl Pts',(-2.1,-0.332730966942087,6.69128302674014));
#24387=CARTESIAN_POINT('Ctrl Pts',(-2.1,-0.326097681493147,6.70048386631449));
#24388=CARTESIAN_POINT('Ctrl Pts',(-2.1,-0.319108257560132,6.70943048957354));
#24389=CARTESIAN_POINT('Ctrl Pts',(-2.1,-0.311774677324918,6.7181003705903));
#24390=CARTESIAN_POINT('Ctrl Pts',(-2.1,-0.308148267079993,6.7223875733389));
#24391=CARTESIAN_POINT('Ctrl Pts',(-2.1,-0.304437253383367,6.7266073471557));
#24392=CARTESIAN_POINT('Ctrl Pts',(-2.1,-0.30065086413981,6.73074867775903));
#24393=CARTESIAN_POINT('Ctrl Pts',(-2.1,-0.284450150446919,6.74846806873983));
#24394=CARTESIAN_POINT('Ctrl Pts',(-2.1,-0.26684239953173,6.76479115222895));
#24395=CARTESIAN_POINT('Ctrl Pts',(-2.1,-0.24806300232608,6.77963444611442));
#24396=CARTESIAN_POINT('Ctrl Pts',(-2.1,-0.229015002355758,6.79469004445943));
#24397=CARTESIAN_POINT('Ctrl Pts',(-2.1,-0.208760629118366,6.80822418203225));
#24398=CARTESIAN_POINT('Ctrl Pts',(-2.1,-0.187501868003905,6.82011881527523));
#24399=CARTESIAN_POINT('Ctrl Pts',(-2.1,-0.182121127272195,6.8231294299218));
#24400=CARTESIAN_POINT('Ctrl Pts',(-2.1,-0.176675868974013,6.82603481851803));
#24401=CARTESIAN_POINT('Ctrl Pts',(-2.1,-0.171169051786272,6.82883264150109));
#24402=CARTESIAN_POINT('Ctrl Pts',(-2.1,-0.165595855256536,6.83166418952754));
#24403=CARTESIAN_POINT('Ctrl Pts',(-2.1,-0.159966248284264,6.83438207494035));
#24404=CARTESIAN_POINT('Ctrl Pts',(-2.1,-0.154290568068188,6.83698163141168));
#24405=CARTESIAN_POINT('Ctrl Pts',(-2.1,-0.139973144289019,6.84353925097815));
#24406=CARTESIAN_POINT('Ctrl Pts',(-2.1,-0.1253500812197,6.84935087179354));
#24407=CARTESIAN_POINT('Ctrl Pts',(-2.1,-0.110478871969928,6.85439100862466));
#24408=CARTESIAN_POINT('Ctrl Pts',(-2.1,-0.091606231881728,6.86078730678786));
#24409=CARTESIAN_POINT('Ctrl Pts',(-2.1,-0.0723341026865624,6.8659419398207));
#24410=CARTESIAN_POINT('Ctrl Pts',(-2.1,-0.0527866493565085,6.86986556285165));
#24411=CARTESIAN_POINT('Ctrl Pts',(-2.1,-0.0364584381349322,6.87314301002196));
#24412=CARTESIAN_POINT('Ctrl Pts',(-2.1,-0.0199377431301133,6.87556121981262));
#24413=CARTESIAN_POINT('Ctrl Pts',(-2.1,-0.00329277923049777,6.87711561177094));
#24414=CARTESIAN_POINT('Ctrl Pts',(-2.1,0.00380833581134274,6.87777875025432));
#24415=CARTESIAN_POINT('Ctrl Pts',(-2.1,0.010934154274537,6.87828439261757));
#24416=CARTESIAN_POINT('Ctrl Pts',(-2.1,0.0180564268157742,6.87863124049195));
#24417=CARTESIAN_POINT('Ctrl Pts',(-2.1,0.0436614570733077,6.87987818102488));
#24418=CARTESIAN_POINT('Ctrl Pts',(-2.1,0.0692830486968658,6.87908401838085));
#24419=CARTESIAN_POINT('Ctrl Pts',(-2.1,0.0946701039420577,6.87627112264398));
#24420=CARTESIAN_POINT('Ctrl Pts',(-2.1,0.105116630998588,6.87511364332475));
#24421=CARTESIAN_POINT('Ctrl Pts',(-2.1,0.115523671677657,6.87361376587106));
#24422=CARTESIAN_POINT('Ctrl Pts',(-2.1,0.125874323021446,6.87177056809269));
#24423=CARTESIAN_POINT('Ctrl Pts',(-2.1,0.138413824297786,6.86953758969098));
#24424=CARTESIAN_POINT('Ctrl Pts',(-2.1,0.150870601134534,6.86680082502239));
#24425=CARTESIAN_POINT('Ctrl Pts',(-2.1,0.163219456840939,6.86357425405869));
#24426=CARTESIAN_POINT('Ctrl Pts',(-2.1,0.170695776276485,6.8616208038136));
#24427=CARTESIAN_POINT('Ctrl Pts',(-2.1,0.178132534318461,6.85948775559199));
#24428=CARTESIAN_POINT('Ctrl Pts',(-2.1,0.185524032856684,6.85717764382782));
#24429=CARTESIAN_POINT('Ctrl Pts',(-2.1,0.191333634449564,6.85536193231609));
#24430=CARTESIAN_POINT('Ctrl Pts',(-2.1,0.197115271577026,6.85343663586951));
#24431=CARTESIAN_POINT('Ctrl Pts',(-2.1,0.202852164838079,6.85140831852427));
#24432=CARTESIAN_POINT('Ctrl Pts',(-2.1,0.227408324506361,6.84272632248192));
#24433=CARTESIAN_POINT('Ctrl Pts',(-2.1,0.251209399850707,6.83214163505072));
#24434=CARTESIAN_POINT('Ctrl Pts',(-2.1,0.274050638756253,6.81980030995607));
#24435=CARTESIAN_POINT('Ctrl Pts',(-2.1,0.297081928279728,6.80735629881755));
#24436=CARTESIAN_POINT('Ctrl Pts',(-2.1,0.319138676313367,6.79312590368834));
#24437=CARTESIAN_POINT('Ctrl Pts',(-2.1,0.33999937244817,6.77720843590635));
#24438=CARTESIAN_POINT('Ctrl Pts',(-2.1,0.343569976374306,6.77448393560256));
#24439=CARTESIAN_POINT('Ctrl Pts',(-2.1,0.347105483833496,6.77170989850117));
#24440=CARTESIAN_POINT('Ctrl Pts',(-2.1,0.350604705166974,6.76888668926355));
#24441=CARTESIAN_POINT('Ctrl Pts',(-2.1,0.353884815611532,6.76624026103711));
#24442=CARTESIAN_POINT('Ctrl Pts',(-2.1,0.357133041678995,6.76355062538503));
#24443=CARTESIAN_POINT('Ctrl Pts',(-2.1,0.360348823959175,6.76081852140068));
#24444=CARTESIAN_POINT('Ctrl Pts',(-2.46703183294109,0.426306423912841,
6.39998913682467));
#24445=CARTESIAN_POINT('Ctrl Pts',(-2.46387625438919,0.426248106936643,
6.45633454115753));
#24446=CARTESIAN_POINT('Ctrl Pts',(-2.46072067583729,0.415012427400236,
6.51270250838063));
#24447=CARTESIAN_POINT('Ctrl Pts',(-2.45756509728538,0.39325469889476,6.56466465519153));
#24448=CARTESIAN_POINT('Ctrl Pts',(-2.45359215175999,0.365861221379708,
6.63008618574973));
#24449=CARTESIAN_POINT('Ctrl Pts',(-2.4496192062346,0.321788838359503,6.68852388050336));
#24450=CARTESIAN_POINT('Ctrl Pts',(-2.4456462607092,0.266417048735948,6.73284480312799));
#24451=CARTESIAN_POINT('Ctrl Pts',(-2.44167331518381,0.211045259112394,
6.77716572575262));
#24452=CARTESIAN_POINT('Ctrl Pts',(-2.43770036965842,0.144374062885491,
6.80736987624826));
#24453=CARTESIAN_POINT('Ctrl Pts',(-2.43372742413302,0.0745413820730864,
6.8197705196968));
#24454=CARTESIAN_POINT('Ctrl Pts',(-2.42975447860763,0.00470870126068151,
6.83217116314535));
#24455=CARTESIAN_POINT('Ctrl Pts',(-2.42578153308224,-0.0682854641372245,
6.82676829954679));
#24456=CARTESIAN_POINT('Ctrl Pts',(-2.42180858755684,-0.135531407000747,
6.80422140536676));
#24457=CARTESIAN_POINT('Ctrl Pts',(-2.41783564203145,-0.202777349864269,
6.78167451118673));
#24458=CARTESIAN_POINT('Ctrl Pts',(-2.41386269650606,-0.264275070193409,
6.74198358642523));
#24459=CARTESIAN_POINT('Ctrl Pts',(-2.40988975098066,-0.312518123176517,
6.68999332669579));
#24460=CARTESIAN_POINT('Ctrl Pts',(-2.40591680545527,-0.360761176159625,
6.63800306696635));
#24461=CARTESIAN_POINT('Ctrl Pts',(-2.40194385992988,-0.395749561796702,
6.57371347226898));
#24462=CARTESIAN_POINT('Ctrl Pts',(-2.39797091440449,-0.413212578910154,
6.50497176512118));
#24463=CARTESIAN_POINT('Ctrl Pts',(-2.39399796887909,-0.430675596023606,
6.43623005797338));
#24464=CARTESIAN_POINT('Ctrl Pts',(-2.3900250233537,-0.430613244613433,
6.36303623837515));
#24465=CARTESIAN_POINT('Ctrl Pts',(-2.38605207782831,-0.413033135329271,
6.29432438331576));
#24466=CARTESIAN_POINT('Ctrl Pts',(-2.38207913230291,-0.395453026045109,
6.22561252825636));
#24467=CARTESIAN_POINT('Ctrl Pts',(-2.37810618677752,-0.360355158886957,
6.16138263773582));
#24468=CARTESIAN_POINT('Ctrl Pts',(-2.37413324125213,-0.312023598397992,
6.10947464674327));
#24469=CARTESIAN_POINT('Ctrl Pts',(-2.37016029572673,-0.263692037909028,
6.05756665575072));
#24470=CARTESIAN_POINT('Ctrl Pts',(-2.36618735020134,-0.20212678408925,
6.01798056428618));
#24471=CARTESIAN_POINT('Ctrl Pts',(-2.36221440467595,-0.1348425249389,5.99554827196608));
#24472=CARTESIAN_POINT('Ctrl Pts',(-2.35824145915055,-0.0675582657885491,
5.97311597964598));
#24473=CARTESIAN_POINT('Ctrl Pts',(-2.35426851362516,0.00544499869237483,
5.96783748647033));
#24474=CARTESIAN_POINT('Ctrl Pts',(-2.35029556809977,0.0752564507749232,
5.98035708815828));
#24475=CARTESIAN_POINT('Ctrl Pts',(-2.34632262257437,0.145067902857471,
5.99287668984623));
#24476=CARTESIAN_POINT('Ctrl Pts',(-2.34234967704898,0.211687542541645,
6.02319438639778));
#24477=CARTESIAN_POINT('Ctrl Pts',(-2.33837673152359,0.266983740765077,
6.06760958345802));
#24478=CARTESIAN_POINT('Ctrl Pts',(-2.33440378599819,0.322279938988509,
6.11202478051826));
#24479=CARTESIAN_POINT('Ctrl Pts',(-2.3304308404728,0.366252695751201,6.17053747808719));
#24480=CARTESIAN_POINT('Ctrl Pts',(-2.32645789494741,0.393534672723127,
6.236005584836));
#24481=CARTESIAN_POINT('Ctrl Pts',(-2.32331587427864,0.415110738889366,
6.28778131224916));
#24482=CARTESIAN_POINT('Ctrl Pts',(-2.32017385360987,0.4262475506417,6.34390730291496));
#24483=CARTESIAN_POINT('Ctrl Pts',(-2.31703183294109,0.426305653513777,
6.40001091236462));
#24484=CARTESIAN_POINT('Ctrl Pts',(-2.6,0.132288496556895,5.90755938055567));
#24485=CARTESIAN_POINT('Ctrl Pts',(-2.6,0.157089924837099,5.91642640455182));
#24486=CARTESIAN_POINT('Ctrl Pts',(-2.6,0.181088073064976,5.9272189255245));
#24487=CARTESIAN_POINT('Ctrl Pts',(-2.6,0.204091900162786,5.93978802247808));
#24488=CARTESIAN_POINT('Ctrl Pts',(-2.6,0.226981614101412,5.95229476896469));
#24489=CARTESIAN_POINT('Ctrl Pts',(-2.6,0.248887897831876,5.96656143458844));
#24490=CARTESIAN_POINT('Ctrl Pts',(-2.6,0.269590200964406,5.98248076289354));
#24491=CARTESIAN_POINT('Ctrl Pts',(-2.6,0.276528918772376,5.98781638792494));
#24492=CARTESIAN_POINT('Ctrl Pts',(-2.6,0.283332046569503,5.99333793609881));
#24493=CARTESIAN_POINT('Ctrl Pts',(-2.6,0.289990147837974,5.99904209573216));
#24494=CARTESIAN_POINT('Ctrl Pts',(-2.6,0.296028106433828,6.00421496383698));
#24495=CARTESIAN_POINT('Ctrl Pts',(-2.6,0.301949771037903,6.00954116989861));
#24496=CARTESIAN_POINT('Ctrl Pts',(-2.6,0.307727671725424,6.01499858003089));
#24497=CARTESIAN_POINT('Ctrl Pts',(-2.6,0.318182122624537,6.02487313990129));
#24498=CARTESIAN_POINT('Ctrl Pts',(-2.6,0.32817930410564,6.03518740593773));
#24499=CARTESIAN_POINT('Ctrl Pts',(-2.6,0.337684947200095,6.04592058651842));
#24500=CARTESIAN_POINT('Ctrl Pts',(-2.6,0.35463663907465,6.06506138196275));
#24501=CARTESIAN_POINT('Ctrl Pts',(-2.6,0.370027957593029,6.08553349763026));
#24502=CARTESIAN_POINT('Ctrl Pts',(-2.6,0.383735216002276,6.10712564152075));
#24503=CARTESIAN_POINT('Ctrl Pts',(-2.6,0.39189872132373,6.11998507528124));
#24504=CARTESIAN_POINT('Ctrl Pts',(-2.6,0.399464029634324,6.13324224816933));
#24505=CARTESIAN_POINT('Ctrl Pts',(-2.6,0.406396423774992,6.1468545793287));
#24506=CARTESIAN_POINT('Ctrl Pts',(-2.6,0.409857954474058,6.15365158210118));
#24507=CARTESIAN_POINT('Ctrl Pts',(-2.6,0.413162930739684,6.16054073803517));
#24508=CARTESIAN_POINT('Ctrl Pts',(-2.6,0.416296070484027,6.16749212337976));
#24509=CARTESIAN_POINT('Ctrl Pts',(-2.6,0.426533299061843,6.19020509710957));
#24510=CARTESIAN_POINT('Ctrl Pts',(-2.6,0.434966161858725,6.21362881910558));
#24511=CARTESIAN_POINT('Ctrl Pts',(-2.6,0.441477406647537,6.23756556523482));
#24512=CARTESIAN_POINT('Ctrl Pts',(-2.6,0.443239379224161,6.24404295805621));
#24513=CARTESIAN_POINT('Ctrl Pts',(-2.6,0.444860350146518,6.25055797543335));
#24514=CARTESIAN_POINT('Ctrl Pts',(-2.6,0.44633733619218,6.25710677385474));
#24515=CARTESIAN_POINT('Ctrl Pts',(-2.6,0.450544524902758,6.27576099937518));
#24516=CARTESIAN_POINT('Ctrl Pts',(-2.6,0.453584703119787,6.29468965910361));
#24517=CARTESIAN_POINT('Ctrl Pts',(-2.6,0.455444326288054,6.31378084410223));
#24518=CARTESIAN_POINT('Ctrl Pts',(-2.6,0.456025440853221,6.31974665796081));
#24519=CARTESIAN_POINT('Ctrl Pts',(-2.6,0.456491144811005,6.32572830613997));
#24520=CARTESIAN_POINT('Ctrl Pts',(-2.6,0.456840676091559,6.33172224529114));
#24521=CARTESIAN_POINT('Ctrl Pts',(-2.6,0.457162778165346,6.33724581453417));
#24522=CARTESIAN_POINT('Ctrl Pts',(-2.6,0.457385661676131,6.34277019876787));
#24523=CARTESIAN_POINT('Ctrl Pts',(-2.6,0.457509644065614,6.34829248285953));
#24524=CARTESIAN_POINT('Ctrl Pts',(-2.6,0.458052816417877,6.37248585461552));
#24525=CARTESIAN_POINT('Ctrl Pts',(-2.6,0.456701759624391,6.39664121290135));
#24526=CARTESIAN_POINT('Ctrl Pts',(-2.6,0.453453339531317,6.42053138158929));
#24527=CARTESIAN_POINT('Ctrl Pts',(-2.6,0.450523324248874,6.44207987511851));
#24528=CARTESIAN_POINT('Ctrl Pts',(-2.6,0.446048919178311,6.46341331208366));
#24529=CARTESIAN_POINT('Ctrl Pts',(-2.6,0.439994176553064,6.48435098741415));
#24530=CARTESIAN_POINT('Ctrl Pts',(-2.6,0.438094472520504,6.49092028172105));
#24531=CARTESIAN_POINT('Ctrl Pts',(-2.6,0.436038962655861,6.4974504658391));
#24532=CARTESIAN_POINT('Ctrl Pts',(-2.6,0.43382941905493,6.50393615250028));
#24533=CARTESIAN_POINT('Ctrl Pts',(-2.6,0.431714290768034,6.5101447013206));
#24534=CARTESIAN_POINT('Ctrl Pts',(-2.6,0.42946061872238,6.5163046335942));
#24535=CARTESIAN_POINT('Ctrl Pts',(-2.6,0.427072414698455,6.5224077707279));
#24536=CARTESIAN_POINT('Ctrl Pts',(-2.6,0.421492488317325,6.53666746360122));
#24537=CARTESIAN_POINT('Ctrl Pts',(-2.6,0.415176231857449,6.5506245268354));
#24538=CARTESIAN_POINT('Ctrl Pts',(-2.6,0.408152204549093,6.56422236660796));
#24539=CARTESIAN_POINT('Ctrl Pts',(-2.6,0.402591346359437,6.57498765201209));
#24540=CARTESIAN_POINT('Ctrl Pts',(-2.6,0.396586710322636,6.58552771963742));
#24541=CARTESIAN_POINT('Ctrl Pts',(-2.6,0.390149689096489,6.59581166017504));
#24542=CARTESIAN_POINT('Ctrl Pts',(-2.6,0.386403333843806,6.6017969277853));
#24543=CARTESIAN_POINT('Ctrl Pts',(-2.6,0.382511806820547,6.60769294534655));
#24544=CARTESIAN_POINT('Ctrl Pts',(-2.6,0.378483683496843,6.61348517016826));
#24545=CARTESIAN_POINT('Ctrl Pts',(-2.6,0.365269544048599,6.63248639241469));
#24546=CARTESIAN_POINT('Ctrl Pts',(-2.6,0.350570496167934,6.65040177272496));
#24547=CARTESIAN_POINT('Ctrl Pts',(-2.6,0.334470605331163,6.66701291851188));
#24548=CARTESIAN_POINT('Ctrl Pts',(-2.6,0.332980284132811,6.66855056512987));
#24549=CARTESIAN_POINT('Ctrl Pts',(-2.6,0.331477939680677,6.67007700481367));
#24550=CARTESIAN_POINT('Ctrl Pts',(-2.6,0.329963627179693,6.67159204424712));
#24551=CARTESIAN_POINT('Ctrl Pts',(-2.6,0.327462974104075,6.67409389773937));
#24552=CARTESIAN_POINT('Ctrl Pts',(-2.6,0.324929685151723,6.67656466471947));
#24553=CARTESIAN_POINT('Ctrl Pts',(-2.6,0.322364416527274,6.67900379523474));
#24554=CARTESIAN_POINT('Origin',(2.35,0.,6.4));
#24555=CARTESIAN_POINT('Origin',(2.1,0.,6.4));
#24556=CARTESIAN_POINT('',(2.1,-0.4,6.4));
#24557=CARTESIAN_POINT('Origin',(2.1,0.,6.4));
#24558=CARTESIAN_POINT('Origin',(1.9,0.,6.4));
#24559=CARTESIAN_POINT('',(1.2,-0.4,6.4));
#24560=CARTESIAN_POINT('',(1.9,-0.4,6.4));
#24561=CARTESIAN_POINT('Origin',(1.2,0.,6.4));
#24562=CARTESIAN_POINT('Origin',(1.2,0.,6.4));
#24563=CARTESIAN_POINT('',(1.2,-0.2,6.4));
#24564=CARTESIAN_POINT('Origin',(1.2,0.,6.4));
#24565=CARTESIAN_POINT('Origin',(1.55,0.,6.4));
#24566=CARTESIAN_POINT('',(0.565685424949238,-0.2,6.4));
#24567=CARTESIAN_POINT('',(1.55,-0.2,6.4));
#24568=CARTESIAN_POINT('',(0.565685424949238,0.2,6.4));
#24569=CARTESIAN_POINT('Ctrl Pts',(0.565685424949238,0.2,6.4));
#24570=CARTESIAN_POINT('Ctrl Pts',(0.565685424949238,0.2,6.42532921208158));
#24571=CARTESIAN_POINT('Ctrl Pts',(0.567565356574251,0.194898067853762,
6.45220039469271));
#24572=CARTESIAN_POINT('Ctrl Pts',(0.574186082552466,0.17443058152527,6.50141063599154));
#24573=CARTESIAN_POINT('Ctrl Pts',(0.578813771212597,0.159074095999941,
6.52376861647468));
#24574=CARTESIAN_POINT('Ctrl Pts',(0.587374622031365,0.123776803829002,
6.55906590864562));
#24575=CARTESIAN_POINT('Ctrl Pts',(0.59188739106068,0.101415562391481,6.57442869722332));
#24576=CARTESIAN_POINT('Ctrl Pts',(0.598240475886912,0.0521932274441716,
6.59490088416061));
#24577=CARTESIAN_POINT('Ctrl Pts',(0.6,0.0253174643734703,6.6));
#24578=CARTESIAN_POINT('Ctrl Pts',(0.6,-0.0253174643734703,6.6));
#24579=CARTESIAN_POINT('Ctrl Pts',(0.598240475886912,-0.0521932274441708,
6.59490088416061));
#24580=CARTESIAN_POINT('Ctrl Pts',(0.59188739106068,-0.10141556239148,6.57442869722332));
#24581=CARTESIAN_POINT('Ctrl Pts',(0.587374622031365,-0.123776803829002,
6.55906590864562));
#24582=CARTESIAN_POINT('Ctrl Pts',(0.578813771212597,-0.159074095999941,
6.52376861647468));
#24583=CARTESIAN_POINT('Ctrl Pts',(0.574186082552466,-0.17443058152527,
6.50141063599154));
#24584=CARTESIAN_POINT('Ctrl Pts',(0.567565356574251,-0.194898067853762,
6.45220039469271));
#24585=CARTESIAN_POINT('Ctrl Pts',(0.565685424949238,-0.2,6.42532921208158));
#24586=CARTESIAN_POINT('Ctrl Pts',(0.565685424949238,-0.2,6.4));
#24587=CARTESIAN_POINT('Ctrl Pts',(0.565685424949238,-0.2,6.4));
#24588=CARTESIAN_POINT('Ctrl Pts',(0.565685424949238,-0.2,6.37467078791842));
#24589=CARTESIAN_POINT('Ctrl Pts',(0.567565356574251,-0.194898067853762,
6.3477996053073));
#24590=CARTESIAN_POINT('Ctrl Pts',(0.574186082552466,-0.17443058152527,
6.29858936400846));
#24591=CARTESIAN_POINT('Ctrl Pts',(0.578813771212597,-0.159074095999941,
6.27623138352532));
#24592=CARTESIAN_POINT('Ctrl Pts',(0.587374622031365,-0.123776803829002,
6.24093409135438));
#24593=CARTESIAN_POINT('Ctrl Pts',(0.59188739106068,-0.101415562391481,
6.22557130277668));
#24594=CARTESIAN_POINT('Ctrl Pts',(0.598240475886912,-0.0521932274441716,
6.20509911583939));
#24595=CARTESIAN_POINT('Ctrl Pts',(0.6,-0.0253174643734704,6.2));
#24596=CARTESIAN_POINT('Ctrl Pts',(0.6,0.0253174643734703,6.2));
#24597=CARTESIAN_POINT('Ctrl Pts',(0.598240475886912,0.0521932274441716,
6.20509911583939));
#24598=CARTESIAN_POINT('Ctrl Pts',(0.59188739106068,0.101415562391481,6.22557130277668));
#24599=CARTESIAN_POINT('Ctrl Pts',(0.587374622031365,0.123776803829002,
6.24093409135438));
#24600=CARTESIAN_POINT('Ctrl Pts',(0.578813771212597,0.159074095999941,
6.27623138352532));
#24601=CARTESIAN_POINT('Ctrl Pts',(0.574186082552466,0.17443058152527,6.29858936400846));
#24602=CARTESIAN_POINT('Ctrl Pts',(0.567565356574251,0.194898067853762,
6.3477996053073));
#24603=CARTESIAN_POINT('Ctrl Pts',(0.565685424949238,0.2,6.37467078791842));
#24604=CARTESIAN_POINT('Ctrl Pts',(0.565685424949238,0.2,6.4));
#24605=CARTESIAN_POINT('Origin',(2.,0.,6.4));
#24606=CARTESIAN_POINT('',(2.37276210354093,0.3605551275464,5.8));
#24607=CARTESIAN_POINT('',(2.6,0.3605551275464,5.8));
#24608=CARTESIAN_POINT('',(2.,0.3605551275464,5.8));
#24609=CARTESIAN_POINT('Ctrl Pts',(2.33023603954621,0.574456264653803,6.8));
#24610=CARTESIAN_POINT('Ctrl Pts',(2.3232708588146,0.602709964998632,6.75942371209316));
#24611=CARTESIAN_POINT('Ctrl Pts',(2.31670997613269,0.627102242782997,6.71508313975596));
#24612=CARTESIAN_POINT('Ctrl Pts',(2.30129622342295,0.682214955011516,6.58244341832651));
#24613=CARTESIAN_POINT('Ctrl Pts',(2.2956480566498,0.7,6.48846273735544));
#24614=CARTESIAN_POINT('Ctrl Pts',(2.2956480566498,0.7,6.4));
#24615=CARTESIAN_POINT('Ctrl Pts',(2.2956480566498,0.7,6.31153726264456));
#24616=CARTESIAN_POINT('Ctrl Pts',(2.30129622342295,0.682214955011516,6.21755658167349));
#24617=CARTESIAN_POINT('Ctrl Pts',(2.32131846716735,0.610624332115547,6.04525948552425));
#24618=CARTESIAN_POINT('Ctrl Pts',(2.3353634864858,0.556843997628587,5.96689450396742));
#24619=CARTESIAN_POINT('Ctrl Pts',(2.35662323311261,0.455977300410207,5.86602780674904));
#24620=CARTESIAN_POINT('Ctrl Pts',(2.36516699585665,0.410537452879607,5.83003563947597));
#24621=CARTESIAN_POINT('Ctrl Pts',(2.37276210354093,0.3605551275464,5.8));
#24622=CARTESIAN_POINT('Origin',(2.,0.,6.4));
#24623=CARTESIAN_POINT('',(2.37276210354093,-0.3605551275464,5.8));
#24624=CARTESIAN_POINT('Ctrl Pts',(2.37276210354093,-0.3605551275464,5.8));
#24625=CARTESIAN_POINT('Ctrl Pts',(2.36516699585665,-0.410537452879608,
5.83003563947597));
#24626=CARTESIAN_POINT('Ctrl Pts',(2.35662323311261,-0.455977300410207,
5.86602780674904));
#24627=CARTESIAN_POINT('Ctrl Pts',(2.3353634864858,-0.556843997628587,5.96689450396742));
#24628=CARTESIAN_POINT('Ctrl Pts',(2.32131846716735,-0.610624332115547,
6.04525948552425));
#24629=CARTESIAN_POINT('Ctrl Pts',(2.30129622342295,-0.682214955011516,
6.21755658167349));
#24630=CARTESIAN_POINT('Ctrl Pts',(2.2956480566498,-0.7,6.31153726264456));
#24631=CARTESIAN_POINT('Ctrl Pts',(2.2956480566498,-0.7,6.48846273735544));
#24632=CARTESIAN_POINT('Ctrl Pts',(2.30129622342295,-0.682214955011516,
6.58244341832651));
#24633=CARTESIAN_POINT('Ctrl Pts',(2.31670997613269,-0.627102242782997,
6.71508313975596));
#24634=CARTESIAN_POINT('Ctrl Pts',(2.3232708588146,-0.602709964998632,6.75942371209315));
#24635=CARTESIAN_POINT('Ctrl Pts',(2.33023603954621,-0.574456264653803,
6.8));
#24636=CARTESIAN_POINT('',(2.6,-0.3605551275464,5.8));
#24637=CARTESIAN_POINT('',(2.,-0.3605551275464,5.8));
#24638=CARTESIAN_POINT('Origin',(2.6,0.,6.4));
#24639=CARTESIAN_POINT('Origin',(2.,0.,6.4));
#24640=CARTESIAN_POINT('Origin',(2.6,0.,6.4));
#24641=CARTESIAN_POINT('',(2.6,0.,5.8));
#24642=CARTESIAN_POINT('Origin',(0.,0.,5.8));
#24643=CARTESIAN_POINT('',(-4.,2.8,5.8));
#24644=CARTESIAN_POINT('',(-4.,-2.8,5.8));
#24645=CARTESIAN_POINT('',(-4.,2.8,5.8));
#24646=CARTESIAN_POINT('',(4.,-2.8,5.8));
#24647=CARTESIAN_POINT('',(-4.,-2.8,5.8));
#24648=CARTESIAN_POINT('',(4.,2.8,5.8));
#24649=CARTESIAN_POINT('',(4.,-2.8,5.8));
#24650=CARTESIAN_POINT('',(4.,2.8,5.8));
#24651=CARTESIAN_POINT('',(3.35,-2.4,5.8));
#24652=CARTESIAN_POINT('Origin',(3.6,-2.4,5.8));
#24653=CARTESIAN_POINT('',(-3.85,-2.4,5.8));
#24654=CARTESIAN_POINT('Origin',(-3.6,-2.4,5.8));
#24655=CARTESIAN_POINT('',(-3.85,2.4,5.8));
#24656=CARTESIAN_POINT('Origin',(-3.6,2.4,5.8));
#24657=CARTESIAN_POINT('',(3.35,2.4,5.8));
#24658=CARTESIAN_POINT('Origin',(3.6,2.4,5.8));
#24659=CARTESIAN_POINT('',(-2.37276210354093,-0.3605551275464,5.8));
#24660=CARTESIAN_POINT('Origin',(0.,0.,5.8));
#24661=CARTESIAN_POINT('',(-2.6,-0.3605551275464,5.8));
#24662=CARTESIAN_POINT('',(-2.,-0.3605551275464,5.8));
#24663=CARTESIAN_POINT('',(-2.6,0.3605551275464,5.8));
#24664=CARTESIAN_POINT('',(-2.6,0.,5.8));
#24665=CARTESIAN_POINT('',(-2.37276210354093,0.3605551275464,5.8));
#24666=CARTESIAN_POINT('',(-2.,0.3605551275464,5.8));
#24667=CARTESIAN_POINT('Origin',(0.,0.,5.8));
#24668=CARTESIAN_POINT('Origin',(0.,0.,5.8));
#24669=CARTESIAN_POINT('Ctrl Pts',(-2.33023603954621,-0.574456264653803,
6.8));
#24670=CARTESIAN_POINT('Ctrl Pts',(-2.3232708588146,-0.602709964998632,
6.75942371209316));
#24671=CARTESIAN_POINT('Ctrl Pts',(-2.31670997613269,-0.627102242782997,
6.71508313975596));
#24672=CARTESIAN_POINT('Ctrl Pts',(-2.30129622342295,-0.682214955011516,
6.58244341832651));
#24673=CARTESIAN_POINT('Ctrl Pts',(-2.2956480566498,-0.7,6.48846273735544));
#24674=CARTESIAN_POINT('Ctrl Pts',(-2.2956480566498,-0.7,6.4));
#24675=CARTESIAN_POINT('Ctrl Pts',(-2.2956480566498,-0.7,6.31153726264456));
#24676=CARTESIAN_POINT('Ctrl Pts',(-2.30129622342295,-0.682214955011516,
6.21755658167349));
#24677=CARTESIAN_POINT('Ctrl Pts',(-2.32131846716735,-0.610624332115547,
6.04525948552425));
#24678=CARTESIAN_POINT('Ctrl Pts',(-2.3353634864858,-0.556843997628587,
5.96689450396742));
#24679=CARTESIAN_POINT('Ctrl Pts',(-2.35662323311261,-0.455977300410207,
5.86602780674904));
#24680=CARTESIAN_POINT('Ctrl Pts',(-2.36516699585665,-0.410537452879607,
5.83003563947597));
#24681=CARTESIAN_POINT('Ctrl Pts',(-2.37276210354093,-0.3605551275464,5.8));
#24682=CARTESIAN_POINT('Origin',(-2.35,0.,6.4));
#24683=CARTESIAN_POINT('Origin',(-2.1,0.,6.4));
#24684=CARTESIAN_POINT('',(-2.1,0.4,6.4));
#24685=CARTESIAN_POINT('Origin',(-2.1,0.,6.4));
#24686=CARTESIAN_POINT('Origin',(-1.9,0.,6.4));
#24687=CARTESIAN_POINT('',(-1.2,0.4,6.4));
#24688=CARTESIAN_POINT('',(-1.9,0.4,6.4));
#24689=CARTESIAN_POINT('Origin',(-1.2,0.,6.4));
#24690=CARTESIAN_POINT('Origin',(-1.2,0.,6.4));
#24691=CARTESIAN_POINT('',(-1.2,0.2,6.4));
#24692=CARTESIAN_POINT('Origin',(-1.2,0.,6.4));
#24693=CARTESIAN_POINT('Origin',(-1.55,0.,6.4));
#24694=CARTESIAN_POINT('',(-0.565685424949238,0.2,6.4));
#24695=CARTESIAN_POINT('',(-1.55,0.2,6.4));
#24696=CARTESIAN_POINT('',(-0.6,1.93921692146525E-17,6.6));
#24697=CARTESIAN_POINT('Ctrl Pts',(-0.6,-2.77555756156289E-17,6.6));
#24698=CARTESIAN_POINT('Ctrl Pts',(-0.6,0.0253174643734703,6.6));
#24699=CARTESIAN_POINT('Ctrl Pts',(-0.598240475886912,0.0521932274441708,
6.59490088416061));
#24700=CARTESIAN_POINT('Ctrl Pts',(-0.59188739106068,0.10141556239148,6.57442869722332));
#24701=CARTESIAN_POINT('Ctrl Pts',(-0.587374622031365,0.123776803829002,
6.55906590864562));
#24702=CARTESIAN_POINT('Ctrl Pts',(-0.578813771212597,0.159074095999941,
6.52376861647468));
#24703=CARTESIAN_POINT('Ctrl Pts',(-0.574186082552466,0.17443058152527,
6.50141063599154));
#24704=CARTESIAN_POINT('Ctrl Pts',(-0.567565356574251,0.194898067853762,
6.45220039469271));
#24705=CARTESIAN_POINT('Ctrl Pts',(-0.565685424949238,0.2,6.42532921208158));
#24706=CARTESIAN_POINT('Ctrl Pts',(-0.565685424949238,0.2,6.4));
#24707=CARTESIAN_POINT('',(-0.565685424949238,-0.2,6.4));
#24708=CARTESIAN_POINT('Ctrl Pts',(-0.565685424949238,-0.2,6.4));
#24709=CARTESIAN_POINT('Ctrl Pts',(-0.565685424949238,-0.2,6.42532921208158));
#24710=CARTESIAN_POINT('Ctrl Pts',(-0.567565356574251,-0.194898067853762,
6.45220039469271));
#24711=CARTESIAN_POINT('Ctrl Pts',(-0.574186082552466,-0.17443058152527,
6.50141063599154));
#24712=CARTESIAN_POINT('Ctrl Pts',(-0.578813771212597,-0.159074095999941,
6.52376861647468));
#24713=CARTESIAN_POINT('Ctrl Pts',(-0.587374622031365,-0.123776803829002,
6.55906590864562));
#24714=CARTESIAN_POINT('Ctrl Pts',(-0.59188739106068,-0.101415562391481,
6.57442869722332));
#24715=CARTESIAN_POINT('Ctrl Pts',(-0.598240475886912,-0.0521932274441716,
6.59490088416061));
#24716=CARTESIAN_POINT('Ctrl Pts',(-0.6,-0.0253174643734703,6.6));
#24717=CARTESIAN_POINT('Ctrl Pts',(-0.6,2.08166817117217E-17,6.6));
#24718=CARTESIAN_POINT('',(-0.6,1.59227222626989E-17,6.2));
#24719=CARTESIAN_POINT('Ctrl Pts',(-0.6,-4.85722573273506E-17,6.2));
#24720=CARTESIAN_POINT('Ctrl Pts',(-0.6,-0.0253174643734703,6.2));
#24721=CARTESIAN_POINT('Ctrl Pts',(-0.598240475886912,-0.0521932274441716,
6.20509911583939));
#24722=CARTESIAN_POINT('Ctrl Pts',(-0.59188739106068,-0.101415562391481,
6.22557130277668));
#24723=CARTESIAN_POINT('Ctrl Pts',(-0.587374622031365,-0.123776803829002,
6.24093409135438));
#24724=CARTESIAN_POINT('Ctrl Pts',(-0.578813771212597,-0.159074095999941,
6.27623138352532));
#24725=CARTESIAN_POINT('Ctrl Pts',(-0.574186082552466,-0.17443058152527,
6.29858936400846));
#24726=CARTESIAN_POINT('Ctrl Pts',(-0.567565356574251,-0.194898067853762,
6.3477996053073));
#24727=CARTESIAN_POINT('Ctrl Pts',(-0.565685424949238,-0.2,6.37467078791842));
#24728=CARTESIAN_POINT('Ctrl Pts',(-0.565685424949238,-0.2,6.4));
#24729=CARTESIAN_POINT('Ctrl Pts',(-0.565685424949238,0.2,6.4));
#24730=CARTESIAN_POINT('Ctrl Pts',(-0.565685424949238,0.2,6.37467078791842));
#24731=CARTESIAN_POINT('Ctrl Pts',(-0.567565356574251,0.194898067853762,
6.3477996053073));
#24732=CARTESIAN_POINT('Ctrl Pts',(-0.574186082552466,0.17443058152527,
6.29858936400846));
#24733=CARTESIAN_POINT('Ctrl Pts',(-0.578813771212597,0.159074095999941,
6.27623138352532));
#24734=CARTESIAN_POINT('Ctrl Pts',(-0.587374622031365,0.123776803829002,
6.24093409135438));
#24735=CARTESIAN_POINT('Ctrl Pts',(-0.59188739106068,0.101415562391481,
6.22557130277668));
#24736=CARTESIAN_POINT('Ctrl Pts',(-0.598240475886912,0.0521932274441716,
6.20509911583939));
#24737=CARTESIAN_POINT('Ctrl Pts',(-0.6,0.0253174643734703,6.2));
#24738=CARTESIAN_POINT('Ctrl Pts',(-0.6,-2.77555756156289E-17,6.2));
#24739=CARTESIAN_POINT('Origin',(-2.6,0.,6.4));
#24740=CARTESIAN_POINT('Origin',(-2.6,0.,6.4));
#24741=CARTESIAN_POINT('Origin',(-2.,0.,6.4));
#24742=CARTESIAN_POINT('Ctrl Pts',(-2.37276210354093,0.3605551275464,5.8));
#24743=CARTESIAN_POINT('Ctrl Pts',(-2.36516699585665,0.410537452879608,
5.83003563947597));
#24744=CARTESIAN_POINT('Ctrl Pts',(-2.35662323311261,0.455977300410207,
5.86602780674904));
#24745=CARTESIAN_POINT('Ctrl Pts',(-2.3353634864858,0.556843997628587,5.96689450396742));
#24746=CARTESIAN_POINT('Ctrl Pts',(-2.32131846716735,0.610624332115547,
6.04525948552425));
#24747=CARTESIAN_POINT('Ctrl Pts',(-2.30129622342295,0.682214955011516,
6.21755658167349));
#24748=CARTESIAN_POINT('Ctrl Pts',(-2.2956480566498,0.7,6.31153726264456));
#24749=CARTESIAN_POINT('Ctrl Pts',(-2.2956480566498,0.7,6.48846273735544));
#24750=CARTESIAN_POINT('Ctrl Pts',(-2.30129622342295,0.682214955011516,
6.58244341832651));
#24751=CARTESIAN_POINT('Ctrl Pts',(-2.31670997613269,0.627102242782997,
6.71508313975596));
#24752=CARTESIAN_POINT('Ctrl Pts',(-2.3232708588146,0.602709964998632,6.75942371209315));
#24753=CARTESIAN_POINT('Ctrl Pts',(-2.33023603954621,0.574456264653803,
6.8));
#24754=CARTESIAN_POINT('Origin',(0.,0.,5.8));
#24755=CARTESIAN_POINT('Origin',(3.6,-2.4,5.5));
#24756=CARTESIAN_POINT('',(3.35,-2.4,5.2));
#24757=CARTESIAN_POINT('',(3.35,-2.4,5.5));
#24758=CARTESIAN_POINT('Origin',(3.6,-2.4,5.2));
#24759=CARTESIAN_POINT('Origin',(-3.6,-2.4,5.5));
#24760=CARTESIAN_POINT('',(-3.85,-2.4,5.2));
#24761=CARTESIAN_POINT('',(-3.85,-2.4,5.5));
#24762=CARTESIAN_POINT('Origin',(-3.6,-2.4,5.2));
#24763=CARTESIAN_POINT('Origin',(-3.6,2.4,5.5));
#24764=CARTESIAN_POINT('',(-3.85,2.4,5.2));
#24765=CARTESIAN_POINT('',(-3.85,2.4,5.5));
#24766=CARTESIAN_POINT('Origin',(-3.6,2.4,5.2));
#24767=CARTESIAN_POINT('Origin',(3.6,2.4,5.5));
#24768=CARTESIAN_POINT('',(3.35,2.4,5.2));
#24769=CARTESIAN_POINT('',(3.35,2.4,5.5));
#24770=CARTESIAN_POINT('Origin',(3.6,2.4,5.2));
#24771=CARTESIAN_POINT('Origin',(0.,0.,5.5));
#24772=CARTESIAN_POINT('',(-0.6,7.34788079488412E-17,5.5));
#24773=CARTESIAN_POINT('',(-0.6,7.34788079488412E-17,5.2));
#24774=CARTESIAN_POINT('',(-0.6,7.34788079488412E-17,5.5));
#24775=CARTESIAN_POINT('Origin',(0.,0.,5.2));
#24776=CARTESIAN_POINT('Origin',(4.,2.8,5.2));
#24777=CARTESIAN_POINT('',(4.,2.8,5.2));
#24778=CARTESIAN_POINT('',(-4.,2.8,5.2));
#24779=CARTESIAN_POINT('',(4.,2.8,5.2));
#24780=CARTESIAN_POINT('',(-4.,2.8,5.2));
#24781=CARTESIAN_POINT('',(4.,2.8,5.2));
#24782=CARTESIAN_POINT('Origin',(4.,-2.8,5.2));
#24783=CARTESIAN_POINT('',(4.,-2.8,5.2));
#24784=CARTESIAN_POINT('',(4.,-2.8,5.2));
#24785=CARTESIAN_POINT('',(4.,-2.8,5.2));
#24786=CARTESIAN_POINT('Origin',(-4.,-2.8,5.2));
#24787=CARTESIAN_POINT('',(-4.,-2.8,5.2));
#24788=CARTESIAN_POINT('',(-4.,-2.8,5.2));
#24789=CARTESIAN_POINT('',(-4.,-2.8,5.2));
#24790=CARTESIAN_POINT('Origin',(-4.,2.8,5.2));
#24791=CARTESIAN_POINT('',(-4.,2.8,5.2));
#24792=CARTESIAN_POINT('Origin',(0.,0.,5.2));
#24793=CARTESIAN_POINT('',(0.,0.,0.));
#24794=CARTESIAN_POINT('Origin',(0.,0.,0.));
#24795=CARTESIAN_POINT('',(-0.8,-9.79717439317883E-17,0.));
#24796=CARTESIAN_POINT('Origin',(0.,0.,0.));
#24797=CARTESIAN_POINT('',(-0.6,-7.34788079488412E-17,0.));
#24798=CARTESIAN_POINT('Origin',(0.,0.,0.));
#24799=CARTESIAN_POINT('Origin',(0.,0.,-0.2));
#24800=CARTESIAN_POINT('',(-0.8,-9.79717439317883E-17,-0.2));
#24801=CARTESIAN_POINT('',(-0.8,-9.79717439317883E-17,-0.2));
#24802=CARTESIAN_POINT('Origin',(0.,0.,-0.2));
#24803=CARTESIAN_POINT('Origin',(0.,0.,-0.2));
#24804=CARTESIAN_POINT('',(-0.4,-4.89858719658941E-17,-0.2));
#24805=CARTESIAN_POINT('Origin',(0.,0.,-0.2));
#24806=CARTESIAN_POINT('Origin',(0.,0.,0.));
#24807=CARTESIAN_POINT('',(-0.4,-4.89858719658941E-17,0.8));
#24808=CARTESIAN_POINT('Origin',(0.,0.,0.8));
#24809=CARTESIAN_POINT('',(-0.4,-4.89858719658941E-17,0.));
#24810=CARTESIAN_POINT('Origin',(0.,0.,0.));
#24811=CARTESIAN_POINT('',(-0.6,-7.34788079488412E-17,0.8));
#24812=CARTESIAN_POINT('Origin',(0.,0.,0.8));
#24813=CARTESIAN_POINT('',(-0.6,-7.34788079488412E-17,0.));
#24814=CARTESIAN_POINT('Origin',(0.,0.,0.8));
#24815=CARTESIAN_POINT('',(0.,0.,0.));
#24816=CARTESIAN_POINT('Origin',(0.,0.,8.1));
#24817=CARTESIAN_POINT('',(-0.166755106676391,-0.000121435635125306,7.78714803633902));
#24818=CARTESIAN_POINT('',(-0.166799883948055,9.68813611086832E-5,7.76785196366098));
#24819=CARTESIAN_POINT('',(-0.1666,2.04026156737949E-17,8.1));
#24820=CARTESIAN_POINT('',(-0.163512932725147,-0.0319230454628249,7.7));
#24821=CARTESIAN_POINT('Ctrl Pts',(-0.166799883948055,9.68813611086832E-5,
7.76785196366098));
#24822=CARTESIAN_POINT('Ctrl Pts',(-0.166840645338411,0.00590548551433283,
7.76746222055426));
#24823=CARTESIAN_POINT('Ctrl Pts',(-0.166563633223871,0.0117101988552057,
7.76707247744754));
#24824=CARTESIAN_POINT('Ctrl Pts',(-0.165956013515963,0.0174801248594044,
7.76668273434082));
#24825=CARTESIAN_POINT('Ctrl Pts',(-0.16018045080637,0.0723245761391249,
7.76297813798855));
#24826=CARTESIAN_POINT('Ctrl Pts',(-0.124534715755048,0.124026015090588,
7.75927354163629));
#24827=CARTESIAN_POINT('Ctrl Pts',(-0.0753218907600186,0.148913777527237,
7.75556894528402));
#24828=CARTESIAN_POINT('Ctrl Pts',(-0.0261090657649881,0.173801539963886,
7.75186434893175));
#24829=CARTESIAN_POINT('Ctrl Pts',(0.0366708491737493,0.17187562588572,
7.74815975257948));
#24830=CARTESIAN_POINT('Ctrl Pts',(0.0842656460541181,0.144035707307694,
7.74445515622722));
#24831=CARTESIAN_POINT('Ctrl Pts',(0.131860442934486,0.116195788729669,
7.74075055987495));
#24832=CARTESIAN_POINT('Ctrl Pts',(0.164270121756485,0.0624418656517862,
7.73704596352268));
#24833=CARTESIAN_POINT('Ctrl Pts',(0.166703321037463,0.0073384302242929,
7.73334136717041));
#24834=CARTESIAN_POINT('Ctrl Pts',(0.169136520318441,-0.0477650052032019,
7.72963677081815));
#24835=CARTESIAN_POINT('Ctrl Pts',(0.141593240058396,-0.104217952980307,
7.72593217446588));
#24836=CARTESIAN_POINT('Ctrl Pts',(0.0965948053937569,-0.136111577080138,
7.72222757811361));
#24837=CARTESIAN_POINT('Ctrl Pts',(0.0515963707291191,-0.168005201179968,
7.71852298176134));
#24838=CARTESIAN_POINT('Ctrl Pts',(-0.0108572183401114,-0.175339501602526,
7.71481838540907));
#24839=CARTESIAN_POINT('Ctrl Pts',(-0.0619807511793317,-0.154911947739832,
7.7111137890568));
#24840=CARTESIAN_POINT('Ctrl Pts',(-0.113104284018553,-0.134484393877138,
7.70740919270453));
#24841=CARTESIAN_POINT('Ctrl Pts',(-0.152897760627764,-0.0862949857291892,
7.70370459635227));
#24842=CARTESIAN_POINT('Ctrl Pts',(-0.163512932725147,-0.0319230454628249,
7.7));
#24843=CARTESIAN_POINT('',(-0.00525765170773282,0.166819768394696,7.7));
#24844=CARTESIAN_POINT('Origin',(0.,0.,7.7));
#24845=CARTESIAN_POINT('',(-0.166344373414692,-6.51389168225824E-5,7.71714803633902));
#24846=CARTESIAN_POINT('Ctrl Pts',(-0.00525764907570514,0.166819936918742,
7.7));
#24847=CARTESIAN_POINT('Ctrl Pts',(-0.0593082520320288,0.165047155780287,
7.70363229181855));
#24848=CARTESIAN_POINT('Ctrl Pts',(-0.11251659993028,0.134577229369471,
7.70726458363711));
#24849=CARTESIAN_POINT('Ctrl Pts',(-0.141284856726116,0.0887831345736904,
7.71089687545566));
#24850=CARTESIAN_POINT('Ctrl Pts',(-0.157788211499337,0.0625126449052761,
7.71298059575011));
#24851=CARTESIAN_POINT('Ctrl Pts',(-0.166248526827595,0.0311990933978105,
7.71506431604457));
#24852=CARTESIAN_POINT('Ctrl Pts',(-0.166344373414692,-6.51389168225825E-5,
7.71714803633902));
#24853=CARTESIAN_POINT('',(-0.1666,-2.04026156737949E-17,7.6));
#24854=CARTESIAN_POINT('',(-0.1666,2.04026156737949E-17,8.1));
#24855=CARTESIAN_POINT('Origin',(0.,0.,7.6));
#24856=CARTESIAN_POINT('Ctrl Pts',(-0.166344373414692,-6.51389168225825E-5,
7.71714803633902));
#24857=CARTESIAN_POINT('Ctrl Pts',(-0.166418930176779,-0.0243848356437411,
7.71876891239684));
#24858=CARTESIAN_POINT('Ctrl Pts',(-0.161432221274225,-0.0486746897655862,
7.72038978845465));
#24859=CARTESIAN_POINT('Ctrl Pts',(-0.151232954480441,-0.0705377895071834,
7.72201066451247));
#24860=CARTESIAN_POINT('Ctrl Pts',(-0.127922000889724,-0.120507038643429,
7.72571526086474));
#24861=CARTESIAN_POINT('Ctrl Pts',(-0.0773819611304395,-0.157799535692006,
7.72941985721701));
#24862=CARTESIAN_POINT('Ctrl Pts',(-0.0227493309511543,-0.165321415232451,
7.73312445356928));
#24863=CARTESIAN_POINT('Ctrl Pts',(0.0318832992281324,-0.172843294772896,
7.73682904992154));
#24864=CARTESIAN_POINT('Ctrl Pts',(0.0906085198274197,-0.150594556805206,
7.74053364627381));
#24865=CARTESIAN_POINT('Ctrl Pts',(0.126553702502437,-0.10877093791917,
7.74423824262608));
#24866=CARTESIAN_POINT('Ctrl Pts',(0.162498885177452,-0.0669473190331356,
7.74794283897834));
#24867=CARTESIAN_POINT('Ctrl Pts',(0.175664029928199,-0.00554881922875591,
7.75164743533061));
#24868=CARTESIAN_POINT('Ctrl Pts',(0.160022369379138,0.0473319831645365,
7.75535203168288));
#24869=CARTESIAN_POINT('Ctrl Pts',(0.144380708830077,0.10021278555783,7.75905662803515));
#24870=CARTESIAN_POINT('Ctrl Pts',(0.0999322429812069,0.144575890540035,
7.76276122438742));
#24871=CARTESIAN_POINT('Ctrl Pts',(0.0470199032740834,0.160114846699796,
7.76646582073968));
#24872=CARTESIAN_POINT('Ctrl Pts',(-0.00589243643303862,0.175653802859556,
7.77017041709195));
#24873=CARTESIAN_POINT('Ctrl Pts',(-0.0672686499984137,0.162368610196872,
7.77387501344422));
#24874=CARTESIAN_POINT('Ctrl Pts',(-0.109019988249582,0.126341039149064,
7.77757960979649));
#24875=CARTESIAN_POINT('Ctrl Pts',(-0.144965839935877,0.0953230699114976,
7.78076908531066));
#24876=CARTESIAN_POINT('Ctrl Pts',(-0.166365019120212,0.0474476213275738,
7.78395856082484));
#24877=CARTESIAN_POINT('Ctrl Pts',(-0.166755106676391,-0.000121435635125306,
7.78714803633902));
#24878=CARTESIAN_POINT('Origin',(0.,0.,8.1));
#24879=CARTESIAN_POINT('',(-0.166723919921104,0.000132477254470589,7.85714803633902));
#24880=CARTESIAN_POINT('',(-0.16637029761803,8.32303651922684E-5,7.83785196366098));
#24881=CARTESIAN_POINT('',(-0.1666,2.04026156737949E-17,8.1));
#24882=CARTESIAN_POINT('Ctrl Pts',(-0.16637029761803,8.32303651922683E-5,
7.83785196366098));
#24883=CARTESIAN_POINT('Ctrl Pts',(-0.166471779784318,0.0225194758640918,
7.83635646533454));
#24884=CARTESIAN_POINT('Ctrl Pts',(-0.162250862274583,0.0449191273246156,
7.83486096700809));
#24885=CARTESIAN_POINT('Ctrl Pts',(-0.153526177634359,0.0654002352708428,
7.83336546868165));
#24886=CARTESIAN_POINT('Ctrl Pts',(-0.131913692804807,0.116135322329401,
7.82966087232938));
#24887=CARTESIAN_POINT('Ctrl Pts',(-0.0826645290024911,0.155097560201121,
7.82595627597712));
#24888=CARTESIAN_POINT('Ctrl Pts',(-0.0283176745893541,0.164455508498786,
7.82225167962485));
#24889=CARTESIAN_POINT('Ctrl Pts',(0.0260291798237814,0.173813456796451,
7.81854708327258));
#24890=CARTESIAN_POINT('Ctrl Pts',(0.085473724847738,0.153567115520063,
7.81484248692031));
#24891=CARTESIAN_POINT('Ctrl Pts',(0.12281048880676,0.112982637616973,7.81113789056804));
#24892=CARTESIAN_POINT('Ctrl Pts',(0.160147252765783,0.0723981597138804,
7.80743329421577));
#24893=CARTESIAN_POINT('Ctrl Pts',(0.175376235659869,0.0114755451840856,
7.8037286978635));
#24894=CARTESIAN_POINT('Ctrl Pts',(0.161528478593592,-0.0419042210738496,
7.80002410151124));
#24895=CARTESIAN_POINT('Ctrl Pts',(0.147680721527315,-0.0952839873317826,
7.79631950515897));
#24896=CARTESIAN_POINT('Ctrl Pts',(0.104756224500674,-0.141120905317855,
7.7926149088067));
#24897=CARTESIAN_POINT('Ctrl Pts',(0.0523982952481369,-0.158436269366283,
7.78891031245443));
#24898=CARTESIAN_POINT('Ctrl Pts',(4.03659955982363E-5,-0.175751633414712,
7.78520571610217));
#24899=CARTESIAN_POINT('Ctrl Pts',(-0.0617509954828385,-0.164545443525494,
7.7815011197499));
#24900=CARTESIAN_POINT('Ctrl Pts',(-0.104693981038127,-0.129948616776896,
7.77779652339763));
#24901=CARTESIAN_POINT('Ctrl Pts',(-0.143119137655905,-0.098991558968666,
7.77448167015208));
#24902=CARTESIAN_POINT('Ctrl Pts',(-0.166453199106715,-0.0493066103172041,
7.77116681690653));
#24903=CARTESIAN_POINT('Ctrl Pts',(-0.166799883948055,9.68813611086832E-5,
7.76785196366098));
#24904=CARTESIAN_POINT('Ctrl Pts',(-0.166755106676391,-0.000121435635125306,
7.78714803633902));
#24905=CARTESIAN_POINT('Ctrl Pts',(-0.166818108329162,-0.00780414471406952,
7.78766315717711));
#24906=CARTESIAN_POINT('Ctrl Pts',(-0.166333101894556,-0.0154788617727347,
7.7881782780152));
#24907=CARTESIAN_POINT('Ctrl Pts',(-0.165272862574954,-0.0230732790724375,
7.78869339885329));
#24908=CARTESIAN_POINT('Ctrl Pts',(-0.157647935712195,-0.0776900768131957,
7.79239799520556));
#24909=CARTESIAN_POINT('Ctrl Pts',(-0.120271619049716,-0.128153722861778,
7.79610259155783));
#24910=CARTESIAN_POINT('Ctrl Pts',(-0.0702495033623604,-0.151368804567472,
7.7998071879101));
#24911=CARTESIAN_POINT('Ctrl Pts',(-0.0202273876750051,-0.174583886273165,
7.80351178426237));
#24912=CARTESIAN_POINT('Ctrl Pts',(0.0424405270372255,-0.17055040363597,
7.80721638061463));
#24913=CARTESIAN_POINT('Ctrl Pts',(0.0890739684606603,-0.1411145241273,
7.8109209769669));
#24914=CARTESIAN_POINT('Ctrl Pts',(0.135707409884095,-0.111678644618631,
7.81462557331917));
#24915=CARTESIAN_POINT('Ctrl Pts',(0.166306378018734,-0.0568403682384865,
7.81833016967144));
#24916=CARTESIAN_POINT('Ctrl Pts',(0.166867054261352,-0.00169663156977216,
7.82203476602371));
#24917=CARTESIAN_POINT('Ctrl Pts',(0.16742773050397,0.0534471050989422,
7.82573936237597));
#24918=CARTESIAN_POINT('Ctrl Pts',(0.137950114854567,0.108896302056227,
7.82944395872824));
#24919=CARTESIAN_POINT('Ctrl Pts',(0.0919248190425322,0.139274263653544,
7.83314855508051));
#24920=CARTESIAN_POINT('Ctrl Pts',(0.0458995232304963,0.169652225250862,
7.83685315143278));
#24921=CARTESIAN_POINT('Ctrl Pts',(-0.0166734527441725,0.174958951488212,
7.84055774778505));
#24922=CARTESIAN_POINT('Ctrl Pts',(-0.0671572385601096,0.152765817367363,
7.84426234413731));
#24923=CARTESIAN_POINT('Ctrl Pts',(-0.117641024376046,0.130572683246515,
7.84796694048958));
#24924=CARTESIAN_POINT('Ctrl Pts',(-0.156035620033251,0.0808796887674675,
7.85167153684185));
#24925=CARTESIAN_POINT('Ctrl Pts',(-0.16476951761495,0.0264291003362266,
7.85537613319412));
#24926=CARTESIAN_POINT('Ctrl Pts',(-0.166161987861879,0.0177478874402586,
7.85596676757575));
#24927=CARTESIAN_POINT('Ctrl Pts',(-0.166800517689049,0.00894574204390801,
7.85655740195739));
#24928=CARTESIAN_POINT('Ctrl Pts',(-0.166723919921104,0.000132477254470589,
7.85714803633902));
#24929=CARTESIAN_POINT('Origin',(0.,0.,8.1));
#24930=CARTESIAN_POINT('',(-0.166337147585101,3.80246141342272E-5,7.92714803633902));
#24931=CARTESIAN_POINT('',(-0.166497798286919,-0.000143128711388071,7.90785196366098));
#24932=CARTESIAN_POINT('',(-0.1666,2.04026156737949E-17,8.1));
#24933=CARTESIAN_POINT('Ctrl Pts',(-0.166497798286919,-0.000143128711388071,
7.90785196366098));
#24934=CARTESIAN_POINT('Ctrl Pts',(-0.166178683426007,0.0388071044866986,
7.90525071011481));
#24935=CARTESIAN_POINT('Ctrl Pts',(-0.1525429547553,0.077958624681208,7.90264945656864));
#24936=CARTESIAN_POINT('Ctrl Pts',(-0.127583662987733,0.107563455699431,
7.90004820302248));
#24937=CARTESIAN_POINT('Ctrl Pts',(-0.0920376850212504,0.149725416097789,
7.89634360667021));
#24938=CARTESIAN_POINT('Ctrl Pts',(-0.0335249580924989,0.172524530026611,
7.89263901031793));
#24939=CARTESIAN_POINT('Ctrl Pts',(0.0211758393351308,0.165526651230438,
7.88893441396567));
#24940=CARTESIAN_POINT('Ctrl Pts',(0.075876636762759,0.158528772434265,
7.8852298176134));
#24941=CARTESIAN_POINT('Ctrl Pts',(0.126765504689265,0.121733900913099,
7.88152522126114));
#24942=CARTESIAN_POINT('Ctrl Pts',(0.150552858584944,0.0719814231904523,
7.87782062490887));
#24943=CARTESIAN_POINT('Ctrl Pts',(0.174340212480624,0.0222289454678044,
7.8741160285566));
#24944=CARTESIAN_POINT('Ctrl Pts',(0.171026052345475,-0.0404811384563263,
7.87041143220433));
#24945=CARTESIAN_POINT('Ctrl Pts',(0.142127133392108,-0.087449212862691,
7.86670683585206));
#24946=CARTESIAN_POINT('Ctrl Pts',(0.113228214438741,-0.134417287269055,
7.86300223949979));
#24947=CARTESIAN_POINT('Ctrl Pts',(0.0587445366671569,-0.165643352157655,
7.85929764314753));
#24948=CARTESIAN_POINT('Ctrl Pts',(0.00361084226918911,-0.166836602473997,
7.85559304679526));
#24949=CARTESIAN_POINT('Ctrl Pts',(-0.051522852128781,-0.168029852790339,
7.85188845044299));
#24950=CARTESIAN_POINT('Ctrl Pts',(-0.107306563153134,-0.139190288534421,
7.84818385409072));
#24951=CARTESIAN_POINT('Ctrl Pts',(-0.138210515736916,-0.0935165382837624,
7.84447925773845));
#24952=CARTESIAN_POINT('Ctrl Pts',(-0.156638936582612,-0.0662806988247655,
7.84227015971263));
#24953=CARTESIAN_POINT('Ctrl Pts',(-0.166220391697549,-0.0330588098244754,
7.8400610616868));
#24954=CARTESIAN_POINT('Ctrl Pts',(-0.16637029761803,8.32303651922683E-5,
7.83785196366098));
#24955=CARTESIAN_POINT('Ctrl Pts',(-0.166723919921104,0.000132477254470589,
7.85714803633902));
#24956=CARTESIAN_POINT('Ctrl Pts',(-0.166320078655114,-0.0463331066073077,
7.86026199830966));
#24957=CARTESIAN_POINT('Ctrl Pts',(-0.146038236890536,-0.0931077699995557,
7.86337596028029));
#24958=CARTESIAN_POINT('Ctrl Pts',(-0.111566386808172,-0.124098479205671,
7.86648992225092));
#24959=CARTESIAN_POINT('Ctrl Pts',(-0.0705561589135018,-0.160967287932896,
7.87019451860319));
#24960=CARTESIAN_POINT('Ctrl Pts',(-0.00946250361796861,-0.17549672300391,
7.87389911495546));
#24961=CARTESIAN_POINT('Ctrl Pts',(0.043754722198001,-0.161037309704663,
7.87760371130772));
#24962=CARTESIAN_POINT('Ctrl Pts',(0.0969719480139703,-0.146577896405417,
7.88130830765999));
#24963=CARTESIAN_POINT('Ctrl Pts',(0.142312744350376,-0.10312963473591,
7.88501290401226));
#24964=CARTESIAN_POINT('Ctrl Pts',(0.159026638215273,-0.0505768661856178,
7.88871750036453));
#24965=CARTESIAN_POINT('Ctrl Pts',(0.17574053208017,0.00197590236467367,
7.8924220967168));
#24966=CARTESIAN_POINT('Ctrl Pts',(0.16382752347356,0.0636331777957509,
7.89612669306907));
#24967=CARTESIAN_POINT('Ctrl Pts',(0.128739668561873,0.106177157462437,
7.89983128942133));
#24968=CARTESIAN_POINT('Ctrl Pts',(0.0936518136501853,0.148721137129124,
7.9035358857736));
#24969=CARTESIAN_POINT('Ctrl Pts',(0.0353891124334194,0.17215182103142,
7.90724048212587));
#24970=CARTESIAN_POINT('Ctrl Pts',(-0.0193841796186578,0.165746024286076,
7.91094507847814));
#24971=CARTESIAN_POINT('Ctrl Pts',(-0.0741574716707353,0.159340227540732,
7.91464967483041));
#24972=CARTESIAN_POINT('Ctrl Pts',(-0.125441354558124,0.123097950147749,
7.91835427118268));
#24973=CARTESIAN_POINT('Ctrl Pts',(-0.149765468420507,0.0736056756289514,
7.92205886753494));
#24974=CARTESIAN_POINT('Ctrl Pts',(-0.160903840835397,0.0509424292566785,
7.9237552571363));
#24975=CARTESIAN_POINT('Ctrl Pts',(-0.166389127400799,0.0255008441238536,
7.92545164673766));
#24976=CARTESIAN_POINT('Ctrl Pts',(-0.166337147585101,3.80246141342272E-5,
7.92714803633902));
#24977=CARTESIAN_POINT('Origin',(0.,0.,8.1));
#24978=CARTESIAN_POINT('',(-0.166584472654422,-0.000152342595601075,7.99714803633902));
#24979=CARTESIAN_POINT('',(-0.166875664957045,6.71117862603047E-7,7.97785196366098));
#24980=CARTESIAN_POINT('',(-0.1666,2.04026156737949E-17,8.1));
#24981=CARTESIAN_POINT('Ctrl Pts',(-0.166875663578624,6.71114506779717E-7,
7.97785196366098));
#24982=CARTESIAN_POINT('Ctrl Pts',(-0.166878959491358,0.055183185010619,
7.97414495489508));
#24983=CARTESIAN_POINT('Ctrl Pts',(-0.136794342365432,0.110362609757235,
7.97043794612919));
#24984=CARTESIAN_POINT('Ctrl Pts',(-0.0904129758162234,0.140260407963621,
7.9667309373633));
#24985=CARTESIAN_POINT('Ctrl Pts',(-0.0440617929130959,0.170138749551395,
7.96302634101103));
#24986=CARTESIAN_POINT('Ctrl Pts',(0.0185649237682023,0.174768358996025,
7.95932174465876));
#24987=CARTESIAN_POINT('Ctrl Pts',(0.0688057022669373,0.152030469242651,
7.95561714830649));
#24988=CARTESIAN_POINT('Ctrl Pts',(0.119046480765674,0.129292579489277,
7.95191255195423));
#24989=CARTESIAN_POINT('Ctrl Pts',(0.156901321081846,0.0791871905378969,
7.94820795560196));
#24990=CARTESIAN_POINT('Ctrl Pts',(0.165045740801789,0.0246453178400153,
7.94450335924969));
#24991=CARTESIAN_POINT('Ctrl Pts',(0.173190160521732,-0.0298965548578656,
7.94079876289742));
#24992=CARTESIAN_POINT('Ctrl Pts',(0.151624159645446,-0.088874911302248,
7.93709416654516));
#24993=CARTESIAN_POINT('Ctrl Pts',(0.110217540942827,-0.125297972397028,
7.93338957019289));
#24994=CARTESIAN_POINT('Ctrl Pts',(0.0688109222402075,-0.161721033491808,
7.92968497384062));
#24995=CARTESIAN_POINT('Ctrl Pts',(0.00756368571125483,-0.175588799236986,
7.92598037748835));
#24996=CARTESIAN_POINT('Ctrl Pts',(-0.0454940239107126,-0.160554607684999,
7.92227578113608));
#24997=CARTESIAN_POINT('Ctrl Pts',(-0.0985517335326801,-0.145520416133013,
7.91857118478381));
#24998=CARTESIAN_POINT('Ctrl Pts',(-0.143419916247662,-0.101584267283862,
7.91486658843155));
#24999=CARTESIAN_POINT('Ctrl Pts',(-0.159564393103046,-0.0488537894253407,
7.91116199207928));
#25000=CARTESIAN_POINT('Ctrl Pts',(-0.164372715171855,-0.0331490302896252,
7.91005864927318));
#25001=CARTESIAN_POINT('Ctrl Pts',(-0.166633153445445,-0.0166641862831651,
7.90895530646708));
#25002=CARTESIAN_POINT('Ctrl Pts',(-0.166497798286919,-0.000143128711388071,
7.90785196366098));
#25003=CARTESIAN_POINT('Ctrl Pts',(-0.166337147585101,3.80246141342272E-5,
7.92714803633902));
#25004=CARTESIAN_POINT('Ctrl Pts',(-0.166275613243749,-0.0301051724413385,
7.92915624308993));
#25005=CARTESIAN_POINT('Ctrl Pts',(-0.158454090740355,-0.0602781275943973,
7.93116444984084));
#25006=CARTESIAN_POINT('Ctrl Pts',(-0.143064725491982,-0.085906782795492,
7.93317265659175));
#25007=CARTESIAN_POINT('Ctrl Pts',(-0.114675523863702,-0.133184695056525,
7.93687725294402));
#25008=CARTESIAN_POINT('Ctrl Pts',(-0.0605327757697651,-0.164998247933979,
7.94058184929628));
#25009=CARTESIAN_POINT('Ctrl Pts',(-0.00541521687100755,-0.166787788618045,
7.94428644564855));
#25010=CARTESIAN_POINT('Ctrl Pts',(0.04970234202775,-0.168577329302111,
7.94799104200082));
#25011=CARTESIAN_POINT('Ctrl Pts',(0.105794711731329,-0.140342857792789,
7.95169563835309));
#25012=CARTESIAN_POINT('Ctrl Pts',(0.137190901172147,-0.0950060400465786,
7.95540023470536));
#25013=CARTESIAN_POINT('Ctrl Pts',(0.168587090612965,-0.0496692223003677,
7.95910483105762));
#25014=CARTESIAN_POINT('Ctrl Pts',(0.175287099791022,0.0127699416827313,
7.9628094274099));
#25015=CARTESIAN_POINT('Ctrl Pts',(0.154224631518061,0.0637358144365465,
7.96651402376216));
#25016=CARTESIAN_POINT('Ctrl Pts',(0.133162163245099,0.114701687190362,
7.97021862011443));
#25017=CARTESIAN_POINT('Ctrl Pts',(0.0843372175211171,0.154194268714893,
7.9739232164667));
#25018=CARTESIAN_POINT('Ctrl Pts',(0.0300948076110954,0.164139555144915,
7.97762781281897));
#25019=CARTESIAN_POINT('Ctrl Pts',(-0.0241476022989255,0.174084841574938,
7.98133240917123));
#25020=CARTESIAN_POINT('Ctrl Pts',(-0.0838074763949865,0.154482832910453,
7.9850370055235));
#25021=CARTESIAN_POINT('Ctrl Pts',(-0.121581135001586,0.114304499563856,
7.98874160187577));
#25022=CARTESIAN_POINT('Ctrl Pts',(-0.150153009444279,0.083913736846075,
7.99154374669685));
#25023=CARTESIAN_POINT('Ctrl Pts',(-0.16620298954139,0.041750515622899,
7.99434589151794));
#25024=CARTESIAN_POINT('Ctrl Pts',(-0.166584472654422,-0.000152342595601075,
7.99714803633902));
#25025=CARTESIAN_POINT('Origin',(0.,0.,8.1));
#25026=CARTESIAN_POINT('',(-0.166853498321983,5.50350387731602E-5,8.06714803633902));
#25027=CARTESIAN_POINT('',(-0.166495840369714,0.000142706802959736,8.04785196366098));
#25028=CARTESIAN_POINT('',(-0.1666,2.04026156737949E-17,8.1));
#25029=CARTESIAN_POINT('Ctrl Pts',(-0.166495840369714,0.000142706802959736,
8.04785196366098));
#25030=CARTESIAN_POINT('Ctrl Pts',(-0.166631270248863,0.0167365034787871,
8.04674379602763));
#25031=CARTESIAN_POINT('Ctrl Pts',(-0.164350623819369,0.0332939115131789,
8.04563562839428));
#25032=CARTESIAN_POINT('Ctrl Pts',(-0.159500786113399,0.0490610585913692,
8.04452746076093));
#25033=CARTESIAN_POINT('Ctrl Pts',(-0.143287813875328,0.101770516793988,
8.04082286440866));
#25034=CARTESIAN_POINT('Ctrl Pts',(-0.0983625864380453,0.145648334294652,
8.03711826805639));
#25035=CARTESIAN_POINT('Ctrl Pts',(-0.0452853888819718,0.160613579110374,
8.03341367170412));
#25036=CARTESIAN_POINT('Ctrl Pts',(0.00779180867410008,0.175578823926095,
8.02970907535185));
#25037=CARTESIAN_POINT('Ctrl Pts',(0.0690209763489626,0.161631496056876,
8.02600447899959));
#25038=CARTESIAN_POINT('Ctrl Pts',(0.110380238363978,0.12515466918812,8.02229988264732));
#25039=CARTESIAN_POINT('Ctrl Pts',(0.151739500378994,0.0886778423193637,
8.01859528629505));
#25040=CARTESIAN_POINT('Ctrl Pts',(0.173228856734163,0.0296715164510714,
8.01489068994278));
#25041=CARTESIAN_POINT('Ctrl Pts',(0.1650135816391,-0.0248597287931786,
8.01118609359052));
#25042=CARTESIAN_POINT('Ctrl Pts',(0.156798306544038,-0.0793909740374281,
8.00748149723825));
#25043=CARTESIAN_POINT('Ctrl Pts',(0.118878399998744,-0.129447138657635,
8.00377690088598));
#25044=CARTESIAN_POINT('Ctrl Pts',(0.0686081222571477,-0.152119735080243,
8.00007230453371));
#25045=CARTESIAN_POINT('Ctrl Pts',(0.0183378445155504,-0.174792331502851,
7.99636770818144));
#25046=CARTESIAN_POINT('Ctrl Pts',(-0.0442828044223508,-0.17008135972786,
7.99266311182918));
#25047=CARTESIAN_POINT('Ctrl Pts',(-0.0905951294928038,-0.140142822695884,
7.98895851547691));
#25048=CARTESIAN_POINT('Ctrl Pts',(-0.136877296221191,-0.110223781481477,
7.98525633153827));
#25049=CARTESIAN_POINT('Ctrl Pts',(-0.166872371955659,-0.0551100204273624,
7.98155414759962));
#25050=CARTESIAN_POINT('Ctrl Pts',(-0.166875663578624,6.71114506779717E-7,
7.97785196366098));
#25051=CARTESIAN_POINT('Ctrl Pts',(-0.166584472654422,-0.000152342595601075,
7.99714803633902));
#25052=CARTESIAN_POINT('Ctrl Pts',(-0.16670733212153,-0.013647468998692,
7.99805048787021));
#25053=CARTESIAN_POINT('Ctrl Pts',(-0.165205039699776,-0.0271155902953411,
7.99895293940139));
#25054=CARTESIAN_POINT('Ctrl Pts',(-0.161972485922986,-0.0401547607711461,
7.99985539093257));
#25055=CARTESIAN_POINT('Ctrl Pts',(-0.148702735120651,-0.0936810297308429,
8.00355998728484));
#25056=CARTESIAN_POINT('Ctrl Pts',(-0.106275790398842,-0.139978909621527,
8.00726458363711));
#25057=CARTESIAN_POINT('Ctrl Pts',(-0.0541085835863948,-0.157859913185374,
8.01096917998938));
#25058=CARTESIAN_POINT('Ctrl Pts',(-0.00194137677394735,-0.17574091674922,
8.01467377634165));
#25059=CARTESIAN_POINT('Ctrl Pts',(0.0599660921291386,-0.165205043986227,
8.01837837269392));
#25060=CARTESIAN_POINT('Ctrl Pts',(0.10328151894002,-0.131074096808347,
8.02208296904618));
#25061=CARTESIAN_POINT('Ctrl Pts',(0.146596945750902,-0.0969431496304671,
8.02578756539845));
#25062=CARTESIAN_POINT('Ctrl Pts',(0.171320330469579,-0.0392171280376997,
8.02949216175071));
#25063=CARTESIAN_POINT('Ctrl Pts',(0.166136875888483,0.0156853268589705,
8.03319675810298));
#25064=CARTESIAN_POINT('Ctrl Pts',(0.160953421307388,0.0705877817556402,
8.03690135445525));
#25065=CARTESIAN_POINT('Ctrl Pts',(0.125863127426521,0.122666669956213,
8.04060595080752));
#25066=CARTESIAN_POINT('Ctrl Pts',(0.0769252662159289,0.14808779296844,
8.04431054715979));
#25067=CARTESIAN_POINT('Ctrl Pts',(0.0279874050053375,0.173508915980668,
8.04801514351206));
#25068=CARTESIAN_POINT('Ctrl Pts',(-0.0347980235349782,0.172272273804551,
8.05171973986432));
#25069=CARTESIAN_POINT('Ctrl Pts',(-0.0826969120159334,0.144943822744164,
8.05542433621659));
#25070=CARTESIAN_POINT('Ctrl Pts',(-0.13059580049689,0.117615371683777,
8.05912893256886));
#25071=CARTESIAN_POINT('Ctrl Pts',(-0.163608148918485,0.0641951117391189,
8.06283352892113));
#25072=CARTESIAN_POINT('Ctrl Pts',(-0.166625668832836,0.0091311277873714,
8.0665381252734));
#25073=CARTESIAN_POINT('Ctrl Pts',(-0.166791266612054,0.00610928411571916,
8.06674142896194));
#25074=CARTESIAN_POINT('Ctrl Pts',(-0.166866529586575,0.00308249007446834,
8.06694473265048));
#25075=CARTESIAN_POINT('Ctrl Pts',(-0.166853498321983,5.50350387731602E-5,
8.06714803633902));
#25076=CARTESIAN_POINT('Origin',(0.,0.,8.1));
#25077=CARTESIAN_POINT('',(-0.166421992115154,0.00011764607293073,8.13714803633902));
#25078=CARTESIAN_POINT('',(-0.1663714196928,-8.42509827993143E-5,8.11785196366098));
#25079=CARTESIAN_POINT('',(-0.1666,2.04026156737949E-17,8.1));
#25080=CARTESIAN_POINT('Ctrl Pts',(-0.1663714196928,-8.42509827993143E-5,
8.11785196366098));
#25081=CARTESIAN_POINT('Ctrl Pts',(-0.166219315065703,0.033129634461824,
8.1156380408079));
#25082=CARTESIAN_POINT('Ctrl Pts',(-0.156593011917271,0.0664247241004012,
8.11342411795482));
#25083=CARTESIAN_POINT('Ctrl Pts',(-0.138088887731799,0.0936960368738783,
8.11121019510175));
#25084=CARTESIAN_POINT('Ctrl Pts',(-0.107125608743007,0.139329607927122,
8.10750559874948));
#25085=CARTESIAN_POINT('Ctrl Pts',(-0.0513045000135449,0.168096650686574,
8.10380100239722));
#25086=CARTESIAN_POINT('Ctrl Pts',(0.00382759151932898,0.166831764913151,
8.10009640604495));
#25087=CARTESIAN_POINT('Ctrl Pts',(0.0589596830522032,0.165566879139728,
8.09639180969269));
#25088=CARTESIAN_POINT('Ctrl Pts',(0.113402757388489,0.134270064833428,
8.09268721334042));
#25089=CARTESIAN_POINT('Ctrl Pts',(0.142240632844969,0.0872644865265266,
8.08898261698814));
#25090=CARTESIAN_POINT('Ctrl Pts',(0.17107850830145,0.0402589082196249,
8.08527802063588));
#25091=CARTESIAN_POINT('Ctrl Pts',(0.174311184878124,-0.0224554340878791,
8.08157342428361));
#25092=CARTESIAN_POINT('Ctrl Pts',(0.15045920980913,-0.0721769660244263,
8.07786882793134));
#25093=CARTESIAN_POINT('Ctrl Pts',(0.126607234740136,-0.121898497960974,
8.07416423157907));
#25094=CARTESIAN_POINT('Ctrl Pts',(0.0756706080254739,-0.158627219526564,
8.07045963522681));
#25095=CARTESIAN_POINT('Ctrl Pts',(0.0209607657114752,-0.165554023030732,
8.06675503887454));
#25096=CARTESIAN_POINT('Ctrl Pts',(-0.0337490766025232,-0.1724808265349,
8.06305044252227));
#25097=CARTESIAN_POINT('Ctrl Pts',(-0.0922321345158577,-0.149605711977646,
8.05934584617));
#25098=CARTESIAN_POINT('Ctrl Pts',(-0.127723304953095,-0.107397605246734,
8.05564124981773));
#25099=CARTESIAN_POINT('Ctrl Pts',(-0.152597889234011,-0.0778153430873971,
8.05304482109881));
#25100=CARTESIAN_POINT('Ctrl Pts',(-0.166178529146176,-0.0387364383267161,
8.0504483923799));
#25101=CARTESIAN_POINT('Ctrl Pts',(-0.166495840369714,0.000142706802959736,
8.04785196366098));
#25102=CARTESIAN_POINT('Ctrl Pts',(-0.166853498321983,5.50350387731602E-5,
8.06714803633902));
#25103=CARTESIAN_POINT('Ctrl Pts',(-0.166629074104989,-0.05208374405736,
8.07064932900275));
#25104=CARTESIAN_POINT('Ctrl Pts',(-0.14021687013706,-0.10441857192293,
8.07415062166647));
#25105=CARTESIAN_POINT('Ctrl Pts',(-0.0980400613034392,-0.135039391987217,
8.0776519143302));
#25106=CARTESIAN_POINT('Ctrl Pts',(-0.0534142424525818,-0.167438219851223,
8.08135651068247));
#25107=CARTESIAN_POINT('Ctrl Pts',(0.0088600866562422,-0.175528167620399,
8.08506110703474));
#25108=CARTESIAN_POINT('Ctrl Pts',(0.060282726186914,-0.15560682482505,
8.08876570338701));
#25109=CARTESIAN_POINT('Ctrl Pts',(0.111705365717586,-0.1356854820297,8.09247029973928));
#25110=CARTESIAN_POINT('Ctrl Pts',(0.152276315670106,-0.0877528486698254,
8.09617489609155));
#25111=CARTESIAN_POINT('Ctrl Pts',(0.163428050745771,-0.033745566199093,
8.09987949244381));
#25112=CARTESIAN_POINT('Ctrl Pts',(0.174579785821436,0.0202617162716397,
8.10358408879608));
#25113=CARTESIAN_POINT('Ctrl Pts',(0.156312306020247,0.0803436478532293,
8.10728868514834));
#25114=CARTESIAN_POINT('Ctrl Pts',(0.116985827056872,0.119003391869641,
8.11099328150061));
#25115=CARTESIAN_POINT('Ctrl Pts',(0.077659348093497,0.157663135886053,
8.11469787785288));
#25116=CARTESIAN_POINT('Ctrl Pts',(0.0172738699679364,0.174900692337286,
8.11840247420515));
#25117=CARTESIAN_POINT('Ctrl Pts',(-0.0365348508466968,0.162827195769839,
8.12210707055742));
#25118=CARTESIAN_POINT('Ctrl Pts',(-0.0903435716613295,0.150753699202392,
8.12581166690969));
#25119=CARTESIAN_POINT('Ctrl Pts',(-0.137575535165035,0.109369149616266,
8.12951626326196));
#25120=CARTESIAN_POINT('Ctrl Pts',(-0.156614765436894,0.0576134207959084,
8.13322085961422));
#25121=CARTESIAN_POINT('Ctrl Pts',(-0.163342481933899,0.0393249781631264,
8.13452991852249));
#25122=CARTESIAN_POINT('Ctrl Pts',(-0.166549946273643,0.0197415505506192,
8.13583897743075));
#25123=CARTESIAN_POINT('Ctrl Pts',(-0.166421992115154,0.00011764607293073,
8.13714803633902));
#25124=CARTESIAN_POINT('Origin',(0.,0.,8.1));
#25125=CARTESIAN_POINT('',(-0.166428342743546,-0.000120644360202635,8.20714803633902));
#25126=CARTESIAN_POINT('',(-0.166803308618304,-9.74733517731731E-5,8.18785196366097));
#25127=CARTESIAN_POINT('',(-0.1666,2.04026156737949E-17,8.1));
#25128=CARTESIAN_POINT('Ctrl Pts',(-0.166803308618304,-9.74733517731731E-5,
8.18785196366097));
#25129=CARTESIAN_POINT('Ctrl Pts',(-0.166459413794316,0.0493761805259084,
8.18453228558818));
#25130=CARTESIAN_POINT('Ctrl Pts',(-0.143046299360482,0.0991325150909699,
8.18121260751538));
#25131=CARTESIAN_POINT('Ctrl Pts',(-0.104524315745128,0.130085186162334,
8.17789292944259));
#25132=CARTESIAN_POINT('Ctrl Pts',(-0.0615356894825779,0.164626834427408,
8.17418833309032));
#25133=CARTESIAN_POINT('Ctrl Pts',(0.000268698766544943,0.175751425299081,
8.17048373673804));
#25134=CARTESIAN_POINT('Ctrl Pts',(0.0526037202653142,0.15836772668421,
8.16677914038577));
#25135=CARTESIAN_POINT('Ctrl Pts',(0.104938741764083,0.14098402806934,8.1630745440335));
#25136=CARTESIAN_POINT('Ctrl Pts',(0.147804396512497,0.0950920399679271,
8.15936994768124));
#25137=CARTESIAN_POINT('Ctrl Pts',(0.161582974550151,0.0416944909598549,
8.15566535132897));
#25138=CARTESIAN_POINT('Ctrl Pts',(0.175361552587805,-0.0117030580482178,
8.1519607549767));
#25139=CARTESIAN_POINT('Ctrl Pts',(0.160053053914698,-0.0726061679629504,
8.14825615862444));
#25140=CARTESIAN_POINT('Ctrl Pts',(0.12266349975367,-0.113142185187744,
8.14455156227217));
#25141=CARTESIAN_POINT('Ctrl Pts',(0.085273945592641,-0.153678202412537,
8.1408469659199));
#25142=CARTESIAN_POINT('Ctrl Pts',(0.0258033359436895,-0.173847126947391,
8.13714236956763));
#25143=CARTESIAN_POINT('Ctrl Pts',(-0.0285312674660481,-0.16441853611335,
8.13343777321536));
#25144=CARTESIAN_POINT('Ctrl Pts',(-0.0828658708757854,-0.154989945279309,
8.12973317686309));
#25145=CARTESIAN_POINT('Ctrl Pts',(-0.132064468046309,-0.115963839076372,
8.12602858051083));
#25146=CARTESIAN_POINT('Ctrl Pts',(-0.15361104200751,-0.0652007363013865,
8.12232398415856));
#25147=CARTESIAN_POINT('Ctrl Pts',(-0.162281057239455,-0.0447744320976445,
8.12083331065937));
#25148=CARTESIAN_POINT('Ctrl Pts',(-0.166473834434309,-0.0224477487753186,
8.11934263716017));
#25149=CARTESIAN_POINT('Ctrl Pts',(-0.1663714196928,-8.42509827993143E-5,
8.11785196366098));
#25150=CARTESIAN_POINT('Ctrl Pts',(-0.166421992115154,0.00011764607293073,
8.13714803633902));
#25151=CARTESIAN_POINT('Ctrl Pts',(-0.16618783994993,-0.0357934941187008,
8.13954357378302));
#25152=CARTESIAN_POINT('Ctrl Pts',(-0.154784081132574,-0.0718401827168746,
8.14193911122702));
#25153=CARTESIAN_POINT('Ctrl Pts',(-0.133343409090461,-0.100334571613147,
8.14433464867103));
#25154=CARTESIAN_POINT('Ctrl Pts',(-0.100186325432156,-0.144399927147257,
8.1480392450233));
#25155=CARTESIAN_POINT('Ctrl Pts',(-0.0430256610755357,-0.170403730160887,
8.15174384137557));
#25156=CARTESIAN_POINT('Ctrl Pts',(0.0119786818135821,-0.166445192753257,
8.15544843772784));
#25157=CARTESIAN_POINT('Ctrl Pts',(0.0669830247027004,-0.162486655345627,
8.1591530340801));
#25158=CARTESIAN_POINT('Ctrl Pts',(0.119831046124316,-0.128565777516737,
8.16285763043236));
#25159=CARTESIAN_POINT('Ctrl Pts',(0.146336549406162,-0.0802066413494387,
8.16656222678463));
#25160=CARTESIAN_POINT('Ctrl Pts',(0.172842052688009,-0.0318475051821409,
8.1702668231369));
#25161=CARTESIAN_POINT('Ctrl Pts',(0.173005037830088,0.0309498893235645,
8.17397141948917));
#25162=CARTESIAN_POINT('Ctrl Pts',(0.146750913757937,0.0794459584866981,
8.17767601584144));
#25163=CARTESIAN_POINT('Ctrl Pts',(0.120496789685787,0.127942027649832,
8.18138061219371));
#25164=CARTESIAN_POINT('Ctrl Pts',(0.0678255563994073,0.162136771470394,
8.18508520854597));
#25165=CARTESIAN_POINT('Ctrl Pts',(0.0128425024785167,0.166380771541514,
8.18878980489824));
#25166=CARTESIAN_POINT('Ctrl Pts',(-0.0421405514423743,0.170624771612635,
8.19249440125051));
#25167=CARTESIAN_POINT('Ctrl Pts',(-0.0994354259977765,0.144918027934313,
8.19619899760278));
#25168=CARTESIAN_POINT('Ctrl Pts',(-0.132820796963375,0.101025377518093,
8.19990359395505));
#25169=CARTESIAN_POINT('Ctrl Pts',(-0.154582807668421,0.0724142732947816,
8.20231840808304));
#25170=CARTESIAN_POINT('Ctrl Pts',(-0.166185696135255,0.0360759969505965,
8.20473322221103));
#25171=CARTESIAN_POINT('Ctrl Pts',(-0.166428342743546,-0.000120644360202635,
8.20714803633902));
#25172=CARTESIAN_POINT('Origin',(0.,0.,8.1));
#25173=CARTESIAN_POINT('',(-0.166857329749817,-5.00571843092702E-5,8.27714803633902));
#25174=CARTESIAN_POINT('',(-0.166666727468001,0.000145874381161297,8.25785196366098));
#25175=CARTESIAN_POINT('',(-0.1666,2.04026156737949E-17,8.1));
#25176=CARTESIAN_POINT('Ctrl Pts',(-0.166666727468001,0.000145874381161297,
8.25785196366098));
#25177=CARTESIAN_POINT('Ctrl Pts',(-0.166765391649288,0.0109115262509472,
8.25713112672072));
#25178=CARTESIAN_POINT('Ctrl Pts',(-0.165811590519144,0.021659769778576,
8.25641028978047));
#25179=CARTESIAN_POINT('Ctrl Pts',(-0.163741809565622,0.0321886321711107,
8.25568945284021));
#25180=CARTESIAN_POINT('Ctrl Pts',(-0.153104586995315,0.0862996010110572,
8.25198485648794));
#25181=CARTESIAN_POINT('Ctrl Pts',(-0.11299166880269,0.134616189497655,
8.24828026013567));
#25182=CARTESIAN_POINT('Ctrl Pts',(-0.0617609594542789,0.155026036936271,
8.2445756637834));
#25183=CARTESIAN_POINT('Ctrl Pts',(-0.0105302501058676,0.175435884374887,
8.24087106743114));
#25184=CARTESIAN_POINT('Ctrl Pts',(0.05181825039833,0.16793899076552,8.23716647107887));
#25185=CARTESIAN_POINT('Ctrl Pts',(0.0967503972625045,0.135966351978801,
8.2334618747266));
#25186=CARTESIAN_POINT('Ctrl Pts',(0.141682544126679,0.103993713192083,
8.22975727837434));
#25187=CARTESIAN_POINT('Ctrl Pts',(0.16919833735083,0.0475453292280127,
8.22605268202206));
#25188=CARTESIAN_POINT('Ctrl Pts',(0.166705018140776,-0.0075448769081583,
8.2223480856698));
#25189=CARTESIAN_POINT('Ctrl Pts',(0.164211698930722,-0.0626350830443292,
8.21864348931753));
#25190=CARTESIAN_POINT('Ctrl Pts',(0.131709267286462,-0.116367111352601,
8.21493889296526));
#25191=CARTESIAN_POINT('Ctrl Pts',(0.0840726453513101,-0.144150194396363,
8.21123429661299));
#25192=CARTESIAN_POINT('Ctrl Pts',(0.0364360234161577,-0.171933277440126,
8.20752970026072));
#25193=CARTESIAN_POINT('Ctrl Pts',(-0.0263347888098876,-0.173767415219379,
8.20382510390846));
#25194=CARTESIAN_POINT('Ctrl Pts',(-0.0755123731768594,-0.148813204179182,
8.20012050755619));
#25195=CARTESIAN_POINT('Ctrl Pts',(-0.124689957543831,-0.123858993138985,
8.19641591120392));
#25196=CARTESIAN_POINT('Ctrl Pts',(-0.160274314051729,-0.0721164332793377,
8.19271131485164));
#25197=CARTESIAN_POINT('Ctrl Pts',(-0.16598006016769,-0.0172658005202765,
8.18900671849938));
#25198=CARTESIAN_POINT('Ctrl Pts',(-0.166572903697511,-0.0115666610778814,
8.18862180021991));
#25199=CARTESIAN_POINT('Ctrl Pts',(-0.166843183389611,-0.00583396746716338,
8.18823688194044));
#25200=CARTESIAN_POINT('Ctrl Pts',(-0.166803308618304,-9.74733517731731E-5,
8.18785196366097));
#25201=CARTESIAN_POINT('Ctrl Pts',(-0.166428342743546,-0.000120644360202635,
8.20714803633902));
#25202=CARTESIAN_POINT('Ctrl Pts',(-0.166557943311361,-0.0194537201444082,
8.2084378185633));
#25203=CARTESIAN_POINT('Ctrl Pts',(-0.163446738612952,-0.0387463908414866,
8.20972760078757));
#25204=CARTESIAN_POINT('Ctrl Pts',(-0.156911714654403,-0.0567996902533336,
8.21101738301185));
#25205=CARTESIAN_POINT('Ctrl Pts',(-0.138141394004038,-0.108653550454424,
8.21472197936412));
#25206=CARTESIAN_POINT('Ctrl Pts',(-0.0911248853275137,-0.150282713702488,
8.21842657571639));
#25207=CARTESIAN_POINT('Ctrl Pts',(-0.0373795604223798,-0.162635357383603,
8.22213117206866));
#25208=CARTESIAN_POINT('Ctrl Pts',(0.0163657644827538,-0.174988001064719,
8.22583576842093));
#25209=CARTESIAN_POINT('Ctrl Pts',(0.0768399056164966,-0.158064125178888,
8.22954036477319));
#25210=CARTESIAN_POINT('Ctrl Pts',(0.116366529377292,-0.119609037490229,
8.23324496112546));
#25211=CARTESIAN_POINT('Ctrl Pts',(0.155893153138087,-0.0811539498015699,
8.23694955747773));
#25212=CARTESIAN_POINT('Ctrl Pts',(0.174472259525936,-0.0211676503100823,
8.24065415383));
#25213=CARTESIAN_POINT('Ctrl Pts',(0.163601015151732,0.0328967908766299,
8.24435875018226));
#25214=CARTESIAN_POINT('Ctrl Pts',(0.152729770777529,0.0869612320633426,
8.24806334653453));
#25215=CARTESIAN_POINT('Ctrl Pts',(0.112408175641274,0.13510381494528,8.2517679428868));
#25216=CARTESIAN_POINT('Ctrl Pts',(0.0610896363960827,0.155291813479256,
8.25547253923907));
#25217=CARTESIAN_POINT('Ctrl Pts',(0.00977109715089173,0.175479812013233,
8.25917713559134));
#25218=CARTESIAN_POINT('Ctrl Pts',(-0.0525443862032349,0.167713226199247,
8.2628817319436));
#25219=CARTESIAN_POINT('Ctrl Pts',(-0.0973377793564846,0.135546478075116,
8.26658632829587));
#25220=CARTESIAN_POINT('Ctrl Pts',(-0.139906046427994,0.104977623416454,
8.27010689764359));
#25221=CARTESIAN_POINT('Ctrl Pts',(-0.166649815966412,0.052372567376715,
8.2736274669913));
#25222=CARTESIAN_POINT('Ctrl Pts',(-0.166857329749817,-5.00571843092702E-5,
8.27714803633902));
#25223=CARTESIAN_POINT('Origin',(0.,0.,8.1));
#25224=CARTESIAN_POINT('',(-0.166575830380064,0.000152189730136115,8.34714803633902));
#25225=CARTESIAN_POINT('',(-0.166329361973163,6.33250651713839E-6,8.32785196366098));
#25226=CARTESIAN_POINT('',(-0.1666,2.04026156737949E-17,8.1));
#25227=CARTESIAN_POINT('Ctrl Pts',(-0.166329361973163,6.33250651713839E-6,
8.32785196366098));
#25228=CARTESIAN_POINT('Ctrl Pts',(-0.16633865860321,0.0274266906163063,
8.326025371501));
#25229=CARTESIAN_POINT('Ctrl Pts',(-0.159934576682436,0.0548429606931825,
8.32419877934102));
#25230=CARTESIAN_POINT('Ctrl Pts',(-0.147093270055154,0.0788102667487975,
8.32237218718103));
#25231=CARTESIAN_POINT('Ctrl Pts',(-0.121049219975437,0.127419472751415,
8.31866759082877));
#25232=CARTESIAN_POINT('Ctrl Pts',(-0.0685264320130064,0.161841786350919,
8.3149629944765));
#25233=CARTESIAN_POINT('Ctrl Pts',(-0.013562257900901,0.166323640537549,
8.31125839812423));
#25234=CARTESIAN_POINT('Ctrl Pts',(0.0414019162112044,0.170805494724179,
8.30755380177196));
#25235=CARTESIAN_POINT('Ctrl Pts',(0.0988074764729849,0.145346889497936,
8.30384920541969));
#25236=CARTESIAN_POINT('Ctrl Pts',(0.132382442717744,0.10159909990231,8.30014460906742));
#25237=CARTESIAN_POINT('Ctrl Pts',(0.165957408962504,0.0578513103066831,
8.29644001271515));
#25238=CARTESIAN_POINT('Ctrl Pts',(0.175701781190243,-0.00418566365832695,
8.29273541636288));
#25239=CARTESIAN_POINT('Ctrl Pts',(0.157155992197206,-0.0561202490848672,
8.28903082001062));
#25240=CARTESIAN_POINT('Ctrl Pts',(0.138610203204169,-0.108054834511407,
8.28532622365835));
#25241=CARTESIAN_POINT('Ctrl Pts',(0.0917742529903561,-0.149887031399478,
8.28162162730609));
#25242=CARTESIAN_POINT('Ctrl Pts',(0.0380828797487078,-0.162472097638159,
8.27791703095382));
#25243=CARTESIAN_POINT('Ctrl Pts',(-0.0156084934929406,-0.175057163876841,
8.27421243460156));
#25244=CARTESIAN_POINT('Ctrl Pts',(-0.0761552897624244,-0.158395099466134,
8.27050783824928));
#25245=CARTESIAN_POINT('Ctrl Pts',(-0.115847924423172,-0.120111392664133,
8.26680324189701));
#25246=CARTESIAN_POINT('Ctrl Pts',(-0.147817202853201,-0.0892768942100117,
8.263819482485));
#25247=CARTESIAN_POINT('Ctrl Pts',(-0.166258326950347,-0.0444163744423642,
8.26083572307299));
#25248=CARTESIAN_POINT('Ctrl Pts',(-0.166666727468001,0.000145874381161297,
8.25785196366098));
#25249=CARTESIAN_POINT('Ctrl Pts',(-0.166857329749817,-5.00571843092702E-5,
8.27714803633902));
#25250=CARTESIAN_POINT('Ctrl Pts',(-0.166868176898728,-0.00279028969102808,
8.27733206334357));
#25251=CARTESIAN_POINT('Ctrl Pts',(-0.166806517545971,-0.00553002372997369,
8.27751609034812));
#25252=CARTESIAN_POINT('Ctrl Pts',(-0.166670821778591,-0.00826608591227963,
8.27770011735268));
#25253=CARTESIAN_POINT('Ctrl Pts',(-0.163939168095075,-0.0633449913412659,
8.28140471370495));
#25254=CARTESIAN_POINT('Ctrl Pts',(-0.131204557775671,-0.116935891764961,
8.28510931005722));
#25255=CARTESIAN_POINT('Ctrl Pts',(-0.0834481708510229,-0.144512607721388,
8.28881390640949));
#25256=CARTESIAN_POINT('Ctrl Pts',(-0.0356917839263749,-0.172089323677816,
8.29251850276175));
#25257=CARTESIAN_POINT('Ctrl Pts',(0.0270863796035167,-0.173651855166976,
8.29622309911402));
#25258=CARTESIAN_POINT('Ctrl Pts',(0.0761555372230057,-0.148485100796662,
8.29992769546628));
#25259=CARTESIAN_POINT('Ctrl Pts',(0.125224694842494,-0.123318346426348,
8.30363229181855));
#25260=CARTESIAN_POINT('Ctrl Pts',(0.160584846551581,-0.0714223061965609,
8.30733688817082));
#25261=CARTESIAN_POINT('Ctrl Pts',(0.166053218414492,-0.016547497181162,
8.31104148452309));
#25262=CARTESIAN_POINT('Ctrl Pts',(0.171521590277403,0.0383273118342368,
8.31474608087536));
#25263=CARTESIAN_POINT('Ctrl Pts',(0.14709818229414,0.0961808896352466,
8.31845067722763));
#25264=CARTESIAN_POINT('Ctrl Pts',(0.103960505619201,0.130536218273543,
8.3221552735799));
#25265=CARTESIAN_POINT('Ctrl Pts',(0.0608228289442621,0.164891546911839,
8.32585986993216));
#25266=CARTESIAN_POINT('Ctrl Pts',(-0.00102911642235214,0.175748626387421,
8.32956446628443));
#25267=CARTESIAN_POINT('Ctrl Pts',(-0.0532884369608459,0.158138652745392,
8.3332690626367));
#25268=CARTESIAN_POINT('Ctrl Pts',(-0.105547757499339,0.140528679103364,
8.33697365898897));
#25269=CARTESIAN_POINT('Ctrl Pts',(-0.148214453209713,0.0944516523437251,
8.34067825534123));
#25270=CARTESIAN_POINT('Ctrl Pts',(-0.16176186886028,0.0409949849761845,
8.3443828516935));
#25271=CARTESIAN_POINT('Ctrl Pts',(-0.165132555990647,0.027694610544955,
8.34530457990867));
#25272=CARTESIAN_POINT('Ctrl Pts',(-0.166700621367384,0.0139374013064621,
8.34622630812385));
#25273=CARTESIAN_POINT('Ctrl Pts',(-0.166575830380064,0.000152189730136115,
8.34714803633902));
#25274=CARTESIAN_POINT('Origin',(0.,0.,8.1));
#25275=CARTESIAN_POINT('',(-0.166339236432839,-4.26122283673641E-5,8.41714803633902));
#25276=CARTESIAN_POINT('',(-0.166643482566988,-0.000149162233397024,8.39785196366098));
#25277=CARTESIAN_POINT('',(-0.1666,2.04026156737949E-17,8.1));
#25278=CARTESIAN_POINT('Ctrl Pts',(-0.166643482566988,-0.000149162233397024,
8.39785196366098));
#25279=CARTESIAN_POINT('Ctrl Pts',(-0.166239168982283,0.043660968966674,
8.39491961628127));
#25280=CARTESIAN_POINT('Ctrl Pts',(-0.148495522651441,0.0877608658755926,
8.39198726890156));
#25281=CARTESIAN_POINT('Ctrl Pts',(-0.117499615731863,0.118496111839818,
8.38905492152186));
#25282=CARTESIAN_POINT('Ctrl Pts',(-0.0783407751033059,0.157325645091268,
8.38535032516959));
#25283=CARTESIAN_POINT('Ctrl Pts',(-0.0180304466584345,0.17482430805586,
8.38164572881733));
#25284=CARTESIAN_POINT('Ctrl Pts',(0.0358300059551043,0.162983738211835,
8.37794113246506));
#25285=CARTESIAN_POINT('Ctrl Pts',(0.0896904585686423,0.151143168367811,
8.37423653611279));
#25286=CARTESIAN_POINT('Ctrl Pts',(0.137101035350848,0.109963365715171,
8.37053193976051));
#25287=CARTESIAN_POINT('Ctrl Pts',(0.15636401692648,0.0582905005399897,
8.36682734340825));
#25288=CARTESIAN_POINT('Ctrl Pts',(0.175626998502113,0.00661763536480815,
8.36312274705598));
#25289=CARTESIAN_POINT('Ctrl Pts',(0.166742384871172,-0.0555482923329149,
8.35941815070372));
#25290=CARTESIAN_POINT('Ctrl Pts',(0.133776269878663,-0.0997566932863041,
8.35571355435145));
#25291=CARTESIAN_POINT('Ctrl Pts',(0.100810154886153,-0.143965094239693,
8.35200895799918));
#25292=CARTESIAN_POINT('Ctrl Pts',(0.043762538532075,-0.170215968448749,
8.34830436164691));
#25293=CARTESIAN_POINT('Ctrl Pts',(-0.0112584140961097,-0.166495454454524,
8.34459976529464));
#25294=CARTESIAN_POINT('Ctrl Pts',(-0.0662793667242941,-0.162774940460298,
8.34089516894237));
#25295=CARTESIAN_POINT('Ctrl Pts',(-0.119273655626585,-0.129083038262791,
8.3371905725901));
#25296=CARTESIAN_POINT('Ctrl Pts',(-0.145988143979229,-0.080839037961172,
8.33348597623784));
#25297=CARTESIAN_POINT('Ctrl Pts',(-0.159530758707101,-0.0563822750094863,
8.33160797204555));
#25298=CARTESIAN_POINT('Ctrl Pts',(-0.166319803676251,-0.0281858105522191,
8.32972996785327));
#25299=CARTESIAN_POINT('Ctrl Pts',(-0.166329361973163,6.33250651713839E-6,
8.32785196366098));
#25300=CARTESIAN_POINT('Ctrl Pts',(-0.166575830380064,0.000152189730136115,
8.34714803633902));
#25301=CARTESIAN_POINT('Ctrl Pts',(-0.16619906328463,-0.0414679163135104,
8.34993090447612));
#25302=CARTESIAN_POINT('Ctrl Pts',(-0.150391099631022,-0.0833432770783291,
8.35271377261321));
#25303=CARTESIAN_POINT('Ctrl Pts',(-0.122172827684305,-0.113671857518162,
8.35549664075031));
#25304=CARTESIAN_POINT('Ctrl Pts',(-0.0846082352669996,-0.154045724669524,
8.35920123710257));
#25305=CARTESIAN_POINT('Ctrl Pts',(-0.0250509148416262,-0.173957150996807,
8.36290583345484));
#25306=CARTESIAN_POINT('Ctrl Pts',(0.0292423881988082,-0.164293559577237,
8.36661042980711));
#25307=CARTESIAN_POINT('Ctrl Pts',(0.0835356912392426,-0.154629968157667,
8.37031502615938));
#25308=CARTESIAN_POINT('Ctrl Pts',(0.132564976894738,-0.115391358991245,
8.37401962251165));
#25309=CARTESIAN_POINT('Ctrl Pts',(0.153891714545025,-0.064535503582266,
8.37772421886392));
#25310=CARTESIAN_POINT('Ctrl Pts',(0.175218452195312,-0.0136796481732867,
8.38142881521619));
#25311=CARTESIAN_POINT('Ctrl Pts',(0.168842641840389,0.0487934534782495,
8.38513341156845));
#25312=CARTESIAN_POINT('Ctrl Pts',(0.137682209292225,0.0942926312053136,
8.38883800792072));
#25313=CARTESIAN_POINT('Ctrl Pts',(0.106521776744061,0.139791808932377,
8.39254260427298));
#25314=CARTESIAN_POINT('Ctrl Pts',(0.0505767220026555,0.168317062734969,
8.39624720062525));
#25315=CARTESIAN_POINT('Ctrl Pts',(-0.0045493834981962,0.166813650344707,
8.39995179697752));
#25316=CARTESIAN_POINT('Ctrl Pts',(-0.0596754889990479,0.165310237954446,
8.40365639332979));
#25317=CARTESIAN_POINT('Ctrl Pts',(-0.113982645259346,0.133778159371331,
8.40736098968206));
#25318=CARTESIAN_POINT('Ctrl Pts',(-0.142616874078383,0.0866482454219461,
8.41106558603433));
#25319=CARTESIAN_POINT('Ctrl Pts',(-0.158288061727777,0.0608545797336438,
8.41309306946923));
#25320=CARTESIAN_POINT('Ctrl Pts',(-0.166269569984901,0.0303889749587513,
8.41512055290413));
#25321=CARTESIAN_POINT('Ctrl Pts',(-0.166339236432839,-4.26122283673641E-5,
8.41714803633902));
#25322=CARTESIAN_POINT('Origin',(0.,0.,8.1));
#25323=CARTESIAN_POINT('',(-0.166732044643443,-0.000130047968060085,8.48714803633902));
#25324=CARTESIAN_POINT('',(-0.16681984310415,8.64016909114964E-5,8.46785196366098));
#25325=CARTESIAN_POINT('',(-0.1666,2.04026156737949E-17,8.1));
#25326=CARTESIAN_POINT('Ctrl Pts',(-0.16681984310415,8.64016909114964E-5,
8.46785196366098));
#25327=CARTESIAN_POINT('Ctrl Pts',(-0.166851207378176,0.00505539796551705,
8.46751845741382));
#25328=CARTESIAN_POINT('Ctrl Pts',(-0.166648433574087,0.010021798785139,
8.46718495116665));
#25329=CARTESIAN_POINT('Ctrl Pts',(-0.166203182979447,0.0149663647710484,
8.46685144491949));
#25330=CARTESIAN_POINT('Ctrl Pts',(-0.161257327413684,0.0698907365654406,
8.46314684856722));
#25331=CARTESIAN_POINT('Ctrl Pts',(-0.126392682383394,0.122120946203704,
8.45944225221496));
#25332=CARTESIAN_POINT('Ctrl Pts',(-0.0775652682414317,0.147753565233456,
8.45573765586268));
#25333=CARTESIAN_POINT('Ctrl Pts',(-0.0287378540994696,0.173386184263208,
8.45203305951042));
#25334=CARTESIAN_POINT('Ctrl Pts',(0.0340523291541647,0.172421212684449,
8.44832846315814));
#25335=CARTESIAN_POINT('Ctrl Pts',(0.0820690071135884,0.145300263537307,
8.44462386680588));
#25336=CARTESIAN_POINT('Ctrl Pts',(0.130085685073012,0.118179314390165,
8.44091927045361));
#25337=CARTESIAN_POINT('Ctrl Pts',(0.163328857738225,0.0649023876746406,
8.43721467410134));
#25338=CARTESIAN_POINT('Ctrl Pts',(0.166584594097058,0.00985197688937799,
8.43351007774908));
#25339=CARTESIAN_POINT('Ctrl Pts',(0.16984033045589,-0.045198433895885,
8.42980548139681));
#25340=CARTESIAN_POINT('Ctrl Pts',(0.143108630508342,-0.102022328750885,
8.42610088504454));
#25341=CARTESIAN_POINT('Ctrl Pts',(0.0986234106037675,-0.134613932949943,
8.42239628869227));
#25342=CARTESIAN_POINT('Ctrl Pts',(0.0541381906991934,-0.167205537149,8.41869169234));
#25343=CARTESIAN_POINT('Ctrl Pts',(-0.0081005491624063,-0.175564850692113,
8.41498709598773));
#25344=CARTESIAN_POINT('Ctrl Pts',(-0.059608897920023,-0.155866184839173,
8.41128249963547));
#25345=CARTESIAN_POINT('Ctrl Pts',(-0.11111724667764,-0.136167518986233,
8.4075779032832));
#25346=CARTESIAN_POINT('Ctrl Pts',(-0.151895204331274,-0.0884108737372401,
8.40387330693093));
#25347=CARTESIAN_POINT('Ctrl Pts',(-0.163280506751969,-0.0344523493435898,
8.40016871057866));
#25348=CARTESIAN_POINT('Ctrl Pts',(-0.165653852525874,-0.0232043182326152,
8.3993964616061));
#25349=CARTESIAN_POINT('Ctrl Pts',(-0.16674996065773,-0.0116867887237509,
8.39862421263354));
#25350=CARTESIAN_POINT('Ctrl Pts',(-0.166643482566988,-0.000149162233397024,
8.39785196366098));
#25351=CARTESIAN_POINT('Ctrl Pts',(-0.166339236432839,-4.26122283673641E-5,
8.41714803633902));
#25352=CARTESIAN_POINT('Ctrl Pts',(-0.166396863783936,-0.0252153002460154,
8.41882514925639));
#25353=CARTESIAN_POINT('Ctrl Pts',(-0.161040873551955,-0.0503647119879558,
8.42050226217376));
#25354=CARTESIAN_POINT('Ctrl Pts',(-0.150145522232543,-0.0728272849498228,
8.42217937509113));
#25355=CARTESIAN_POINT('Ctrl Pts',(-0.126078640189889,-0.122445152056552,
8.4258839714434));
#25356=CARTESIAN_POINT('Ctrl Pts',(-0.0749835747268059,-0.158953136954354,
8.42958856779567));
#25357=CARTESIAN_POINT('Ctrl Pts',(-0.0202442715114259,-0.165643168038739,
8.43329316414793));
#25358=CARTESIAN_POINT('Ctrl Pts',(0.0344950317039542,-0.172333199123123,
8.4369977605002));
#25359=CARTESIAN_POINT('Ctrl Pts',(0.0928785726716311,-0.149205276394089,
8.44070235685247));
#25360=CARTESIAN_POINT('Ctrl Pts',(0.128186791283717,-0.106843995678858,
8.44440695320474));
#25361=CARTESIAN_POINT('Ctrl Pts',(0.163495009895803,-0.0644827149636277,
8.44811154955701));
#25362=CARTESIAN_POINT('Ctrl Pts',(0.175727906152299,-0.00288807626219958,
8.45181614590928));
#25363=CARTESIAN_POINT('Ctrl Pts',(0.159287028744638,0.0497507269318684,
8.45552074226155));
#25364=CARTESIAN_POINT('Ctrl Pts',(0.142846151336978,0.102389530125936,
8.45922533861382));
#25365=CARTESIAN_POINT('Ctrl Pts',(0.0977315002651613,0.146072497812644,
8.46292993496608));
#25366=CARTESIAN_POINT('Ctrl Pts',(0.0445900454027681,0.160807986828964,
8.46663453131835));
#25367=CARTESIAN_POINT('Ctrl Pts',(-0.00855140945962513,0.175543475845283,
8.47033912767062));
#25368=CARTESIAN_POINT('Ctrl Pts',(-0.0697196681125948,0.161331486191215,
8.47404372402289));
#25369=CARTESIAN_POINT('Ctrl Pts',(-0.110920718221372,0.124675988017335,
8.47774832037516));
#25370=CARTESIAN_POINT('Ctrl Pts',(-0.145767354814535,0.0936738455808142,
8.48088155902978));
#25371=CARTESIAN_POINT('Ctrl Pts',(-0.166330890122557,0.0466172354067069,
8.4840147976844));
#25372=CARTESIAN_POINT('Ctrl Pts',(-0.166732044643443,-0.000130047968060085,
8.48714803633902));
#25373=CARTESIAN_POINT('Origin',(0.,0.,8.1));
#25374=CARTESIAN_POINT('',(-0.166747144031447,0.000121296159821427,8.55714803633902));
#25375=CARTESIAN_POINT('',(-0.166383640089184,9.41837290711752E-5,8.53785196366098));
#25376=CARTESIAN_POINT('',(-0.1666,2.04026156737949E-17,8.1));
#25377=CARTESIAN_POINT('',(0.126907087985233,0.107935865304857,8.6));
#25378=CARTESIAN_POINT('Ctrl Pts',(-0.166747144031447,0.000121296159821427,
8.55714803633902));
#25379=CARTESIAN_POINT('Ctrl Pts',(-0.16635329561639,-0.0471552430000254,
8.56031823516921));
#25380=CARTESIAN_POINT('Ctrl Pts',(-0.14524398945692,-0.0947301254344308,
8.5634884339994));
#25381=CARTESIAN_POINT('Ctrl Pts',(-0.109675246818716,-0.12575848265665,
8.56665863282959));
#25382=CARTESIAN_POINT('Ctrl Pts',(-0.0681107137120021,-0.162017261723657,
8.57036322918185));
#25383=CARTESIAN_POINT('Ctrl Pts',(-0.00680104346501744,-0.175680871885562,
8.57406782553412));
#25384=CARTESIAN_POINT('Ctrl Pts',(0.0461904511917562,-0.160385037585203,
8.57777242188639));
#25385=CARTESIAN_POINT('Ctrl Pts',(0.0991819458485301,-0.145089203284843,
8.58147701823866));
#25386=CARTESIAN_POINT('Ctrl Pts',(0.143855264915093,-0.10083392452222,
8.58518161459093));
#25387=CARTESIAN_POINT('Ctrl Pts',(0.159759361228124,-0.0481275638750195,
8.5888862109432));
#25388=CARTESIAN_POINT('Ctrl Pts',(0.175663457541156,0.00457879677218119,
8.59259080729547));
#25389=CARTESIAN_POINT('Ctrl Pts',(0.162798331100656,0.0657362393039593,
8.59629540364773));
#25390=CARTESIAN_POINT('Ctrl Pts',(0.126907087985233,0.107935865304858,
8.6));
#25391=CARTESIAN_POINT('',(-0.127146846929917,0.108121031306322,8.59999999999999));
#25392=CARTESIAN_POINT('Origin',(0.,0.,8.6));
#25393=CARTESIAN_POINT('Ctrl Pts',(-0.127146980098748,0.108121134152685,
8.6));
#25394=CARTESIAN_POINT('Ctrl Pts',(-0.0920609617982474,0.149274297422621,
8.59636770818144));
#25395=CARTESIAN_POINT('Ctrl Pts',(-0.0350637580639813,0.171876538765403,
8.59273541636288));
#25396=CARTESIAN_POINT('Ctrl Pts',(0.0186762172371964,0.165816310153089,
8.58910312454433));
#25397=CARTESIAN_POINT('Ctrl Pts',(0.0734859424511011,0.159635446408496,
8.58539852819206));
#25398=CARTESIAN_POINT('Ctrl Pts',(0.124907471537698,0.123639642847462,
8.5816939318398));
#25399=CARTESIAN_POINT('Ctrl Pts',(0.149440861098049,0.0742590945192524,
8.57798933548753));
#25400=CARTESIAN_POINT('Ctrl Pts',(0.173974250658401,0.0248785461910427,
8.57428473913527));
#25401=CARTESIAN_POINT('Ctrl Pts',(0.171619500692506,-0.0378867469043425,
8.57058014278299));
#25402=CARTESIAN_POINT('Ctrl Pts',(0.143437456560707,-0.0852900722270229,
8.56687554643073));
#25403=CARTESIAN_POINT('Ctrl Pts',(0.115255412428908,-0.132693397549703,
8.56317095007846));
#25404=CARTESIAN_POINT('Ctrl Pts',(0.0612460741312054,-0.164734755099679,
8.55946635372619));
#25405=CARTESIAN_POINT('Ctrl Pts',(0.00613559996277483,-0.166761229307977,
8.55576175737392));
#25406=CARTESIAN_POINT('Ctrl Pts',(-0.0489748742056557,-0.168787703516275,
8.55205716102165));
#25407=CARTESIAN_POINT('Ctrl Pts',(-0.105186484244814,-0.140799294382895,
8.54835256466938));
#25408=CARTESIAN_POINT('Ctrl Pts',(-0.136777942839038,-0.0955995137046261,
8.54464796831711));
#25409=CARTESIAN_POINT('Ctrl Pts',(-0.1560958998925,-0.0679601624108457,
8.54238263343174));
#25410=CARTESIAN_POINT('Ctrl Pts',(-0.166207797888661,-0.033885070733673,
8.54011729854636));
#25411=CARTESIAN_POINT('Ctrl Pts',(-0.166383640089184,9.41837290711752E-5,
8.53785196366098));
#25412=CARTESIAN_POINT('Origin',(0.,0.,8.75459252805377));
#25413=CARTESIAN_POINT('',(-0.205721525535574,0.000119487981252803,7.74540747194623));
#25414=CARTESIAN_POINT('',(-0.205159724654165,-8.03386490614408E-5,7.73959252805377));
#25415=CARTESIAN_POINT('',(-0.205475,1.36055398187253E-14,8.75459252805377));
#25416=CARTESIAN_POINT('',(0.18826275096637,-0.0823232180103198,7.7));
#25417=CARTESIAN_POINT('Ctrl Pts',(-0.205159724654165,-8.03386490614358E-5,
7.73959252805377));
#25418=CARTESIAN_POINT('Ctrl Pts',(-0.205041512904561,0.0384791939730818,
7.73750880775931));
#25419=CARTESIAN_POINT('Ctrl Pts',(-0.176055839029368,0.14576176638949,
7.7317204911126));
#25420=CARTESIAN_POINT('Ctrl Pts',(-0.00298040876483471,0.242992688549725,
7.7222275781136));
#25421=CARTESIAN_POINT('Ctrl Pts',(0.202514421274951,0.133877006738626,
7.7111137890568));
#25422=CARTESIAN_POINT('Ctrl Pts',(0.215637179506012,-0.0197213743559677,
7.70370459635227));
#25423=CARTESIAN_POINT('Ctrl Pts',(0.188262750966369,-0.0823232180103224,
7.7));
#25424=CARTESIAN_POINT('',(0.122359307443305,-0.165534545134462,7.7));
#25425=CARTESIAN_POINT('Origin',(0.,0.,7.7));
#25426=CARTESIAN_POINT('Ctrl Pts',(-0.205721525535573,0.000119487981252853,
7.74540747194623));
#25427=CARTESIAN_POINT('Ctrl Pts',(-0.205771798324789,0.00728349121284206,
7.74501772883951));
#25428=CARTESIAN_POINT('Ctrl Pts',(-0.202182676839297,0.0824925534713558,
7.74092338938052));
#25429=CARTESIAN_POINT('Ctrl Pts',(-0.109630632113431,0.216732284629596,
7.73312445356927));
#25430=CARTESIAN_POINT('Ctrl Pts',(0.122656937311001,0.209606344739839,
7.72201066451247));
#25431=CARTESIAN_POINT('Ctrl Pts',(0.241793562216327,0.0120091699547426,
7.71096917998937));
#25432=CARTESIAN_POINT('Ctrl Pts',(0.175945028483479,-0.125819303453627,
7.70363229181856));
#25433=CARTESIAN_POINT('Ctrl Pts',(0.122359422806364,-0.165534717635809,
7.7));
#25434=CARTESIAN_POINT('Origin',(0.,0.,8.75459252805377));
#25435=CARTESIAN_POINT('',(-0.205191698097627,0.000102651616370908,7.81540747194623));
#25436=CARTESIAN_POINT('',(-0.205666299785903,-0.000149771831496819,7.80959252805377));
#25437=CARTESIAN_POINT('',(-0.205475,1.36055398187253E-14,8.75459252805377));
#25438=CARTESIAN_POINT('Ctrl Pts',(-0.205666299785903,-0.000149771831496818,
7.80959252805377));
#25439=CARTESIAN_POINT('Ctrl Pts',(-0.205185187897512,0.0585192076367542,
7.80640305253959));
#25440=CARTESIAN_POINT('Ctrl Pts',(-0.148137553353403,0.186149387791063,
7.79950898067314));
#25441=CARTESIAN_POINT('Ctrl Pts',(0.0684305468563471,0.233026651290108,
7.78891031245443));
#25442=CARTESIAN_POINT('Ctrl Pts',(0.232891204484732,0.0688818314302299,
7.77779652339763));
#25443=CARTESIAN_POINT('Ctrl Pts',(0.184179773794582,-0.158294460538047,
7.76668273434082));
#25444=CARTESIAN_POINT('Ctrl Pts',(-0.0331053048843776,-0.240615458747729,
7.75556894528403));
#25445=CARTESIAN_POINT('Ctrl Pts',(-0.18504446938345,-0.128502550435188,
7.74653887652167));
#25446=CARTESIAN_POINT('Ctrl Pts',(-0.205251678739939,-0.0300748745732145,
7.74121340411158));
#25447=CARTESIAN_POINT('Ctrl Pts',(-0.205159724654165,-8.03386490614358E-5,
7.73959252805377));
#25448=CARTESIAN_POINT('Ctrl Pts',(-0.205191698097627,0.000102651616370887,
7.81540747194623));
#25449=CARTESIAN_POINT('Ctrl Pts',(-0.205316860451277,0.0277742455172506,
7.81391197361979));
#25450=CARTESIAN_POINT('Ctrl Pts',(-0.187215293273578,0.12383601283077,
7.80871187894108));
#25451=CARTESIAN_POINT('Ctrl Pts',(-0.0412126180342513,0.239342358997698,
7.7998071879101));
#25452=CARTESIAN_POINT('Ctrl Pts',(0.178733982604362,0.164430288641772,
7.7886933988533));
#25453=CARTESIAN_POINT('Ctrl Pts',(0.23508167636479,-0.0609852135282689,
7.77757960979648));
#25454=CARTESIAN_POINT('Ctrl Pts',(0.0762597491160078,-0.230583185734543,
7.76646582073969));
#25455=CARTESIAN_POINT('Ctrl Pts',(-0.14435245202745,-0.190573997415322,
7.75574177478959));
#25456=CARTESIAN_POINT('Ctrl Pts',(-0.205293944096357,-0.060811979321282,
7.74872232519178));
#25457=CARTESIAN_POINT('Ctrl Pts',(-0.205721525535573,0.000119487981252853,
7.74540747194623));
#25458=CARTESIAN_POINT('Origin',(0.,0.,8.75459252805377));
#25459=CARTESIAN_POINT('',(-0.205348950198108,-0.000176526842551344,7.88540747194623));
#25460=CARTESIAN_POINT('',(-0.205627835809057,0.000163389939152625,7.87959252805377));
#25461=CARTESIAN_POINT('',(-0.205475,1.36055398187253E-14,8.75459252805377));
#25462=CARTESIAN_POINT('Ctrl Pts',(-0.205627835809057,0.000163389939152636,
7.87959252805377));
#25463=CARTESIAN_POINT('Ctrl Pts',(-0.205722307155807,0.0110331713473729,
7.87900189367214));
#25464=CARTESIAN_POINT('Ctrl Pts',(-0.199995231038606,0.0899810208205928,
7.87470666293823));
#25465=CARTESIAN_POINT('Ctrl Pts',(-0.0977380548679695,0.222329472572989,
7.86670683585206));
#25466=CARTESIAN_POINT('Ctrl Pts',(0.133783834178758,0.2026944262293,7.85559304679526));
#25467=CARTESIAN_POINT('Ctrl Pts',(0.242851896763891,-0.00246926665421919,
7.84447925773846));
#25468=CARTESIAN_POINT('Ctrl Pts',(0.129634796329349,-0.205372535067366,
7.83336546868165));
#25469=CARTESIAN_POINT('Ctrl Pts',(-0.102238368895662,-0.220296541877889,
7.82225167962484));
#25470=CARTESIAN_POINT('Ctrl Pts',(-0.200843893701057,-0.0871642606221136,
7.81432736608222));
#25471=CARTESIAN_POINT('Ctrl Pts',(-0.20574400245459,-0.00962518988669528,
7.81010764889186));
#25472=CARTESIAN_POINT('Ctrl Pts',(-0.205666299785903,-0.000149771831496818,
7.80959252805377));
#25473=CARTESIAN_POINT('Ctrl Pts',(-0.205348950198108,-0.00017652684255136,
7.88540747194623));
#25474=CARTESIAN_POINT('Ctrl Pts',(-0.204955372010552,0.047862483759944,
7.88280621840006));
#25475=CARTESIAN_POINT('Ctrl Pts',(-0.164187007775315,0.164918452985973,
7.87650036850162));
#25476=CARTESIAN_POINT('Ctrl Pts',(0.0308184982090563,0.240901114896414,
7.86648992225093));
#25477=CARTESIAN_POINT('Ctrl Pts',(0.21910883681408,0.104758985980235,7.85537613319412));
#25478=CARTESIAN_POINT('Ctrl Pts',(0.206846344849442,-0.12727020659438,
7.84426234413731));
#25479=CARTESIAN_POINT('Ctrl Pts',(0.00525510193017616,-0.242807583839013,
7.83314855508051));
#25480=CARTESIAN_POINT('Ctrl Pts',(-0.173372430949953,-0.150459116557522,
7.82353026435015));
#25481=CARTESIAN_POINT('Ctrl Pts',(-0.205006812629375,-0.0407728628372422,
7.81761656997206));
#25482=CARTESIAN_POINT('Ctrl Pts',(-0.205191698097627,0.000102651616370887,
7.81540747194623));
#25483=CARTESIAN_POINT('Origin',(0.,0.,8.75459252805377));
#25484=CARTESIAN_POINT('',(-0.205814989538108,8.27718761863166E-7,7.95540747194623));
#25485=CARTESIAN_POINT('',(-0.205150812725382,4.68974045001175E-5,7.94959252805377));
#25486=CARTESIAN_POINT('',(-0.205475,1.36055398187253E-14,8.75459252805377));
#25487=CARTESIAN_POINT('Ctrl Pts',(-0.205150812725382,4.6897404500125E-5,
7.94959252805377));
#25488=CARTESIAN_POINT('Ctrl Pts',(-0.205214921684749,0.0314512961965735,
7.94789613845241));
#25489=CARTESIAN_POINT('Ctrl Pts',(-0.183675662640219,0.131353623293904,
7.94249515249879));
#25490=CARTESIAN_POINT('Ctrl Pts',(-0.0282109883268786,0.241220379359275,
7.93338957019289));
#25491=CARTESIAN_POINT('Ctrl Pts',(0.187362754755622,0.154526145718984,
7.92227578113608));
#25492=CARTESIAN_POINT('Ctrl Pts',(0.23144124413335,-0.0736076238344533,
7.91116199207928));
#25493=CARTESIAN_POINT('Ctrl Pts',(0.0636789369204538,-0.234367495981061,
7.90004820302247));
#25494=CARTESIAN_POINT('Ctrl Pts',(-0.150356242673218,-0.183465152197969,
7.8895250483473));
#25495=CARTESIAN_POINT('Ctrl Pts',(-0.205129760874308,-0.057144628332151,
7.8827064900244));
#25496=CARTESIAN_POINT('Ctrl Pts',(-0.205627835809057,0.000163389939152636,
7.87959252805377));
#25497=CARTESIAN_POINT('Ctrl Pts',(-0.205814987838042,8.27714623007834E-7,
7.95540747194623));
#25498=CARTESIAN_POINT('Ctrl Pts',(-0.205814990483421,4.51185256548844E-5,
7.9554050595326));
#25499=CARTESIAN_POINT('Ctrl Pts',(-0.205794920564842,0.0681041019067216,
7.95169805076671));
#25500=CARTESIAN_POINT('Ctrl Pts',(-0.131583562478442,0.204129595218713,
7.94428644564855));
#25501=CARTESIAN_POINT('Ctrl Pts',(0.100137168795687,0.221259289107705,
7.93317265659175));
#25502=CARTESIAN_POINT('Ctrl Pts',(0.240201214065173,0.035867846224428,
7.92205886753494));
#25503=CARTESIAN_POINT('Ctrl Pts',(0.160406363583993,-0.182353842678505,
7.91094507847815));
#25504=CARTESIAN_POINT('Ctrl Pts',(-0.0662102497254891,-0.233664992135114,
7.89983128942133));
#25505=CARTESIAN_POINT('Ctrl Pts',(-0.19336732015938,-0.109149318984397,
7.8913187539107));
#25506=CARTESIAN_POINT('Ctrl Pts',(-0.205515889581051,-0.0205526631244362,
7.88651081475233));
#25507=CARTESIAN_POINT('Ctrl Pts',(-0.205348950198108,-0.00017652684255136,
7.88540747194623));
#25508=CARTESIAN_POINT('Origin',(0.,0.,8.75459252805377));
#25509=CARTESIAN_POINT('',(-0.205346535413967,0.000176006484619851,8.02540747194623));
#25510=CARTESIAN_POINT('',(-0.205455849451785,-0.000187890725276845,8.01959252805377));
#25511=CARTESIAN_POINT('',(-0.205475,1.36055398187253E-14,8.75459252805377));
#25512=CARTESIAN_POINT('Ctrl Pts',(-0.205455849451785,-0.000187890725276842,
8.01959252805376));
#25513=CARTESIAN_POINT('Ctrl Pts',(-0.204985349796021,0.0514927202738006,
8.01679038323268));
#25514=CARTESIAN_POINT('Ctrl Pts',(-0.159019907330079,0.172243718567035,
8.01028364205933));
#25515=CARTESIAN_POINT('Ctrl Pts',(0.043798823814624,0.238882386272181,
8.00007230453372));
#25516=CARTESIAN_POINT('Ctrl Pts',(0.224452588327861,0.0927586493798742,
7.98895851547691));
#25517=CARTESIAN_POINT('Ctrl Pts',(0.199662353288342,-0.138268131282085,
7.9778447264201));
#25518=CARTESIAN_POINT('Ctrl Pts',(-0.00788109805936929,-0.242736523239671,
7.96673093736331));
#25519=CARTESIAN_POINT('Ctrl Pts',(-0.17763289672451,-0.142992642240008,
7.95731353790785));
#25520=CARTESIAN_POINT('Ctrl Pts',(-0.205074919755458,-0.0371300138498422,
7.95160073480467));
#25521=CARTESIAN_POINT('Ctrl Pts',(-0.205150812725382,4.6897404500125E-5,
7.94959252805377));
#25522=CARTESIAN_POINT('Ctrl Pts',(-0.205346535413967,0.000176006484619816,
8.02540747194623));
#25523=CARTESIAN_POINT('Ctrl Pts',(-0.205513566953093,0.0206418550558431,
8.02429930431288));
#25524=CARTESIAN_POINT('Ctrl Pts',(-0.193297509774496,0.109329974644086,
8.01948654032727));
#25525=CARTESIAN_POINT('Ctrl Pts',(-0.0659066106883685,0.233750816567481,
8.01096917998937));
#25526=CARTESIAN_POINT('Ctrl Pts',(0.160643147318701,0.182145284864098,
7.99985539093258));
#25527=CARTESIAN_POINT('Ctrl Pts',(0.240154410771491,-0.0361798917467206,
7.98874160187577));
#25528=CARTESIAN_POINT('Ctrl Pts',(0.0998496185014871,-0.221389203127338,
7.97762781281897));
#25529=CARTESIAN_POINT('Ctrl Pts',(-0.131798368373502,-0.203962249775518,
7.96651643617579));
#25530=CARTESIAN_POINT('Ctrl Pts',(-0.205810928136795,-0.067969576514468,
7.95910965588487));
#25531=CARTESIAN_POINT('Ctrl Pts',(-0.205814987838042,8.27714623007834E-7,
7.95540747194623));
#25532=CARTESIAN_POINT('Origin',(0.,0.,8.75459252805377));
#25533=CARTESIAN_POINT('',(-0.205193082001069,-0.000103910388300932,8.09540747194623));
#25534=CARTESIAN_POINT('',(-0.205787650466444,6.7877098390864E-5,8.08959252805377));
#25535=CARTESIAN_POINT('',(-0.205475,1.36055398187253E-14,8.75459252805377));
#25536=CARTESIAN_POINT('Ctrl Pts',(-0.205787650466444,6.7877098390855E-5,
8.08959252805377));
#25537=CARTESIAN_POINT('Ctrl Pts',(-0.205803722489804,0.00380176859574709,
8.08938922436523));
#25538=CARTESIAN_POINT('Ctrl Pts',(-0.204019440224857,0.0755588970087965,
8.08548132432442));
#25539=CARTESIAN_POINT('Ctrl Pts',(-0.120353900451207,0.210945656715802,
8.07786882793134));
#25540=CARTESIAN_POINT('Ctrl Pts',(0.111954069464546,0.215521269881544,
8.06675503887454));
#25541=CARTESIAN_POINT('Ctrl Pts',(0.241789209953822,0.0228278205475825,
8.05564124981773));
#25542=CARTESIAN_POINT('Ctrl Pts',(0.150311944496376,-0.190760191819292,
8.04452746076093));
#25543=CARTESIAN_POINT('Ctrl Pts',(-0.0787475484122947,-0.229743237245029,
8.03341367170412));
#25544=CARTESIAN_POINT('Ctrl Pts',(-0.196148549788041,-0.101630843190257,
8.0251020274684));
#25545=CARTESIAN_POINT('Ctrl Pts',(-0.205607377356971,-0.0168320149610218,
8.02049497958495));
#25546=CARTESIAN_POINT('Ctrl Pts',(-0.205455849451785,-0.000187890725276842,
8.01959252805376));
#25547=CARTESIAN_POINT('Ctrl Pts',(-0.205193082001069,-0.000103910388300946,
8.09540747194623));
#25548=CARTESIAN_POINT('Ctrl Pts',(-0.205005484772661,0.0408602139318314,
8.09319354909315));
#25549=CARTESIAN_POINT('Ctrl Pts',(-0.17326642156507,0.150638073432689,
8.08727502988781));
#25550=CARTESIAN_POINT('Ctrl Pts',(0.00557052926712743,0.242800524674804,
8.0776519143302));
#25551=CARTESIAN_POINT('Ctrl Pts',(0.207011538257192,0.127001372461354,
8.06653812527341));
#25552=CARTESIAN_POINT('Ctrl Pts',(0.218972538609993,-0.105043576259552,
8.05542433621658));
#25553=CARTESIAN_POINT('Ctrl Pts',(0.0305054910554562,-0.240940948354804,
8.0443105471598));
#25554=CARTESIAN_POINT('Ctrl Pts',(-0.164307195981861,-0.164741743111656,
8.03430492573633));
#25555=CARTESIAN_POINT('Ctrl Pts',(-0.204955181730555,-0.0477753281223429,
8.02800390066515));
#25556=CARTESIAN_POINT('Ctrl Pts',(-0.205346535413967,0.000176006484619816,
8.02540747194623));
#25557=CARTESIAN_POINT('Origin',(0.,0.,8.75459252805377));
#25558=CARTESIAN_POINT('',(-0.205725749329808,-0.000120218108977228,8.16540747194623));
#25559=CARTESIAN_POINT('',(-0.205255455161232,0.000145098000214199,8.15959252805377));
#25560=CARTESIAN_POINT('',(-0.205475,1.36055398187253E-14,8.75459252805377));
#25561=CARTESIAN_POINT('Ctrl Pts',(-0.205255455161232,0.000145098000214217,
8.15959252805377));
#25562=CARTESIAN_POINT('Ctrl Pts',(-0.205413266570088,0.024348109840268,
8.1582834691455));
#25563=CARTESIAN_POINT('Ctrl Pts',(-0.190262273248928,0.116853699781198,
8.15326981388497));
#25564=CARTESIAN_POINT('Ctrl Pts',(-0.0531714146829997,0.236972428990521,
8.14455156227216));
#25565=CARTESIAN_POINT('Ctrl Pts',(0.170256666670833,0.173192952787333,
8.13343777321537));
#25566=CARTESIAN_POINT('Ctrl Pts',(0.237846890178926,-0.0491119972437703,
8.12232398415856));
#25567=CARTESIAN_POINT('Ctrl Pts',(0.0877331577390571,-0.22646417922973,
8.11121019510175));
#25568=CARTESIAN_POINT('Ctrl Pts',(-0.138468730552596,-0.19707869266157,
8.10029970973349));
#25569=CARTESIAN_POINT('Ctrl Pts',(-0.205510858353677,-0.064237138716603,
8.0930938207175));
#25570=CARTESIAN_POINT('Ctrl Pts',(-0.205787650466444,6.7877098390855E-5,
8.08959252805377));
#25571=CARTESIAN_POINT('Ctrl Pts',(-0.205725749329808,-0.000120218108977229,
8.16540747194622));
#25572=CARTESIAN_POINT('Ctrl Pts',(-0.205301608939898,0.060897783274676,
8.16208779387343));
#25573=CARTESIAN_POINT('Ctrl Pts',(-0.144200557987511,0.190746562771969,
8.15506351944837));
#25574=CARTESIAN_POINT('Ctrl Pts',(0.0765574282985869,0.230482289451893,
8.14433464867103));
#25575=CARTESIAN_POINT('Ctrl Pts',(0.235161637351955,0.0606805561660993,
8.13322085961422));
#25576=CARTESIAN_POINT('Ctrl Pts',(0.178519732822726,-0.164662778342839,
8.12210707055743));
#25577=CARTESIAN_POINT('Ctrl Pts',(-0.0415233077106159,-0.239288404431658,
8.1109932815006));
#25578=CARTESIAN_POINT('Ctrl Pts',(-0.18729704716622,-0.123655403395563,
8.10209341529689));
#25579=CARTESIAN_POINT('Ctrl Pts',(-0.205319394540154,-0.0276857813902086,
8.09689814544542));
#25580=CARTESIAN_POINT('Ctrl Pts',(-0.205193082001069,-0.000103910388300946,
8.09540747194623));
#25581=CARTESIAN_POINT('Origin',(0.,0.,8.75459252805377));
#25582=CARTESIAN_POINT('',(-0.205557297878076,0.000179913196093145,8.23540747194623));
#25583=CARTESIAN_POINT('',(-0.205263287666448,-0.000148795917841437,8.22959252805377));
#25584=CARTESIAN_POINT('',(-0.205475,1.36055398187253E-14,8.75459252805377));
#25585=CARTESIAN_POINT('Ctrl Pts',(-0.205263287666448,-0.000148795917841445,
8.22959252805377));
#25586=CARTESIAN_POINT('Ctrl Pts',(-0.204964021088784,0.0444940904767351,
8.22717771392578));
#25587=CARTESIAN_POINT('Ctrl Pts',(-0.16869999758381,0.158066853952189,
8.22105830344552));
#25588=CARTESIAN_POINT('Ctrl Pts',(0.0186904834432735,0.242144166292971,
8.21123429661299));
#25589=CARTESIAN_POINT('Ctrl Pts',(0.213575627372185,0.115622587904077,
8.20012050755619));
#25590=CARTESIAN_POINT('Ctrl Pts',(0.212972577454982,-0.11672965644274,
8.18900671849938));
#25591=CARTESIAN_POINT('Ctrl Pts',(0.0174333121199337,-0.24223792244318,
8.17789292944259));
#25592=CARTESIAN_POINT('Ctrl Pts',(-0.169151380035818,-0.157355921249033,
8.16808819929403));
#25593=CARTESIAN_POINT('Ctrl Pts',(-0.204966665148331,-0.0441456674912357,
8.16198806549777));
#25594=CARTESIAN_POINT('Ctrl Pts',(-0.205255455161232,0.000145098000214217,
8.15959252805377));
#25595=CARTESIAN_POINT('Ctrl Pts',(-0.205557297878076,0.000179913196093175,
8.23540747194624));
#25596=CARTESIAN_POINT('Ctrl Pts',(-0.2056789846887,0.013457658201761,8.23468663500598));
#25597=CARTESIAN_POINT('Ctrl Pts',(-0.198456933057522,0.0948418873117451,
8.23026120171346));
#25598=CARTESIAN_POINT('Ctrl Pts',(-0.0898845214982184,0.22561892290705,
8.22213117206865));
#25599=CARTESIAN_POINT('Ctrl Pts',(0.14080680157081,0.197880191555585,8.21101738301186));
#25600=CARTESIAN_POINT('Ctrl Pts',(0.242616062304287,-0.0109805232406446,
8.19990359395504));
#25601=CARTESIAN_POINT('Ctrl Pts',(0.122356089757392,-0.209790640587143,
8.18878980489824));
#25602=CARTESIAN_POINT('Ctrl Pts',(-0.109897799356892,-0.21657700541653,
8.17767601584145));
#25603=CARTESIAN_POINT('Ctrl Pts',(-0.202233319405892,-0.0823136199806689,
8.16988190485743));
#25604=CARTESIAN_POINT('Ctrl Pts',(-0.205774928613328,-0.00719528490585479,
8.16579239022569));
#25605=CARTESIAN_POINT('Ctrl Pts',(-0.205725749329808,-0.000120218108977229,
8.16540747194622));
#25606=CARTESIAN_POINT('Origin',(0.,0.,8.75459252805377));
#25607=CARTESIAN_POINT('',(-0.205141210392772,7.81015472149649E-6,8.30540747194623));
#25608=CARTESIAN_POINT('',(-0.205792375932435,-6.17376947855616E-5,8.29959252805377));
#25609=CARTESIAN_POINT('',(-0.205475,1.36055398187253E-14,8.75459252805377));
#25610=CARTESIAN_POINT('Ctrl Pts',(-0.205792375932435,-6.17376947855664E-5,
8.29959252805376));
#25611=CARTESIAN_POINT('Ctrl Pts',(-0.205536440190278,0.0645933570331749,
8.29607195870605));
#25612=CARTESIAN_POINT('Ctrl Pts',(-0.137843789364693,0.197744956512954,
8.28884679300607));
#25613=CARTESIAN_POINT('Ctrl Pts',(0.088907503777123,0.226005723850825,
8.27791703095381));
#25614=CARTESIAN_POINT('Ctrl Pts',(0.238098615913173,0.0478767223322276,
8.26680324189701));
#25615=CARTESIAN_POINT('Ctrl Pts',(0.169355364681906,-0.174074386095383,
8.2556894528402));
#25616=CARTESIAN_POINT('Ctrl Pts',(-0.0544007724631579,-0.236693234792403,
8.24457566378341));
#25617=CARTESIAN_POINT('Ctrl Pts',(-0.190564537929879,-0.116131675020199,
8.23587668885459));
#25618=CARTESIAN_POINT('Ctrl Pts',(-0.205423129663277,-0.0239931161264832,
8.23088231027804));
#25619=CARTESIAN_POINT('Ctrl Pts',(-0.205263287666448,-0.000148795917841445,
8.22959252805377));
#25620=CARTESIAN_POINT('Ctrl Pts',(-0.205141210392772,7.81015472149649E-6,
8.30540747194623));
#25621=CARTESIAN_POINT('Ctrl Pts',(-0.2051526763295,0.0338265261367679,
8.30358087978625));
#25622=CARTESIAN_POINT('Ctrl Pts',(-0.181235068435874,0.136219282150282,
8.298049691274));
#25623=CARTESIAN_POINT('Ctrl Pts',(-0.0197379877628579,0.242061020031891,
8.28881390640948));
#25624=CARTESIAN_POINT('Ctrl Pts',(0.19266430806168,0.147863416631009,8.27770011735268));
#25625=CARTESIAN_POINT('Ctrl Pts',(0.22871877775246,-0.0816752488934883,
8.26658632829587));
#25626=CARTESIAN_POINT('Ctrl Pts',(0.0554243563205898,-0.236455632847443,
8.25547253923908));
#25627=CARTESIAN_POINT('Ctrl Pts',(-0.154070416783098,-0.178804103481232,
8.24507958712251));
#25628=CARTESIAN_POINT('Ctrl Pts',(-0.205053599820663,-0.0547806394870636,
8.23839123135824));
#25629=CARTESIAN_POINT('Ctrl Pts',(-0.205557297878076,0.000179913196093175,
8.23540747194624));
#25630=CARTESIAN_POINT('Origin',(0.,0.,8.75459252805377));
#25631=CARTESIAN_POINT('',(-0.205528628934285,-0.000183968246708688,8.37540747194623));
#25632=CARTESIAN_POINT('',(-0.205445190560286,0.000187702189675683,8.36959252805377));
#25633=CARTESIAN_POINT('',(-0.205475,1.36055398187253E-14,8.75459252805377));
#25634=CARTESIAN_POINT('Ctrl Pts',(-0.205445190560286,0.000187702189675667,
8.36959252805377));
#25635=CARTESIAN_POINT('Ctrl Pts',(-0.205599100693057,0.0171896010410893,
8.3686707998386));
#25636=CARTESIAN_POINT('Ctrl Pts',(-0.195892182403793,0.102351934160262,
8.36404447527116));
#25637=CARTESIAN_POINT('Ctrl Pts',(-0.0775539386019673,0.230148904034816,
8.35571355435145));
#25638=CARTESIAN_POINT('Ctrl Pts',(0.151300115555386,0.189977384132442,
8.34459976529464));
#25639=CARTESIAN_POINT('Ctrl Pts',(0.241667458088899,-0.0240825900331494,
8.33348597623784));
#25640=CARTESIAN_POINT('Ctrl Pts',(0.110833835536237,-0.216099496387572,
8.32237218718103));
#25641=CARTESIAN_POINT('Ctrl Pts',(-0.121447253622906,-0.210318082982978,
8.31125839812424));
#25642=CARTESIAN_POINT('Ctrl Pts',(-0.204198823013731,-0.0748427841522689,
8.30366517841514));
#25643=CARTESIAN_POINT('Ctrl Pts',(-0.205805754191272,-0.00344138519968516,
8.29977655505832));
#25644=CARTESIAN_POINT('Ctrl Pts',(-0.205792375932435,-6.17376947855664E-5,
8.29959252805376));
#25645=CARTESIAN_POINT('Ctrl Pts',(-0.205528628934285,-0.000183968246708686,
8.37540747194623));
#25646=CARTESIAN_POINT('Ctrl Pts',(-0.205029971468385,0.0538489651766571,
8.37247512456652));
#25647=CARTESIAN_POINT('Ctrl Pts',(-0.155498687892329,0.176953566042901,
8.36583818083455));
#25648=CARTESIAN_POINT('Ctrl Pts',(0.05214561050461,0.237200254924533,8.35549664075031));
#25649=CARTESIAN_POINT('Ctrl Pts',(0.22756616748523,0.0848337492213278,
8.3443828516935));
#25650=CARTESIAN_POINT('Ctrl Pts',(0.19469283040568,-0.145182048984365,
8.3332690626367));
#25651=CARTESIAN_POINT('Ctrl Pts',(-0.016385062217743,-0.242311071399234,
8.3221552735799));
#25652=CARTESIAN_POINT('Ctrl Pts',(-0.180238976017125,-0.138138524644507,
8.31286807668307));
#25653=CARTESIAN_POINT('Ctrl Pts',(-0.205129421730959,-0.0347627816519641,
8.30728547613852));
#25654=CARTESIAN_POINT('Ctrl Pts',(-0.205141210392772,7.81015472149649E-6,
8.30540747194623));
#25655=CARTESIAN_POINT('Origin',(0.,0.,8.75459252805377));
#25656=CARTESIAN_POINT('',(-0.205746142027763,0.000106562949819478,8.44540747194623));
#25657=CARTESIAN_POINT('',(-0.205153388991823,-5.25555079458241E-5,8.43959252805377));
#25658=CARTESIAN_POINT('',(-0.205475,1.36055398187253E-14,8.75459252805377));
#25659=CARTESIAN_POINT('Ctrl Pts',(-0.205153388991823,-5.25555079458132E-5,
8.43959252805377));
#25660=CARTESIAN_POINT('Ctrl Pts',(-0.205067466342422,0.0374800397938141,
8.43756504461887));
#25661=CARTESIAN_POINT('Ctrl Pts',(-0.177236782892462,0.143710413212875,
8.43183296483171));
#25662=CARTESIAN_POINT('Ctrl Pts',(-0.00662099741593451,0.242774159607174,
8.42239628869227));
#25663=CARTESIAN_POINT('Ctrl Pts',(0.200377384150519,0.13722986443753,8.41128249963547));
#25664=CARTESIAN_POINT('Ctrl Pts',(0.223968073814581,-0.0939224866161797,
8.40016871057866));
#25665=CARTESIAN_POINT('Ctrl Pts',(0.0425582454220915,-0.239106518161268,
8.38905492152186));
#25666=CARTESIAN_POINT('Ctrl Pts',(-0.15952962843628,-0.171543743623583,
8.37886286068023));
#25667=CARTESIAN_POINT('Ctrl Pts',(-0.204980507373406,-0.0511441782984296,
8.37237539619086));
#25668=CARTESIAN_POINT('Ctrl Pts',(-0.205445190560286,0.000187702189675667,
8.36959252805377));
#25669=CARTESIAN_POINT('Ctrl Pts',(-0.205746142027763,0.000106562949819445,
8.44540747194623));
#25670=CARTESIAN_POINT('Ctrl Pts',(-0.205784824946164,0.00623504139834656,
8.44507396569907));
#25671=CARTESIAN_POINT('Ctrl Pts',(-0.202756731895245,0.0804000642300188,
8.44103586309964));
#25672=CARTESIAN_POINT('Ctrl Pts',(-0.112885495048793,0.215034836414334,
8.43329316414793));
#25673=CARTESIAN_POINT('Ctrl Pts',(0.119440067448933,0.211464412612195,
8.42217937509113));
#25674=CARTESIAN_POINT('Ctrl Pts',(0.242440804004482,0.0143381848173731,
8.41106558603433));
#25675=CARTESIAN_POINT('Ctrl Pts',(0.143532711926644,-0.195911931545135,
8.39995179697752));
#25676=CARTESIAN_POINT('Ctrl Pts',(-0.0867524934706339,-0.226841642534413,
8.38883800792072));
#25677=CARTESIAN_POINT('Ctrl Pts',(-0.197822911553203,-0.0967627749490978,
8.38065656624362));
#25678=CARTESIAN_POINT('Ctrl Pts',(-0.205659952978076,-0.0144138230072569,
8.37617972091879));
#25679=CARTESIAN_POINT('Ctrl Pts',(-0.205528628934285,-0.000183968246708686,
8.37540747194623));
#25680=CARTESIAN_POINT('Origin',(0.,0.,8.75459252805377));
#25681=CARTESIAN_POINT('',(-0.205208153945529,0.000116160874735274,8.51540747194623));
#25682=CARTESIAN_POINT('',(-0.205637856381221,-0.00016039379494083,8.50959252805377));
#25683=CARTESIAN_POINT('',(-0.205475,1.36055398187253E-14,8.75459252805377));
#25684=CARTESIAN_POINT('Ctrl Pts',(-0.205637856381221,-0.000160393794940828,
8.50959252805377));
#25685=CARTESIAN_POINT('Ctrl Pts',(-0.205143095125645,0.0574950566938362,
8.50645928939915));
#25686=CARTESIAN_POINT('Ctrl Pts',(-0.14979446013605,0.184152224411407,
8.49962145439225));
#25687=CARTESIAN_POINT('Ctrl Pts',(0.0648946403841687,0.234033639096515,
8.48907902303309));
#25688=CARTESIAN_POINT('Ctrl Pts',(0.231820203331014,0.0724053476422597,
8.4779652339763));
#25689=CARTESIAN_POINT('Ctrl Pts',(0.18655812004824,-0.155496664131617,
8.46685144491948));
#25690=CARTESIAN_POINT('Ctrl Pts',(-0.0294627337392764,-0.241070672344369,
8.45573765586269));
#25691=CARTESIAN_POINT('Ctrl Pts',(-0.184027107137038,-0.130632731643015,
8.44665135024078));
#25692=CARTESIAN_POINT('Ctrl Pts',(-0.205224463301346,-0.031099122557323,
8.44126964097114));
#25693=CARTESIAN_POINT('Ctrl Pts',(-0.205153388991823,-5.25555079458132E-5,
8.43959252805377));
#25694=CARTESIAN_POINT('Ctrl Pts',(-0.205208153945529,0.00011616087473525,
8.51540747194623));
#25695=CARTESIAN_POINT('Ctrl Pts',(-0.205345942894438,0.0267421115464025,
8.51396821047934));
#25696=CARTESIAN_POINT('Ctrl Pts',(-0.188159225831614,0.121731577366826,
8.50882435266019));
#25697=CARTESIAN_POINT('Ctrl Pts',(-0.0448312245259985,0.238689656539759,
8.49997589848875));
#25698=CARTESIAN_POINT('Ctrl Pts',(0.176222693303572,0.167118876029215,
8.48886210943197));
#25699=CARTESIAN_POINT('Ctrl Pts',(0.235979340716847,-0.0574194692648986,
8.47774832037514));
#25700=CARTESIAN_POINT('Ctrl Pts',(0.0797407360187229,-0.229400234578822,
8.46663453131836));
#25701=CARTESIAN_POINT('Ctrl Pts',(-0.14260643792996,-0.192548870793535,
8.4558542485087));
#25702=CARTESIAN_POINT('Ctrl Pts',(-0.205355134049455,-0.0618402618335321,
8.44877856205133));
#25703=CARTESIAN_POINT('Ctrl Pts',(-0.205746142027763,0.000106562949819445,
8.44540747194623));
#25704=CARTESIAN_POINT('Origin',(0.,0.,8.75459252805377));
#25705=CARTESIAN_POINT('',(-0.205267617401664,-0.000235214789251412,8.58540747194623));
#25706=CARTESIAN_POINT('',(-0.205656479110814,0.00014959981056081,8.57959252805377));
#25707=CARTESIAN_POINT('',(-0.205475,1.36055398187253E-14,8.75459252805377));
#25708=CARTESIAN_POINT('',(-0.0530170217188482,-0.198517432567176,8.6));
#25709=CARTESIAN_POINT('Ctrl Pts',(-0.0530170217188485,-0.198517432567176,
8.6));
#25710=CARTESIAN_POINT('Ctrl Pts',(-0.119028790974543,-0.180888011517996,
8.59629540364773));
#25711=CARTESIAN_POINT('Ctrl Pts',(-0.192495809737496,-0.111280924019936,
8.59143122762981));
#25712=CARTESIAN_POINT('Ctrl Pts',(-0.205429477035024,-0.0216596338882675,
8.58656705161189));
#25713=CARTESIAN_POINT('Ctrl Pts',(-0.205267617401664,-0.000235214789251429,
8.58540747194623));
#25714=CARTESIAN_POINT('',(0.0531303528054007,-0.198873455395433,8.6));
#25715=CARTESIAN_POINT('Origin',(0.,0.,8.6));
#25716=CARTESIAN_POINT('Ctrl Pts',(0.0531304158591932,-0.198873653475093,
8.6));
#25717=CARTESIAN_POINT('Ctrl Pts',(-0.0113304135988541,-0.216006401657972,
8.59636770818144));
#25718=CARTESIAN_POINT('Ctrl Pts',(-0.149305780278568,-0.184063659998061,
8.58956521753269));
#25719=CARTESIAN_POINT('Ctrl Pts',(-0.205170728792184,-0.0581586047744906,
8.58276272688396));
#25720=CARTESIAN_POINT('Ctrl Pts',(-0.205656479110814,0.000149599810560773,
8.57959252805377));
#25721=CARTESIAN_POINT('Origin',(0.6,1.,2.15));
#25722=CARTESIAN_POINT('',(0.473748222256554,0.999995809921948,2.01934196736194));
#25723=CARTESIAN_POINT('',(0.473622351265484,0.999839631194249,2.00565803263806));
#25724=CARTESIAN_POINT('',(0.47355,1.,2.15));
#25725=CARTESIAN_POINT('',(0.504188384727762,1.08252112989365,2.));
#25726=CARTESIAN_POINT('Ctrl Pts',(0.473622351265484,0.999839631194249,
2.00565803263806));
#25727=CARTESIAN_POINT('Ctrl Pts',(0.473885391482026,1.02975027328269,2.00377202175871));
#25728=CARTESIAN_POINT('Ctrl Pts',(0.484630619730662,1.05981347843636,2.00188601087935));
#25729=CARTESIAN_POINT('Ctrl Pts',(0.504188384727762,1.08252112989365,2.));
#25730=CARTESIAN_POINT('',(0.695988975197609,1.08263517233072,2.));
#25731=CARTESIAN_POINT('Origin',(0.6,1.,2.));
#25732=CARTESIAN_POINT('Ctrl Pts',(0.69598984030289,1.08263572859344,2.));
#25733=CARTESIAN_POINT('Ctrl Pts',(0.670163701400848,1.11242100165145,2.0024908160387));
#25734=CARTESIAN_POINT('Ctrl Pts',(0.629259702670384,1.12936970915052,2.0049816320774));
#25735=CARTESIAN_POINT('Ctrl Pts',(0.589969605604523,1.12624206673302,2.0074724481161));
#25736=CARTESIAN_POINT('Ctrl Pts',(0.548691445154515,1.12295616684523,2.01008929846199));
#25737=CARTESIAN_POINT('Ctrl Pts',(0.509194644046665,1.09751080441727,2.01270614880789));
#25738=CARTESIAN_POINT('Ctrl Pts',(0.489166147389288,1.06128256435802,2.01532299915378));
#25739=CARTESIAN_POINT('Ctrl Pts',(0.478912868232585,1.04273607706854,2.01666265522317));
#25740=CARTESIAN_POINT('Ctrl Pts',(0.473761783314308,1.02136364588323,2.01800231129256));
#25741=CARTESIAN_POINT('Ctrl Pts',(0.473748222256554,0.999995809921948,
2.01934196736194));
#25742=CARTESIAN_POINT('Origin',(0.6,1.,2.15));
#25743=CARTESIAN_POINT('',(0.473418004372097,0.999922226677399,2.06934196736194));
#25744=CARTESIAN_POINT('',(0.473391518308752,1.00006258785156,2.05565803263806));
#25745=CARTESIAN_POINT('',(0.47355,1.,2.15));
#25746=CARTESIAN_POINT('Ctrl Pts',(0.473391518308752,1.00006258785156,2.05565803263806));
#25747=CARTESIAN_POINT('Ctrl Pts',(0.473368951434719,1.00377931266751,2.05542330751329));
#25748=CARTESIAN_POINT('Ctrl Pts',(0.473518765465857,1.00749417831325,2.05518858238852));
#25749=CARTESIAN_POINT('Ctrl Pts',(0.473846950690071,1.01119320034366,2.05495385726375));
#25750=CARTESIAN_POINT('Ctrl Pts',(0.477505747839885,1.05243201995956,2.05233700691785));
#25751=CARTESIAN_POINT('Ctrl Pts',(0.503334424526069,1.09170162561774,2.04972015657196));
#25752=CARTESIAN_POINT('Ctrl Pts',(0.539751219345993,1.1113984538297,2.04710330622607));
#25753=CARTESIAN_POINT('Ctrl Pts',(0.576168014165918,1.13109528204167,2.04448645588018));
#25754=CARTESIAN_POINT('Ctrl Pts',(0.623172927119585,1.13121933280741,2.04186960553428));
#25755=CARTESIAN_POINT('Ctrl Pts',(0.659688152943108,1.11170438100077,2.03925275518839));
#25756=CARTESIAN_POINT('Ctrl Pts',(0.69620337876663,1.09218942919414,2.0366359048425));
#25757=CARTESIAN_POINT('Ctrl Pts',(0.722228917460009,1.05303547481514,2.0340190544966));
#25758=CARTESIAN_POINT('Ctrl Pts',(0.726095080681017,1.01182045619333,2.03140220415071));
#25759=CARTESIAN_POINT('Ctrl Pts',(0.729961243902025,0.970605437571516,
2.02878535380482));
#25760=CARTESIAN_POINT('Ctrl Pts',(0.711668031650661,0.927329354706896,
2.02616850345893));
#25761=CARTESIAN_POINT('Ctrl Pts',(0.679417475504429,0.901356588462624,
2.02355165311304));
#25762=CARTESIAN_POINT('Ctrl Pts',(0.647166919358198,0.875383822218351,
2.02093480276714));
#25763=CARTESIAN_POINT('Ctrl Pts',(0.600959019317099,0.866714372594425,
2.01831795242125));
#25764=CARTESIAN_POINT('Ctrl Pts',(0.561514908627169,0.879318620323889,
2.01570110207536));
#25765=CARTESIAN_POINT('Ctrl Pts',(0.522070797937238,0.891922868053354,
2.01308425172946));
#25766=CARTESIAN_POINT('Ctrl Pts',(0.489390476598475,0.925800813136209,
2.01046740138357));
#25767=CARTESIAN_POINT('Ctrl Pts',(0.47813574698779,0.965573631142046,2.00785055103768));
#25768=CARTESIAN_POINT('Ctrl Pts',(0.474992502439002,0.976681467377235,
2.00711971157114));
#25769=CARTESIAN_POINT('Ctrl Pts',(0.473520421751905,0.988249094815541,
2.0063888721046));
#25770=CARTESIAN_POINT('Ctrl Pts',(0.473622351265484,0.999839631194249,
2.00565803263806));
#25771=CARTESIAN_POINT('Ctrl Pts',(0.473748222256554,0.999995809921948,
2.01934196736194));
#25772=CARTESIAN_POINT('Ctrl Pts',(0.473735293486444,0.979624254554346,
2.02061916163845));
#25773=CARTESIAN_POINT('Ctrl Pts',(0.478391980488661,0.959256875893503,
2.02189635591496));
#25774=CARTESIAN_POINT('Ctrl Pts',(0.487748897958052,0.941346462457022,
2.02317355019146));
#25775=CARTESIAN_POINT('Ctrl Pts',(0.5069203373911,0.904649718305799,2.02579040053735));
#25776=CARTESIAN_POINT('Ctrl Pts',(0.545823408464101,0.878267347693885,
2.02840725088324));
#25777=CARTESIAN_POINT('Ctrl Pts',(0.587007341569528,0.874020924816605,
2.03102410122914));
#25778=CARTESIAN_POINT('Ctrl Pts',(0.628191274674955,0.869774501939324,
2.03364095157503));
#25779=CARTESIAN_POINT('Ctrl Pts',(0.671656069812808,0.887664026796678,
2.03625780192092));
#25780=CARTESIAN_POINT('Ctrl Pts',(0.697914735578316,0.919671996193035,
2.03887465226682));
#25781=CARTESIAN_POINT('Ctrl Pts',(0.724173401343824,0.951679965589392,
2.04149150261271));
#25782=CARTESIAN_POINT('Ctrl Pts',(0.733225937736988,0.997806379524751,
2.0441083529586));
#25783=CARTESIAN_POINT('Ctrl Pts',(0.72101148240133,1.03736538090912,2.04672520330449));
#25784=CARTESIAN_POINT('Ctrl Pts',(0.708797027065672,1.07692438229349,2.04934205365039));
#25785=CARTESIAN_POINT('Ctrl Pts',(0.675315580001192,1.10991597112687,2.05195890399628));
#25786=CARTESIAN_POINT('Ctrl Pts',(0.635581432895856,1.12154745886576,2.05457575434217));
#25787=CARTESIAN_POINT('Ctrl Pts',(0.59584728579052,1.13317894660465,2.05719260468807));
#25788=CARTESIAN_POINT('Ctrl Pts',(0.549860438644329,1.12345033324905,2.05980945503396));
#25789=CARTESIAN_POINT('Ctrl Pts',(0.518241526751132,1.09672346863534,2.06242630537985));
#25790=CARTESIAN_POINT('Ctrl Pts',(0.490387977892526,1.07317939375162,2.06473152604054));
#25791=CARTESIAN_POINT('Ctrl Pts',(0.473684088301786,1.03644450847376,2.06703674670124));
#25792=CARTESIAN_POINT('Ctrl Pts',(0.473418004372097,0.999922226677399,
2.06934196736194));
#25793=CARTESIAN_POINT('Origin',(0.6,1.,2.15));
#25794=CARTESIAN_POINT('',(0.473569322058917,1.00010891293128,2.11934196736194));
#25795=CARTESIAN_POINT('',(0.473740555540666,1.00002674768131,2.10565803263806));
#25796=CARTESIAN_POINT('',(0.47355,1.,2.15));
#25797=CARTESIAN_POINT('Ctrl Pts',(0.473740555540666,1.00002674768131,2.10565803263806));
#25798=CARTESIAN_POINT('Ctrl Pts',(0.473703568953707,1.01916777914625,2.10445774292198));
#25799=CARTESIAN_POINT('Ctrl Pts',(0.477794964495735,1.03829380542625,2.10325745320589));
#25800=CARTESIAN_POINT('Ctrl Pts',(0.486097635636878,1.0553725521712,2.10205716348981));
#25801=CARTESIAN_POINT('Ctrl Pts',(0.504198971969625,1.09260733284801,2.09944031314392));
#25802=CARTESIAN_POINT('Ctrl Pts',(0.542317321105284,1.12011099531618,2.09682346279803));
#25803=CARTESIAN_POINT('Ctrl Pts',(0.583359964347627,1.12555066422426,2.09420661245214));
#25804=CARTESIAN_POINT('Ctrl Pts',(0.62440260758997,1.13099033313234,2.09158976210624));
#25805=CARTESIAN_POINT('Ctrl Pts',(0.668369544938998,1.11436600848032,2.08897291176035));
#25806=CARTESIAN_POINT('Ctrl Pts',(0.695545474812698,1.08313205071709,2.08635606141446));
#25807=CARTESIAN_POINT('Ctrl Pts',(0.722721404686398,1.05189809295385,2.08373921106856));
#25808=CARTESIAN_POINT('Ctrl Pts',(0.733106327084771,1.00605450207939,2.08112236072267));
#25809=CARTESIAN_POINT('Ctrl Pts',(0.722043527705466,0.966158451314527,
2.07850551037678));
#25810=CARTESIAN_POINT('Ctrl Pts',(0.71098072832616,0.926262400549665,2.07588866003089));
#25811=CARTESIAN_POINT('Ctrl Pts',(0.678470207169174,0.892313889894401,
2.073271809685));
#25812=CARTESIAN_POINT('Ctrl Pts',(0.639090051974211,0.87953512362367,2.0706549593391));
#25813=CARTESIAN_POINT('Ctrl Pts',(0.599709896779248,0.86675635735294,2.06803810899321));
#25814=CARTESIAN_POINT('Ctrl Pts',(0.553460107546307,0.875147335466744,
2.06542125864732));
#25815=CARTESIAN_POINT('Ctrl Pts',(0.52107967173656,0.900946841310449,2.06280440830142));
#25816=CARTESIAN_POINT('Ctrl Pts',(0.491603682429651,0.924432194096951,
2.0604222830803));
#25817=CARTESIAN_POINT('Ctrl Pts',(0.473620539892396,0.962343132242784,
2.05804015785918));
#25818=CARTESIAN_POINT('Ctrl Pts',(0.473391518308752,1.00006258785156,2.05565803263806));
#25819=CARTESIAN_POINT('Ctrl Pts',(0.473418004372097,0.999922226677399,
2.06934196736194));
#25820=CARTESIAN_POINT('Ctrl Pts',(0.473382033997262,0.994984986883897,
2.06965359704714));
#25821=CARTESIAN_POINT('Ctrl Pts',(0.473646461235087,0.990051632376521,
2.06996522673233));
#25822=CARTESIAN_POINT('Ctrl Pts',(0.474224350273596,0.985155275839,2.07027685641753));
#25823=CARTESIAN_POINT('Ctrl Pts',(0.47907706232946,0.944039063528183,2.07289370676342));
#25824=CARTESIAN_POINT('Ctrl Pts',(0.50603346308139,0.905531754778367,2.07551055710931));
#25825=CARTESIAN_POINT('Ctrl Pts',(0.543005874916624,0.886900335416373,
2.0781274074552));
#25826=CARTESIAN_POINT('Ctrl Pts',(0.579978286751859,0.868268916054378,
2.0807442578011));
#25827=CARTESIAN_POINT('Ctrl Pts',(0.626966709670398,0.869513386080205,
2.08336110814699));
#25828=CARTESIAN_POINT('Ctrl Pts',(0.662901030784248,0.890075786233013,
2.08597795849288));
#25829=CARTESIAN_POINT('Ctrl Pts',(0.698835351898097,0.910638186385821,
2.08859480883878));
#25830=CARTESIAN_POINT('Ctrl Pts',(0.723715571207256,0.95051851666561,2.09121165918467));
#25831=CARTESIAN_POINT('Ctrl Pts',(0.726385074899299,0.991833924307951,
2.09382850953056));
#25832=CARTESIAN_POINT('Ctrl Pts',(0.729054578591342,1.03314933195029,2.09644535987645));
#25833=CARTESIAN_POINT('Ctrl Pts',(0.709513366666269,1.07589981695519,2.09906221022235));
#25834=CARTESIAN_POINT('Ctrl Pts',(0.676523964943026,1.10091557332887,2.10167906056824));
#25835=CARTESIAN_POINT('Ctrl Pts',(0.643534563219784,1.12593132970255,2.10429591091413));
#25836=CARTESIAN_POINT('Ctrl Pts',(0.597096971698373,1.13321235744502,2.10691276126002));
#25837=CARTESIAN_POINT('Ctrl Pts',(0.558034351233094,1.1194937471697,2.10952961160592));
#25838=CARTESIAN_POINT('Ctrl Pts',(0.518971730767816,1.10577513689439,2.11214646195181));
#25839=CARTESIAN_POINT('Ctrl Pts',(0.48728408135867,1.0710568886013,2.1147633122977));
#25840=CARTESIAN_POINT('Ctrl Pts',(0.477180525319141,1.0309070826023,2.11738016264359));
#25841=CARTESIAN_POINT('Ctrl Pts',(0.474655708422174,1.02087389149615,2.11803409754971));
#25842=CARTESIAN_POINT('Ctrl Pts',(0.473478752433508,1.01050151615012,2.11868803245583));
#25843=CARTESIAN_POINT('Ctrl Pts',(0.473569322058917,1.00010891293128,2.11934196736194));
#25844=CARTESIAN_POINT('Origin',(0.6,1.,2.15));
#25845=CARTESIAN_POINT('',(0.473701319324768,0.999928563934628,2.16934196736194));
#25846=CARTESIAN_POINT('',(0.473475969746711,0.999901036847401,2.15565803263806));
#25847=CARTESIAN_POINT('',(0.47355,1.,2.15));
#25848=CARTESIAN_POINT('Ctrl Pts',(0.473475969746711,0.999901036847401,
2.15565803263806));
#25849=CARTESIAN_POINT('Ctrl Pts',(0.473771376261924,1.03425627771038,2.15349217833067));
#25850=CARTESIAN_POINT('Ctrl Pts',(0.488302943448428,1.0688317671636,2.15132632402327));
#25851=CARTESIAN_POINT('Ctrl Pts',(0.513274800541643,1.09229629753053,2.14916046971588));
#25852=CARTESIAN_POINT('Ctrl Pts',(0.543446549698046,1.12064684917997,2.14654361936999));
#25853=CARTESIAN_POINT('Ctrl Pts',(0.588859242361366,1.13277740107318,2.1439267690241));
#25854=CARTESIAN_POINT('Ctrl Pts',(0.629149287366476,1.12324847117969,2.1413099186782));
#25855=CARTESIAN_POINT('Ctrl Pts',(0.669439332371586,1.11371954128621,2.13869306833231));
#25856=CARTESIAN_POINT('Ctrl Pts',(0.704606729718486,1.08253112960603,2.13607621798642));
#25857=CARTESIAN_POINT('Ctrl Pts',(0.718882000334445,1.04366848746118,2.13345936764053));
#25858=CARTESIAN_POINT('Ctrl Pts',(0.733157270950405,1.00480584531632,2.13084251729463));
#25859=CARTESIAN_POINT('Ctrl Pts',(0.726540414835423,0.958268972706794,
2.12822566694874));
#25860=CARTESIAN_POINT('Ctrl Pts',(0.701998509069979,0.924925562785253,
2.12560881660285));
#25861=CARTESIAN_POINT('Ctrl Pts',(0.677456603304535,0.891582152863712,
2.12299196625696));
#25862=CARTESIAN_POINT('Ctrl Pts',(0.634989647888627,0.871432205630162,
2.12037511591106));
#25863=CARTESIAN_POINT('Ctrl Pts',(0.59364033014263,0.873511184567866,2.11775826556517));
#25864=CARTESIAN_POINT('Ctrl Pts',(0.552291012396633,0.87559016350557,2.11514141521928));
#25865=CARTESIAN_POINT('Ctrl Pts',(0.512059332320547,0.899898068614528,
2.11252456487339));
#25866=CARTESIAN_POINT('Ctrl Pts',(0.490985654047422,0.935534970611733,
2.10990771452749));
#25867=CARTESIAN_POINT('Ctrl Pts',(0.479577992537903,0.954826036459998,
2.10849115389768));
#25868=CARTESIAN_POINT('Ctrl Pts',(0.473784206454455,0.977436841907783,
2.10707459326787));
#25869=CARTESIAN_POINT('Ctrl Pts',(0.473740555540666,1.00002674768131,2.10565803263806));
#25870=CARTESIAN_POINT('Ctrl Pts',(0.473569322058917,1.00010891293128,2.11934196736194));
#25871=CARTESIAN_POINT('Ctrl Pts',(0.473841184769449,0.968913451231703,
2.12130488280172));
#25872=CARTESIAN_POINT('Ctrl Pts',(0.485533699168036,0.937535732473691,
2.1232677982415));
#25873=CARTESIAN_POINT('Ctrl Pts',(0.506474126044697,0.914602214201428,
2.12523071368127));
#25874=CARTESIAN_POINT('Ctrl Pts',(0.534390745479694,0.884028515504489,
2.12784756402717));
#25875=CARTESIAN_POINT('Ctrl Pts',(0.578743447019601,0.868462481815532,
2.13046441437306));
#25876=CARTESIAN_POINT('Ctrl Pts',(0.619643953027205,0.874884108988649,
2.13308126471895));
#25877=CARTESIAN_POINT('Ctrl Pts',(0.660544459034809,0.881305736161766,
2.13569811506484));
#25878=CARTESIAN_POINT('Ctrl Pts',(0.697992769510109,0.909715024196956,
2.13831496541074));
#25879=CARTESIAN_POINT('Ctrl Pts',(0.715196616413391,0.947372909972802,
2.14093181575663));
#25880=CARTESIAN_POINT('Ctrl Pts',(0.732400463316672,0.985030795748647,
2.14354866610252));
#25881=CARTESIAN_POINT('Ctrl Pts',(0.729359846647935,1.03193727926515,2.14616551644841));
#25882=CARTESIAN_POINT('Ctrl Pts',(0.707438215309595,1.0670589360858,2.14878236679431));
#25883=CARTESIAN_POINT('Ctrl Pts',(0.685516583971256,1.10218059290645,2.1513992171402));
#25884=CARTESIAN_POINT('Ctrl Pts',(0.644713937963314,1.12551742303125,2.15401606748609));
#25885=CARTESIAN_POINT('Ctrl Pts',(0.603326668644815,1.12660491425775,2.15663291783199));
#25886=CARTESIAN_POINT('Ctrl Pts',(0.561939399326316,1.12769240548424,2.15924976817788));
#25887=CARTESIAN_POINT('Ctrl Pts',(0.51996750669726,1.10653055781244,2.16186661852377));
#25888=CARTESIAN_POINT('Ctrl Pts',(0.496231686388225,1.07260859537424,2.16448346886966));
#25889=CARTESIAN_POINT('Ctrl Pts',(0.481542214702607,1.05161518961582,2.16610296836709));
#25890=CARTESIAN_POINT('Ctrl Pts',(0.473837240540682,1.02573460264732,2.16772246786452));
#25891=CARTESIAN_POINT('Ctrl Pts',(0.473701319324768,0.999928563934628,
2.16934196736194));
#25892=CARTESIAN_POINT('Origin',(0.6,1.,2.15));
#25893=CARTESIAN_POINT('',(0.473352235667534,0.999991049382066,2.21934196736194));
#25894=CARTESIAN_POINT('',(0.473504867419963,1.00010483506638,2.20565803263806));
#25895=CARTESIAN_POINT('',(0.47355,1.,2.15));
#25896=CARTESIAN_POINT('Ctrl Pts',(0.473504867419963,1.00010483506638,2.20565803263806));
#25897=CARTESIAN_POINT('Ctrl Pts',(0.473432601452696,1.00827186028206,2.20514346408525));
#25898=CARTESIAN_POINT('Ctrl Pts',(0.474157534286366,1.01642611923938,2.20462889553244));
#25899=CARTESIAN_POINT('Ctrl Pts',(0.475726914006531,1.02441447959464,2.20411432697963));
#25900=CARTESIAN_POINT('Ctrl Pts',(0.48370803108242,1.0650394720171,2.20149747663373));
#25901=CARTESIAN_POINT('Ctrl Pts',(0.513528695332623,1.10137390406913,2.19888062628784));
#25902=CARTESIAN_POINT('Ctrl Pts',(0.551816966436341,1.11712498450026,2.19626377594195));
#25903=CARTESIAN_POINT('Ctrl Pts',(0.59010523754006,1.1328760649314,2.19364692559606));
#25904=CARTESIAN_POINT('Ctrl Pts',(0.636861115497294,1.12804379374164,2.19103007525016));
#25905=CARTESIAN_POINT('Ctrl Pts',(0.671118708852879,1.10479501880275,2.18841322490427));
#25906=CARTESIAN_POINT('Ctrl Pts',(0.705376302208464,1.08154624386386,2.18579637455838));
#25907=CARTESIAN_POINT('Ctrl Pts',(0.7271356109624,1.03988096517584,2.18317952421248));
#25908=CARTESIAN_POINT('Ctrl Pts',(0.726639502419725,0.998482388913484,
2.18056267386659));
#25909=CARTESIAN_POINT('Ctrl Pts',(0.726143393877049,0.95708381265113,2.1779458235207));
#25910=CARTESIAN_POINT('Ctrl Pts',(0.703391868037763,0.915951938814441,
2.17532897317481));
#25911=CARTESIAN_POINT('Ctrl Pts',(0.668586979533722,0.893530788668923,
2.17271212282892));
#25912=CARTESIAN_POINT('Ctrl Pts',(0.63378209102968,0.871109638523405,2.17009527248302));
#25913=CARTESIAN_POINT('Ctrl Pts',(0.586923839860883,0.867399212069058,
2.16747842213713));
#25914=CARTESIAN_POINT('Ctrl Pts',(0.549024022842182,0.88406330841772,2.16486157179124));
#25915=CARTESIAN_POINT('Ctrl Pts',(0.511124205823482,0.900727404766382,
2.16224472144534));
#25916=CARTESIAN_POINT('Ctrl Pts',(0.482182822954877,0.937766023918054,
2.15962787109945));
#25917=CARTESIAN_POINT('Ctrl Pts',(0.475177534345317,0.978570609196729,
2.15701102075356));
#25918=CARTESIAN_POINT('Ctrl Pts',(0.473970221356853,0.985602996945691,
2.15656002471506));
#25919=CARTESIAN_POINT('Ctrl Pts',(0.473414457221305,0.992747241932372,
2.15610902867656));
#25920=CARTESIAN_POINT('Ctrl Pts',(0.473475969746711,0.999901036847401,
2.15565803263806));
#25921=CARTESIAN_POINT('Ctrl Pts',(0.473701319324768,0.999928563934628,
2.16934196736194));
#25922=CARTESIAN_POINT('Ctrl Pts',(0.473617613747686,0.984036200493609,
2.17033931821041));
#25923=CARTESIAN_POINT('Ctrl Pts',(0.476404528994482,0.968172110044866,
2.17133666905888));
#25924=CARTESIAN_POINT('Ctrl Pts',(0.482198594761734,0.953495162034513,
2.17233401990734));
#25925=CARTESIAN_POINT('Ctrl Pts',(0.497401071433289,0.914985768337587,
2.17495087025323));
#25926=CARTESIAN_POINT('Ctrl Pts',(0.533305772765409,0.884649058148337,
2.17756772059913));
#25927=CARTESIAN_POINT('Ctrl Pts',(0.573812603904437,0.876088372947374,
2.18018457094502));
#25928=CARTESIAN_POINT('Ctrl Pts',(0.614319435043466,0.86752768774641,2.18280142129091));
#25929=CARTESIAN_POINT('Ctrl Pts',(0.659428395989404,0.880743027533735,
2.1854182716368));
#25930=CARTESIAN_POINT('Ctrl Pts',(0.688912092443748,0.909808476845009,
2.1880351219827));
#25931=CARTESIAN_POINT('Ctrl Pts',(0.718395788898092,0.938873926156282,
2.19065197232859));
#25932=CARTESIAN_POINT('Ctrl Pts',(0.732254220860843,0.983789484991505,
2.19326882267448));
#25933=CARTESIAN_POINT('Ctrl Pts',(0.724273102711297,1.02441448287903,2.19588567302037));
#25934=CARTESIAN_POINT('Ctrl Pts',(0.716291984561752,1.06503948076655,2.19850252336627));
#25935=CARTESIAN_POINT('Ctrl Pts',(0.686471316299909,1.10137391770637,2.20111937371216));
#25936=CARTESIAN_POINT('Ctrl Pts',(0.648183040045466,1.11712500025644,2.20373622405805));
#25937=CARTESIAN_POINT('Ctrl Pts',(0.609894763791023,1.13287608280652,2.20635307440395));
#25938=CARTESIAN_POINT('Ctrl Pts',(0.563138879543981,1.12804381096685,2.20896992474984));
#25939=CARTESIAN_POINT('Ctrl Pts',(0.528881281579892,1.10479503290036,2.21158677509573));
#25940=CARTESIAN_POINT('Ctrl Pts',(0.49503980248944,1.0818286521973,2.21417183918447));
#25941=CARTESIAN_POINT('Ctrl Pts',(0.473394826320348,1.04089044984514,2.2167569032732));
#25942=CARTESIAN_POINT('Ctrl Pts',(0.473352235667534,0.999991049382066,
2.21934196736194));
#25943=CARTESIAN_POINT('Origin',(0.6,1.,2.15));
#25944=CARTESIAN_POINT('',(0.473682079464411,1.00008273769678,2.26934196736194));
#25945=CARTESIAN_POINT('',(0.473732170341016,0.999958186567598,2.25565803263806));
#25946=CARTESIAN_POINT('',(0.47355,1.,2.15));
#25947=CARTESIAN_POINT('Ctrl Pts',(0.473732170341016,0.999958186567598,
2.25565803263806));
#25948=CARTESIAN_POINT('Ctrl Pts',(0.47380378639699,1.0235579489136,2.25417789949394));
#25949=CARTESIAN_POINT('Ctrl Pts',(0.480162569358453,1.04719354904427,2.25269776634982));
#25950=CARTESIAN_POINT('Ctrl Pts',(0.492561799143745,1.06705892706426,2.25121763320569));
#25951=CARTESIAN_POINT('Ctrl Pts',(0.514483427533268,1.1021805791598,2.2486007828598));
#25952=CARTESIAN_POINT('Ctrl Pts',(0.555286068051798,1.12551740614607,2.24598393251391));
#25953=CARTESIAN_POINT('Ctrl Pts',(0.596673331802579,1.12660489722647,2.24336708216802));
#25954=CARTESIAN_POINT('Ctrl Pts',(0.63806059555336,1.12769238830687,2.24075023182212));
#25955=CARTESIAN_POINT('Ctrl Pts',(0.680032482536391,1.10653054348142,2.23813338147623));
#25956=CARTESIAN_POINT('Ctrl Pts',(0.703768299652422,1.07260858560646,2.23551653113034));
#25957=CARTESIAN_POINT('Ctrl Pts',(0.727504116768454,1.0386866277315,2.23289968078445));
#25958=CARTESIAN_POINT('Ctrl Pts',(0.733003864017485,0.992004556807043,
2.23028283043855));
#25959=CARTESIAN_POINT('Ctrl Pts',(0.717801389391014,0.953495168290641,
2.22766598009266));
#25960=CARTESIAN_POINT('Ctrl Pts',(0.702598914764542,0.914985779774238,
2.22504912974677));
#25961=CARTESIAN_POINT('Ctrl Pts',(0.666694218262566,0.884649073665893,
2.22243227940087));
#25962=CARTESIAN_POINT('Ctrl Pts',(0.626187392572728,0.876088389616529,
2.21981542905498));
#25963=CARTESIAN_POINT('Ctrl Pts',(0.58568056688289,0.867527705567165,2.21719857870909));
#25964=CARTESIAN_POINT('Ctrl Pts',(0.540571612005191,0.880743043576783,
2.2145817283632));
#25965=CARTESIAN_POINT('Ctrl Pts',(0.511087919517129,0.909808488978038,
2.21196487801731));
#25966=CARTESIAN_POINT('Ctrl Pts',(0.487401800053794,0.933158604039368,
2.20986259622422));
#25967=CARTESIAN_POINT('Ctrl Pts',(0.473800111710378,0.966738263555599,
2.20776031443114));
#25968=CARTESIAN_POINT('Ctrl Pts',(0.473504867419963,1.00010483506638,2.20565803263806));
#25969=CARTESIAN_POINT('Ctrl Pts',(0.473352235667534,0.999991049382066,
2.21934196736194));
#25970=CARTESIAN_POINT('Ctrl Pts',(0.473351711967774,0.99948814546325,2.2193737536191));
#25971=CARTESIAN_POINT('Ctrl Pts',(0.473354454431116,0.998985247411069,
2.21940553987625));
#25972=CARTESIAN_POINT('Ctrl Pts',(0.473360480544096,0.998482388709186,
2.21943732613341));
#25973=CARTESIAN_POINT('Ctrl Pts',(0.473856589153524,0.95708380687781,2.2220541764793));
#25974=CARTESIAN_POINT('Ctrl Pts',(0.496608118053516,0.915951927508368,
2.22467102682519));
#25975=CARTESIAN_POINT('Ctrl Pts',(0.531413011239654,0.893530774346426,
2.22728787717109));
#25976=CARTESIAN_POINT('Ctrl Pts',(0.566217904425792,0.871109621184485,
2.22990472751698));
#25977=CARTESIAN_POINT('Ctrl Pts',(0.613076161898077,0.867399194230046,
2.23252157786287));
#25978=CARTESIAN_POINT('Ctrl Pts',(0.650975984015301,0.88406329282086,2.23513842820876));
#25979=CARTESIAN_POINT('Ctrl Pts',(0.688875806132525,0.900727391411673,
2.23775527855466));
#25980=CARTESIAN_POINT('Ctrl Pts',(0.717817192894688,0.93776601554774,2.24037212890055));
#25981=CARTESIAN_POINT('Ctrl Pts',(0.724822482446523,0.978570606314872,
2.24298897924644));
#25982=CARTESIAN_POINT('Ctrl Pts',(0.731827771998358,1.019375197082,2.24560582959233));
#25983=CARTESIAN_POINT('Ctrl Pts',(0.716896964339864,1.0639457544802,2.24822267993823));
#25984=CARTESIAN_POINT('Ctrl Pts',(0.686725211124828,1.09229630994494,2.25083953028412));
#25985=CARTESIAN_POINT('Ctrl Pts',(0.656553457909791,1.12064686540969,2.25345638063001));
#25986=CARTESIAN_POINT('Ctrl Pts',(0.611140759138212,1.13277741894098,2.25607323097591));
#25987=CARTESIAN_POINT('Ctrl Pts',(0.570850708712658,1.12324848776292,2.2586900813218));
#25988=CARTESIAN_POINT('Ctrl Pts',(0.530560658287105,1.11371955658487,2.26130693166769));
#25989=CARTESIAN_POINT('Ctrl Pts',(0.495393256207577,1.08253114069748,2.26392378201358));
#25990=CARTESIAN_POINT('Ctrl Pts',(0.481117983672093,1.04366849332961,2.26654063235948));
#25991=CARTESIAN_POINT('Ctrl Pts',(0.476024096576591,1.02980102162761,2.26747441069363));
#25992=CARTESIAN_POINT('Ctrl Pts',(0.473590398662461,1.01495639211521,2.26840818902779));
#25993=CARTESIAN_POINT('Ctrl Pts',(0.473682079464411,1.00008273769678,2.26934196736194));
#25994=CARTESIAN_POINT('Origin',(0.6,1.,2.15));
#25995=CARTESIAN_POINT('',(0.473597863174539,0.999893075682974,2.31934196736194));
#25996=CARTESIAN_POINT('',(0.473373733146151,0.999953562449677,2.30565803263806));
#25997=CARTESIAN_POINT('',(0.47355,1.,2.15));
#25998=CARTESIAN_POINT('Ctrl Pts',(0.473373733146151,0.999953562449677,
2.30565803263806));
#25999=CARTESIAN_POINT('Ctrl Pts',(0.473559114374899,1.03866557284283,2.30321233490263));
#26000=CARTESIAN_POINT('Ctrl Pts',(0.492644288253083,1.07753593829701,2.3007666371672));
#26001=CARTESIAN_POINT('Ctrl Pts',(0.523476045360312,1.10091555973398,2.29832093943176));
#26002=CARTESIAN_POINT('Ctrl Pts',(0.556465442652399,1.12593131272659,2.29570408908587));
#26003=CARTESIAN_POINT('Ctrl Pts',(0.602903027909946,1.1332123395264,2.29308723873998));
#26004=CARTESIAN_POINT('Ctrl Pts',(0.641965643116553,1.11949373110512,2.29047038839408));
#26005=CARTESIAN_POINT('Ctrl Pts',(0.681028258323161,1.10577512268384,2.28785353804819));
#26006=CARTESIAN_POINT('Ctrl Pts',(0.712715903478828,1.07105687904148,2.2852366877023));
#26007=CARTESIAN_POINT('Ctrl Pts',(0.722819458161278,1.03090707843903,2.28261983735641));
#26008=CARTESIAN_POINT('Ctrl Pts',(0.732923012843728,0.990757277836576,
2.28000298701051));
#26009=CARTESIAN_POINT('Ctrl Pts',(0.72144247705296,0.945175920274039,2.27738613666462));
#26010=CARTESIAN_POINT('Ctrl Pts',(0.693525861372284,0.914602225692484,
2.27476928631873));
#26011=CARTESIAN_POINT('Ctrl Pts',(0.665609245691608,0.88402853111093,2.27215243597284));
#26012=CARTESIAN_POINT('Ctrl Pts',(0.621256550121025,0.868462499510358,
2.26953558562694));
#26013=CARTESIAN_POINT('Ctrl Pts',(0.580356049616192,0.874884125818288,
2.26691873528105));
#26014=CARTESIAN_POINT('Ctrl Pts',(0.539455549111359,0.881305752126219,
2.26430188493516));
#26015=CARTESIAN_POINT('Ctrl Pts',(0.502007243672275,0.909715036342652,
2.26168503458927));
#26016=CARTESIAN_POINT('Ctrl Pts',(0.484803399082991,0.947372917053277,
2.25906818424337));
#26017=CARTESIAN_POINT('Ctrl Pts',(0.477330328981013,0.963730887562828,
2.2579314670416));
#26018=CARTESIAN_POINT('Ctrl Pts',(0.473677170422209,0.981833968538321,
2.25679474983983));
#26019=CARTESIAN_POINT('Ctrl Pts',(0.473732170341016,0.999958186567598,
2.25565803263806));
#26020=CARTESIAN_POINT('Ctrl Pts',(0.473682079464411,1.00008273769678,2.26934196736194));
#26021=CARTESIAN_POINT('Ctrl Pts',(0.473847327881654,0.973273986038867,
2.27102503937368));
#26022=CARTESIAN_POINT('Ctrl Pts',(0.4822169290695,0.946370939387992,2.27270811138542));
#26023=CARTESIAN_POINT('Ctrl Pts',(0.498001477210419,0.924925552697152,
2.27439118339715));
#26024=CARTESIAN_POINT('Ctrl Pts',(0.522543386275672,0.891582138280912,
2.27700803374305));
#26025=CARTESIAN_POINT('Ctrl Pts',(0.565010347397619,0.871432188296782,
2.27962488408894));
#26026=CARTESIAN_POINT('Ctrl Pts',(0.606359670709474,0.873511167531032,
2.28224173443483));
#26027=CARTESIAN_POINT('Ctrl Pts',(0.64770899402133,0.875590146765282,2.28485858478073));
#26028=CARTESIAN_POINT('Ctrl Pts',(0.687940679523094,0.899898055217912,
2.28747543512662));
#26029=CARTESIAN_POINT('Ctrl Pts',(0.709014360624521,0.935534961978321,
2.29009228547251));
#26030=CARTESIAN_POINT('Ctrl Pts',(0.730088041725949,0.971171868738729,
2.2927091358184));
#26031=CARTESIAN_POINT('Ctrl Pts',(0.73200371842704,1.01813777380691,2.2953259861643));
#26032=CARTESIAN_POINT('Ctrl Pts',(0.713902379672349,1.05537255954882,2.29794283651019));
#26033=CARTESIAN_POINT('Ctrl Pts',(0.695801040917658,1.09260734529072,2.30055968685608));
#26034=CARTESIAN_POINT('Ctrl Pts',(0.657682686707185,1.12011101170634,2.30317653720197));
#26035=CARTESIAN_POINT('Ctrl Pts',(0.616640037917562,1.12555068124487,2.30579338754787));
#26036=CARTESIAN_POINT('Ctrl Pts',(0.57559738912794,1.1309903507834,2.30841023789376));
#26037=CARTESIAN_POINT('Ctrl Pts',(0.531630445759169,1.11436602344484,2.31102708823965));
#26038=CARTESIAN_POINT('Ctrl Pts',(0.504454512281174,1.08313206166147,2.31364393858554));
#26039=CARTESIAN_POINT('Ctrl Pts',(0.484729877635794,1.06046205898416,2.31554328151101));
#26040=CARTESIAN_POINT('Ctrl Pts',(0.473850812735054,1.03009564368688,2.31744262443648));
#26041=CARTESIAN_POINT('Ctrl Pts',(0.473597863174539,0.999893075682974,
2.31934196736194));
#26042=CARTESIAN_POINT('Origin',(0.6,1.,2.15));
#26043=CARTESIAN_POINT('',(0.473395817154925,1.00006080538999,2.36934196736194));
#26044=CARTESIAN_POINT('',(0.473630671680838,1.00010094048498,2.35565803263806));
#26045=CARTESIAN_POINT('',(0.47355,1.,2.15));
#26046=CARTESIAN_POINT('',(0.695811615272236,1.08252112989365,2.4));
#26047=CARTESIAN_POINT('Ctrl Pts',(0.473395817154925,1.00006080538999,2.36934196736194));
#26048=CARTESIAN_POINT('Ctrl Pts',(0.473632259557073,0.962556436040281,
2.37171076053695));
#26049=CARTESIAN_POINT('Ctrl Pts',(0.491389033274771,0.924867297705602,
2.37407955371196));
#26050=CARTESIAN_POINT('Ctrl Pts',(0.520582501482215,0.901356555443706,
2.37644834688697));
#26051=CARTESIAN_POINT('Ctrl Pts',(0.552833074551427,0.875383796542954,
2.37906519723286));
#26052=CARTESIAN_POINT('Ctrl Pts',(0.59904103097391,0.866714403531687,2.38168204757875));
#26053=CARTESIAN_POINT('Ctrl Pts',(0.638485120164714,0.879318631335514,
2.38429889792465));
#26054=CARTESIAN_POINT('Ctrl Pts',(0.677929209355517,0.891922859139342,
2.38691574827054));
#26055=CARTESIAN_POINT('Ctrl Pts',(0.710609431314642,0.925800707758264,
2.38953259861643));
#26056=CARTESIAN_POINT('Ctrl Pts',(0.721864159102138,0.965573527992604,
2.39214944896232));
#26057=CARTESIAN_POINT('Ctrl Pts',(0.733118886889633,1.00534634822694,2.39476629930821));
#26058=CARTESIAN_POINT('Ctrl Pts',(0.7229481205055,1.0510141400767,2.39738314965411));
#26059=CARTESIAN_POINT('Ctrl Pts',(0.695811615272236,1.08252112989365,2.4));
#26060=CARTESIAN_POINT('',(0.50401104110406,1.08263520219401,2.4));
#26061=CARTESIAN_POINT('Origin',(0.6,1.,2.4));
#26062=CARTESIAN_POINT('Ctrl Pts',(0.504010178078501,1.08263575731581,2.4));
#26063=CARTESIAN_POINT('Ctrl Pts',(0.529836321312633,1.11242104812743,2.3975091839613));
#26064=CARTESIAN_POINT('Ctrl Pts',(0.57074030629072,1.12936968375571,2.3950183679226));
#26065=CARTESIAN_POINT('Ctrl Pts',(0.610030393987409,1.12624202648756,2.3925275518839));
#26066=CARTESIAN_POINT('Ctrl Pts',(0.651308544594168,1.12295611099769,2.389910701538));
#26067=CARTESIAN_POINT('Ctrl Pts',(0.690805340696773,1.09751079590418,2.38729385119211));
#26068=CARTESIAN_POINT('Ctrl Pts',(0.710833835900798,1.0612825699207,2.38467700084622));
#26069=CARTESIAN_POINT('Ctrl Pts',(0.730862331104824,1.02505434393722,2.38206015050033));
#26070=CARTESIAN_POINT('Ctrl Pts',(0.73142252541027,0.978043207063774,2.37944330015443));
#26071=CARTESIAN_POINT('Ctrl Pts',(0.712251088485857,0.941346462423258,
2.37682644980854));
#26072=CARTESIAN_POINT('Ctrl Pts',(0.693079651561443,0.904649717782742,
2.37420959946265));
#26073=CARTESIAN_POINT('Ctrl Pts',(0.654176583407171,0.878267365375156,
2.37159274911676));
#26074=CARTESIAN_POINT('Ctrl Pts',(0.612992655582392,0.874020946237636,
2.36897589877086));
#26075=CARTESIAN_POINT('Ctrl Pts',(0.571808727757614,0.869774527100117,
2.36635904842497));
#26076=CARTESIAN_POINT('Ctrl Pts',(0.52834394026233,0.887664041232664,2.36374219807908));
#26077=CARTESIAN_POINT('Ctrl Pts',(0.502085278312862,0.919672004499943,
2.36112534773319));
#26078=CARTESIAN_POINT('Ctrl Pts',(0.483798106092066,0.941963130294246,
2.35930290936814));
#26079=CARTESIAN_POINT('Ctrl Pts',(0.473856023642611,0.971101801466951,
2.3574804710031));
#26080=CARTESIAN_POINT('Ctrl Pts',(0.473630671680838,1.00010094048498,2.35565803263806));
#26081=CARTESIAN_POINT('Origin',(-0.6,1.,2.15));
#26082=CARTESIAN_POINT('',(-0.726251764241557,0.999995816438242,2.01934196736194));
#26083=CARTESIAN_POINT('',(-0.726377624507173,0.999839605165841,2.00565803263806));
#26084=CARTESIAN_POINT('',(-0.72645,1.,2.15));
#26085=CARTESIAN_POINT('',(-0.695811615272238,1.08252112989365,2.));
#26086=CARTESIAN_POINT('Ctrl Pts',(-0.726377624507173,0.999839605165841,
2.00565803263806));
#26087=CARTESIAN_POINT('Ctrl Pts',(-0.726114592834244,1.02975025674996,
2.00377202175871));
#26088=CARTESIAN_POINT('Ctrl Pts',(-0.715369380269338,1.05981347843636,
2.00188601087935));
#26089=CARTESIAN_POINT('Ctrl Pts',(-0.695811615272238,1.08252112989365,
2.));
#26090=CARTESIAN_POINT('',(-0.504011038081522,1.08263519664064,2.));
#26091=CARTESIAN_POINT('Origin',(-0.6,1.,2.));
#26092=CARTESIAN_POINT('Ctrl Pts',(-0.504010174669748,1.08263575197435,
2.));
#26093=CARTESIAN_POINT('Ctrl Pts',(-0.529836317100857,1.11242103949754,
2.0024908160387));
#26094=CARTESIAN_POINT('Ctrl Pts',(-0.570740304630068,1.12936968846467,
2.0049816320774));
#26095=CARTESIAN_POINT('Ctrl Pts',(-0.610030394063595,1.12624203395227,
2.0074724481161));
#26096=CARTESIAN_POINT('Ctrl Pts',(-0.651308546495077,1.12295612135759,
2.010089298462));
#26097=CARTESIAN_POINT('Ctrl Pts',(-0.690805343523631,1.09751079747805,
2.01270614880789));
#26098=CARTESIAN_POINT('Ctrl Pts',(-0.710833838996196,1.06128256888394,
2.01532299915378));
#26099=CARTESIAN_POINT('Ctrl Pts',(-0.721087117546352,1.04273608746385,
2.01666265522317));
#26100=CARTESIAN_POINT('Ctrl Pts',(-0.72623820261666,1.02136365505003,2.01800231129255));
#26101=CARTESIAN_POINT('Ctrl Pts',(-0.726251764241557,0.999995816438242,
2.01934196736194));
#26102=CARTESIAN_POINT('Origin',(-0.6,1.,2.15));
#26103=CARTESIAN_POINT('',(-0.7265819818033,0.99992222657182,2.06934196736194));
#26104=CARTESIAN_POINT('',(-0.726608486751216,1.0000625869776,2.05565803263806));
#26105=CARTESIAN_POINT('',(-0.72645,1.,2.15));
#26106=CARTESIAN_POINT('Ctrl Pts',(-0.726608486751216,1.0000625869776,2.05565803263806));
#26107=CARTESIAN_POINT('Ctrl Pts',(-0.726631053637245,1.00377931196893,
2.05542330751329));
#26108=CARTESIAN_POINT('Ctrl Pts',(-0.726481239616099,1.00749417780353,
2.05518858238852));
#26109=CARTESIAN_POINT('Ctrl Pts',(-0.726153054400444,1.01119320003794,
2.05495385726375));
#26110=CARTESIAN_POINT('Ctrl Pts',(-0.722494257346049,1.0524320219281,2.05233700691785));
#26111=CARTESIAN_POINT('Ctrl Pts',(-0.696665580577272,1.09170163174089,
2.04972015657196));
#26112=CARTESIAN_POINT('Ctrl Pts',(-0.660248783717448,1.1113984599152,2.04710330622607));
#26113=CARTESIAN_POINT('Ctrl Pts',(-0.623831986857623,1.13109528808951,
2.04448645588018));
#26114=CARTESIAN_POINT('Ctrl Pts',(-0.576827069906751,1.13121933462535,
2.04186960553428));
#26115=CARTESIAN_POINT('Ctrl Pts',(-0.540311843519016,1.11170438339395,
2.03925275518839));
#26116=CARTESIAN_POINT('Ctrl Pts',(-0.503796617131281,1.09218943216256,
2.0366359048425));
#26117=CARTESIAN_POINT('Ctrl Pts',(-0.477771081306684,1.05303548316395,
2.03401905449661));
#26118=CARTESIAN_POINT('Ctrl Pts',(-0.473904915961309,1.01182046061616,
2.03140220415071));
#26119=CARTESIAN_POINT('Ctrl Pts',(-0.470038750615934,0.970605438068375,
2.02878535380482));
#26120=CARTESIAN_POINT('Ctrl Pts',(-0.48833195574978,0.927329341971419,
2.02616850345893));
#26121=CARTESIAN_POINT('Ctrl Pts',(-0.520582517234745,0.901356578046236,
2.02355165311303));
#26122=CARTESIAN_POINT('Ctrl Pts',(-0.55283307871971,0.875383814121054,
2.02093480276714));
#26123=CARTESIAN_POINT('Ctrl Pts',(-0.599040996555793,0.866714382367644,
2.01831795242125));
#26124=CARTESIAN_POINT('Ctrl Pts',(-0.63848510046728,0.879318623815634,
2.01570110207536));
#26125=CARTESIAN_POINT('Ctrl Pts',(-0.677929204378768,0.891922865263625,
2.01308425172946));
#26126=CARTESIAN_POINT('Ctrl Pts',(-0.710609494365659,0.925800779913016,
2.01046740138357));
#26127=CARTESIAN_POINT('Ctrl Pts',(-0.721864223397342,0.965573598616285,
2.00785055103768));
#26128=CARTESIAN_POINT('Ctrl Pts',(-0.725007467784426,0.976681435046254,
2.00711971157114));
#26129=CARTESIAN_POINT('Ctrl Pts',(-0.726479550710055,0.988249065107503,
2.0063888721046));
#26130=CARTESIAN_POINT('Ctrl Pts',(-0.726377624507173,0.999839605165841,
2.00565803263806));
#26131=CARTESIAN_POINT('Ctrl Pts',(-0.726251764241557,0.999995816438242,
2.01934196736194));
#26132=CARTESIAN_POINT('Ctrl Pts',(-0.726264693552367,0.979624258543708,
2.02061916163845));
#26133=CARTESIAN_POINT('Ctrl Pts',(-0.721608007468156,0.959256876063438,
2.02189635591495));
#26134=CARTESIAN_POINT('Ctrl Pts',(-0.712251090996448,0.941346462433457,
2.02317355019146));
#26135=CARTESIAN_POINT('Ctrl Pts',(-0.693079653607559,0.904649717885772,
2.02579040053735));
#26136=CARTESIAN_POINT('Ctrl Pts',(-0.654176584913204,0.878267362099087,
2.02840725088324));
#26137=CARTESIAN_POINT('Ctrl Pts',(-0.612992656110291,0.874020942267452,
2.03102410122914));
#26138=CARTESIAN_POINT('Ctrl Pts',(-0.571808727307379,0.869774522435818,
2.03364095157503));
#26139=CARTESIAN_POINT('Ctrl Pts',(-0.528343938395909,0.887664038559235,
2.03625780192092));
#26140=CARTESIAN_POINT('Ctrl Pts',(-0.502085275739541,0.919672002962672,
2.03887465226682));
#26141=CARTESIAN_POINT('Ctrl Pts',(-0.475826613083173,0.951679967366109,
2.04149150261271));
#26142=CARTESIAN_POINT('Ctrl Pts',(-0.466774076681907,0.997806380049565,
2.0441083529586));
#26143=CARTESIAN_POINT('Ctrl Pts',(-0.478988530498336,1.03736537794115,
2.04672520330449));
#26144=CARTESIAN_POINT('Ctrl Pts',(-0.491202984314765,1.07692437583273,
2.04934205365039));
#26145=CARTESIAN_POINT('Ctrl Pts',(-0.52468442834889,1.10991595893243,2.05195890399628));
#26146=CARTESIAN_POINT('Ctrl Pts',(-0.564418571222927,1.12154744492272,
2.05457575434217));
#26147=CARTESIAN_POINT('Ctrl Pts',(-0.604152714096964,1.13317893091301,
2.05719260468806));
#26148=CARTESIAN_POINT('Ctrl Pts',(-0.650139555810913,1.12345031979389,
2.05980945503396));
#26149=CARTESIAN_POINT('Ctrl Pts',(-0.681758464159146,1.09672345837341,
2.06242630537985));
#26150=CARTESIAN_POINT('Ctrl Pts',(-0.709612009894941,1.07317938630266,
2.06473152604055));
#26151=CARTESIAN_POINT('Ctrl Pts',(-0.726315897827418,1.03644450458023,
2.06703674670125));
#26152=CARTESIAN_POINT('Ctrl Pts',(-0.7265819818033,0.99992222657182,2.06934196736194));
#26153=CARTESIAN_POINT('Origin',(-0.6,1.,2.15));
#26154=CARTESIAN_POINT('',(-0.726430664085926,1.00010891291408,2.11934196736194));
#26155=CARTESIAN_POINT('',(-0.726259449807842,1.00002674766465,2.10565803263806));
#26156=CARTESIAN_POINT('',(-0.72645,1.,2.15));
#26157=CARTESIAN_POINT('Ctrl Pts',(-0.726259449807842,1.00002674766465,
2.10565803263806));
#26158=CARTESIAN_POINT('Ctrl Pts',(-0.726296436394794,1.01916777993272,
2.10445774292198));
#26159=CARTESIAN_POINT('Ctrl Pts',(-0.722205040678573,1.0382938070189,2.1032574532059));
#26160=CARTESIAN_POINT('Ctrl Pts',(-0.713902369187372,1.05537255449598,
2.10205716348981));
#26161=CARTESIAN_POINT('Ctrl Pts',(-0.695801032091435,1.09260733676896,
2.09944031314392));
#26162=CARTESIAN_POINT('Ctrl Pts',(-0.657682681356665,1.12011100048129,
2.09682346279803));
#26163=CARTESIAN_POINT('Ctrl Pts',(-0.616640036366223,1.12555066958795,
2.09420661245214));
#26164=CARTESIAN_POINT('Ctrl Pts',(-0.57559739137578,1.13099033869461,2.09158976210624));
#26165=CARTESIAN_POINT('Ctrl Pts',(-0.531630452129665,1.1143660131956,2.08897291176035));
#26166=CARTESIAN_POINT('Ctrl Pts',(-0.504454521120231,1.08313205416568,
2.08635606141446));
#26167=CARTESIAN_POINT('Ctrl Pts',(-0.477278590110797,1.05189809513576,
2.08373921106857));
#26168=CARTESIAN_POINT('Ctrl Pts',(-0.466893667338043,1.00605450257494,
2.08112236072267));
#26169=CARTESIAN_POINT('Ctrl Pts',(-0.477956467154043,0.966158450016923,
2.07850551037678));
#26170=CARTESIAN_POINT('Ctrl Pts',(-0.489019266970043,0.926262397458909,
2.07588866003089));
#26171=CARTESIAN_POINT('Ctrl Pts',(-0.521529789374798,0.892313884903708,
2.07327180968499));
#26172=CARTESIAN_POINT('Ctrl Pts',(-0.560909946303062,0.879535118270141,
2.0706549593391));
#26173=CARTESIAN_POINT('Ctrl Pts',(-0.600290103231324,0.866756351636574,
2.06803810899321));
#26174=CARTESIAN_POINT('Ctrl Pts',(-0.646539894683095,0.875147330924641,
2.06542125864732));
#26175=CARTESIAN_POINT('Ctrl Pts',(-0.678920331738974,0.900946837552442,
2.06280440830142));
#26176=CARTESIAN_POINT('Ctrl Pts',(-0.708396322180238,0.924432191052708,
2.0604222830803));
#26177=CARTESIAN_POINT('Ctrl Pts',(-0.726379465045821,0.962343129588992,
2.05804015785918));
#26178=CARTESIAN_POINT('Ctrl Pts',(-0.726608486751216,1.0000625869776,2.05565803263806));
#26179=CARTESIAN_POINT('Ctrl Pts',(-0.7265819818033,0.99992222657182,2.06934196736194));
#26180=CARTESIAN_POINT('Ctrl Pts',(-0.726617952184381,0.99498498729039,
2.06965359704714));
#26181=CARTESIAN_POINT('Ctrl Pts',(-0.726353524983949,0.990051633299336,
2.06996522673233));
#26182=CARTESIAN_POINT('Ctrl Pts',(-0.725775636014574,0.985155277281126,
2.07027685641753));
#26183=CARTESIAN_POINT('Ctrl Pts',(-0.720922924539255,0.944039069331128,
2.07289370676342));
#26184=CARTESIAN_POINT('Ctrl Pts',(-0.693966526606102,0.905531765152948,
2.07551055710931));
#26185=CARTESIAN_POINT('Ctrl Pts',(-0.656994118794319,0.886900347913169,
2.0781274074552));
#26186=CARTESIAN_POINT('Ctrl Pts',(-0.620021710982536,0.868268930673389,
2.0807442578011));
#26187=CARTESIAN_POINT('Ctrl Pts',(-0.573033293292122,0.86951340037201,
2.08336110814699));
#26188=CARTESIAN_POINT('Ctrl Pts',(-0.537098976133817,0.890075798227289,
2.08597795849288));
#26189=CARTESIAN_POINT('Ctrl Pts',(-0.501164658975514,0.910638196082568,
2.08859480883878));
#26190=CARTESIAN_POINT('Ctrl Pts',(-0.476284442349319,0.950518522094504,
2.09121165918467));
#26191=CARTESIAN_POINT('Ctrl Pts',(-0.473614938940181,0.991833925232179,
2.09382850953056));
#26192=CARTESIAN_POINT('Ctrl Pts',(-0.470945435531044,1.03314932836985,
2.09644535987645));
#26193=CARTESIAN_POINT('Ctrl Pts',(-0.490486645338963,1.07589980863327,
2.09906221022235));
#26194=CARTESIAN_POINT('Ctrl Pts',(-0.523476043451828,1.10091556225217,
2.10167906056824));
#26195=CARTESIAN_POINT('Ctrl Pts',(-0.556465441564692,1.12593131587107,
2.10429591091413));
#26196=CARTESIAN_POINT('Ctrl Pts',(-0.6029030279825,1.13321234284545,2.10691276126002));
#26197=CARTESIAN_POINT('Ctrl Pts',(-0.64196564416317,1.11949373408075,2.10952961160592));
#26198=CARTESIAN_POINT('Ctrl Pts',(-0.68102826034384,1.10577512531604,2.11214646195181));
#26199=CARTESIAN_POINT('Ctrl Pts',(-0.712715906287371,1.07105688081224,
2.1147633122977));
#26200=CARTESIAN_POINT('Ctrl Pts',(-0.722819461221189,1.03090707921019,
2.1173801626436));
#26201=CARTESIAN_POINT('Ctrl Pts',(-0.725344277841846,1.02087388920281,
2.11803409754971));
#26202=CARTESIAN_POINT('Ctrl Pts',(-0.72652123370157,1.01050151499351,2.11868803245583));
#26203=CARTESIAN_POINT('Ctrl Pts',(-0.726430664085926,1.00010891291408,
2.11934196736194));
#26204=CARTESIAN_POINT('Origin',(-0.6,1.,2.15));
#26205=CARTESIAN_POINT('',(-0.726298666832045,0.999928563942421,2.16934196736194));
#26206=CARTESIAN_POINT('',(-0.72652403561687,0.999901036843312,2.15565803263806));
#26207=CARTESIAN_POINT('',(-0.72645,1.,2.15));
#26208=CARTESIAN_POINT('Ctrl Pts',(-0.72652403561687,0.999901036843312,
2.15565803263806));
#26209=CARTESIAN_POINT('Ctrl Pts',(-0.726228629089082,1.03425627916229,
2.15349217833067));
#26210=CARTESIAN_POINT('Ctrl Pts',(-0.711697061286474,1.06883177008057,
2.15132632402327));
#26211=CARTESIAN_POINT('Ctrl Pts',(-0.686725203134716,1.09229630144258,
2.14916046971588));
#26212=CARTESIAN_POINT('Ctrl Pts',(-0.65655345269935,1.12064685429431,2.14654361936999));
#26213=CARTESIAN_POINT('Ctrl Pts',(-0.611140758111187,1.13277740670372,
2.1439267690241));
#26214=CARTESIAN_POINT('Ctrl Pts',(-0.570850711397976,1.12324847640543,
2.1413099186782));
#26215=CARTESIAN_POINT('Ctrl Pts',(-0.530560664684765,1.11371954610715,
2.13869306833231));
#26216=CARTESIAN_POINT('Ctrl Pts',(-0.495393265846508,1.08253113310118,
2.13607621798642));
#26217=CARTESIAN_POINT('Ctrl Pts',(-0.481117994625666,1.04366848931044,
2.13345936764053));
#26218=CARTESIAN_POINT('Ctrl Pts',(-0.466842723404823,1.00480584551971,
2.13084251729463));
#26219=CARTESIAN_POINT('Ctrl Pts',(-0.473459579801396,0.958268970944215,
2.12822566694874));
#26220=CARTESIAN_POINT('Ctrl Pts',(-0.498001486606679,0.924925559606287,
2.12560881660285));
#26221=CARTESIAN_POINT('Ctrl Pts',(-0.522543393411961,0.89158214826836,
2.12299196625695));
#26222=CARTESIAN_POINT('Ctrl Pts',(-0.565010350625955,0.871432200167998,
2.12037511591106));
#26223=CARTESIAN_POINT('Ctrl Pts',(-0.606359670125879,0.873511179199166,
2.11775826556517));
#26224=CARTESIAN_POINT('Ctrl Pts',(-0.647708989625804,0.875590158230334,
2.11514141521928));
#26225=CARTESIAN_POINT('Ctrl Pts',(-0.687940671411661,0.899898064393031,
2.11252456487338));
#26226=CARTESIAN_POINT('Ctrl Pts',(-0.709014350576037,0.935534967891196,
2.10990771452749));
#26227=CARTESIAN_POINT('Ctrl Pts',(-0.72042201256801,0.954826034551965,
2.10849115389768));
#26228=CARTESIAN_POINT('Ctrl Pts',(-0.726215798894061,0.977436840943303,
2.10707459326787));
#26229=CARTESIAN_POINT('Ctrl Pts',(-0.726259449807842,1.00002674766465,
2.10565803263806));
#26230=CARTESIAN_POINT('Ctrl Pts',(-0.726430664085926,1.00010891291408,
2.11934196736194));
#26231=CARTESIAN_POINT('Ctrl Pts',(-0.726158801404701,0.968913454634673,
2.12130488280172));
#26232=CARTESIAN_POINT('Ctrl Pts',(-0.714466288285182,0.937535739321086,
2.1232677982415));
#26233=CARTESIAN_POINT('Ctrl Pts',(-0.693525863703029,0.914602223563998,
2.12523071368127));
#26234=CARTESIAN_POINT('Ctrl Pts',(-0.665609247326942,0.884028528220152,
2.12784756402716));
#26235=CARTESIAN_POINT('Ctrl Pts',(-0.621256550650662,0.868462496232756,
2.13046441437306));
#26236=CARTESIAN_POINT('Ctrl Pts',(-0.580356049126553,0.874884122700947,
2.13308126471895));
#26237=CARTESIAN_POINT('Ctrl Pts',(-0.539455547602445,0.881305749169137,
2.13569811506484));
#26238=CARTESIAN_POINT('Ctrl Pts',(-0.502007241230509,0.909715034092914,
2.13831496541074));
#26239=CARTESIAN_POINT('Ctrl Pts',(-0.484803396212605,0.947372915741768,
2.14093181575663));
#26240=CARTESIAN_POINT('Ctrl Pts',(-0.467599551194702,0.985030797390621,
2.14354866610252));
#26241=CARTESIAN_POINT('Ctrl Pts',(-0.470640167530832,1.03193727576455,
2.14616551644841));
#26242=CARTESIAN_POINT('Ctrl Pts',(-0.492561796466562,1.06705892873532,
2.14878236679431));
#26243=CARTESIAN_POINT('Ctrl Pts',(-0.514483425402293,1.10218058170609,
2.1513992171402));
#26244=CARTESIAN_POINT('Ctrl Pts',(-0.555286066937625,1.1255174092737,2.15401606748609));
#26245=CARTESIAN_POINT('Ctrl Pts',(-0.596673331719711,1.12660490038116,
2.15663291783198));
#26246=CARTESIAN_POINT('Ctrl Pts',(-0.638060596501796,1.12769239148863,
2.15924976817788));
#26247=CARTESIAN_POINT('Ctrl Pts',(-0.680032484530636,1.10653054613594,
2.16186661852377));
#26248=CARTESIAN_POINT('Ctrl Pts',(-0.703768302238105,1.07260858741574,
2.16448346886966));
#26249=CARTESIAN_POINT('Ctrl Pts',(-0.718457772313683,1.05161518395829,
2.16610296836709));
#26250=CARTESIAN_POINT('Ctrl Pts',(-0.726162745631061,1.02573459982654,
2.16772246786452));
#26251=CARTESIAN_POINT('Ctrl Pts',(-0.726298666832045,0.999928563942421,
2.16934196736194));
#26252=CARTESIAN_POINT('Origin',(-0.6,1.,2.15));
#26253=CARTESIAN_POINT('',(-0.726647750450984,0.999991049383163,2.21934196736194));
#26254=CARTESIAN_POINT('',(-0.726495137942383,1.00010483507083,2.20565803263806));
#26255=CARTESIAN_POINT('',(-0.72645,1.,2.15));
#26256=CARTESIAN_POINT('Ctrl Pts',(-0.726495137942383,1.00010483507083,
2.20565803263806));
#26257=CARTESIAN_POINT('Ctrl Pts',(-0.726567403912713,1.00827186063272,
2.20514346408525));
#26258=CARTESIAN_POINT('Ctrl Pts',(-0.725842471048314,1.01642611993573,
2.20462889553244));
#26259=CARTESIAN_POINT('Ctrl Pts',(-0.72427309126162,1.02441448062962,2.20411432697963));
#26260=CARTESIAN_POINT('Ctrl Pts',(-0.716291973847398,1.06503947477424,
2.20149747663373));
#26261=CARTESIAN_POINT('Ctrl Pts',(-0.686471308333041,1.10137390836652,
2.19888062628784));
#26262=CARTESIAN_POINT('Ctrl Pts',(-0.648183035606218,1.11712498946538,
2.19626377594195));
#26263=CARTESIAN_POINT('Ctrl Pts',(-0.609894762879395,1.13287607056424,
2.19364692559606));
#26264=CARTESIAN_POINT('Ctrl Pts',(-0.563138882940105,1.12804379916968,
2.19103007525017));
#26265=CARTESIAN_POINT('Ctrl Pts',(-0.52888128813228,1.10479502324521,2.18841322490427));
#26266=CARTESIAN_POINT('Ctrl Pts',(-0.494623693324455,1.08154624732075,
2.18579637455838));
#26267=CARTESIAN_POINT('Ctrl Pts',(-0.472864383648094,1.03988096686638,
2.18317952421249));
#26268=CARTESIAN_POINT('Ctrl Pts',(-0.473360492211805,0.998482388849106,
2.18056267386659));
#26269=CARTESIAN_POINT('Ctrl Pts',(-0.473856600775515,0.957083810831832,
2.1779458235207));
#26270=CARTESIAN_POINT('Ctrl Pts',(-0.496608127579297,0.915951935251654,
2.17532897317481));
#26271=CARTESIAN_POINT('Ctrl Pts',(-0.531413017558768,0.893530784155595,
2.17271212282892));
#26272=CARTESIAN_POINT('Ctrl Pts',(-0.56621790753824,0.871109633059536,
2.17009527248302));
#26273=CARTESIAN_POINT('Ctrl Pts',(-0.613076160693402,0.867399206447596,
2.16747842213713));
#26274=CARTESIAN_POINT('Ctrl Pts',(-0.650975979318758,0.884063303502809,
2.16486157179124));
#26275=CARTESIAN_POINT('Ctrl Pts',(-0.688875797944115,0.900727400558021,
2.16224472144534));
#26276=CARTESIAN_POINT('Ctrl Pts',(-0.717817182039666,0.937766021280388,
2.15962787109945));
#26277=CARTESIAN_POINT('Ctrl Pts',(-0.724822470946157,0.978570608288594,
2.15701102075356));
#26278=CARTESIAN_POINT('Ctrl Pts',(-0.726029783985795,0.985602996335628,
2.15656002471506));
#26279=CARTESIAN_POINT('Ctrl Pts',(-0.726585548144894,0.9927472416251,2.15610902867656));
#26280=CARTESIAN_POINT('Ctrl Pts',(-0.72652403561687,0.999901036843312,
2.15565803263806));
#26281=CARTESIAN_POINT('Ctrl Pts',(-0.726298666832045,0.999928563942421,
2.16934196736194));
#26282=CARTESIAN_POINT('Ctrl Pts',(-0.726382372399933,0.984036202243351,
2.17033931821041));
#26283=CARTESIAN_POINT('Ctrl Pts',(-0.723595457458582,0.968172113533461,
2.17133666905888));
#26284=CARTESIAN_POINT('Ctrl Pts',(-0.71780139232639,0.95349516713182,2.17233401990734));
#26285=CARTESIAN_POINT('Ctrl Pts',(-0.702598917321108,0.914985777655832,
2.17495087025323));
#26286=CARTESIAN_POINT('Ctrl Pts',(-0.666694219924447,0.884649070791584,
2.17756772059913));
#26287=CARTESIAN_POINT('Ctrl Pts',(-0.626187393225259,0.876088386528911,
2.18018457094502));
#26288=CARTESIAN_POINT('Ctrl Pts',(-0.58568056652607,0.867527702266238,
2.18280142129091));
#26289=CARTESIAN_POINT('Ctrl Pts',(-0.540571610524354,0.880743040605142,
2.1854182716368));
#26290=CARTESIAN_POINT('Ctrl Pts',(-0.511087917301621,0.909808486730647,
2.1880351219827));
#26291=CARTESIAN_POINT('Ctrl Pts',(-0.481604224078888,0.938873932856152,
2.19065197232859));
#26292=CARTESIAN_POINT('Ctrl Pts',(-0.467745793635136,0.983789486768259,
2.19326882267448));
#26293=CARTESIAN_POINT('Ctrl Pts',(-0.475726910909899,1.02441448020301,
2.19588567302037));
#26294=CARTESIAN_POINT('Ctrl Pts',(-0.483708028184661,1.06503947363776,
2.19850252336627));
#26295=CARTESIAN_POINT('Ctrl Pts',(-0.513528693177939,1.10137390659515,
2.20111937371216));
#26296=CARTESIAN_POINT('Ctrl Pts',(-0.551816965235723,1.11712498741877,
2.20373622405805));
#26297=CARTESIAN_POINT('Ctrl Pts',(-0.590105237293507,1.1328760682424,2.20635307440395));
#26298=CARTESIAN_POINT('Ctrl Pts',(-0.636861116415798,1.12804379693225,
2.20896992474984));
#26299=CARTESIAN_POINT('Ctrl Pts',(-0.671118710625013,1.10479502141404,
2.21158677509573));
#26300=CARTESIAN_POINT('Ctrl Pts',(-0.704960186006201,1.0818286432283,2.21417183918447));
#26301=CARTESIAN_POINT('Ctrl Pts',(-0.726605159802828,1.04089044536347,
2.21675690327321));
#26302=CARTESIAN_POINT('Ctrl Pts',(-0.726647750450984,0.999991049383163,
2.21934196736194));
#26303=CARTESIAN_POINT('Origin',(-0.6,1.,2.15));
#26304=CARTESIAN_POINT('',(-0.726317906690824,1.0000827376849,2.26934196736194));
#26305=CARTESIAN_POINT('',(-0.726267835011577,0.999958186565595,2.25565803263806));
#26306=CARTESIAN_POINT('',(-0.72645,1.,2.15));
#26307=CARTESIAN_POINT('Ctrl Pts',(-0.726267835011577,0.999958186565595,
2.25565803263806));
#26308=CARTESIAN_POINT('Ctrl Pts',(-0.726196218952626,1.02355794991214,
2.25417789949394));
#26309=CARTESIAN_POINT('Ctrl Pts',(-0.719837435721701,1.04719355104496,
2.25269776634982));
#26310=CARTESIAN_POINT('Ctrl Pts',(-0.707438205410818,1.06705892990714,
2.25121763320569));
#26311=CARTESIAN_POINT('Ctrl Pts',(-0.685516576092059,1.10218058349167,
2.2486007828598));
#26312=CARTESIAN_POINT('Ctrl Pts',(-0.644713933843695,1.12551741146695,
2.24598393251391));
#26313=CARTESIAN_POINT('Ctrl Pts',(-0.603326668338405,1.12660490259339,
2.24336708216802));
#26314=CARTESIAN_POINT('Ctrl Pts',(-0.561939402833115,1.12769239371984,
2.24075023182213));
#26315=CARTESIAN_POINT('Ctrl Pts',(-0.519967514070899,1.10653054799744,
2.23813338147623));
#26316=CARTESIAN_POINT('Ctrl Pts',(-0.496231695948683,1.0726085886845,2.23551653113034));
#26317=CARTESIAN_POINT('Ctrl Pts',(-0.472495877826467,1.03868662937157,
2.23289968078445));
#26318=CARTESIAN_POINT('Ctrl Pts',(-0.466996130344251,0.992004556468098,
2.23028283043855));
#26319=CARTESIAN_POINT('Ctrl Pts',(-0.482198605615172,0.9534951663192,2.22766598009266));
#26320=CARTESIAN_POINT('Ctrl Pts',(-0.497401080886093,0.914985776170301,
2.22504912974677));
#26321=CARTESIAN_POINT('Ctrl Pts',(-0.533305778910153,0.884649068775973,
2.22243227940087));
#26322=CARTESIAN_POINT('Ctrl Pts',(-0.573812606317149,0.876088384363716,
2.21981542905498));
#26323=CARTESIAN_POINT('Ctrl Pts',(-0.614319433724146,0.867527699951458,
2.21719857870909));
#26324=CARTESIAN_POINT('Ctrl Pts',(-0.659428390514079,0.88074303852127,
2.2145817283632));
#26325=CARTESIAN_POINT('Ctrl Pts',(-0.688912084252003,0.909808485154657,
2.21196487801731));
#26326=CARTESIAN_POINT('Ctrl Pts',(-0.712598204719431,0.933158601205837,
2.20986259622422));
#26327=CARTESIAN_POINT('Ctrl Pts',(-0.72619989363945,0.96673826214558,2.20776031443114));
#26328=CARTESIAN_POINT('Ctrl Pts',(-0.726495137942383,1.00010483507083,
2.20565803263806));
#26329=CARTESIAN_POINT('Ctrl Pts',(-0.726647750450984,0.999991049383163,
2.21934196736194));
#26330=CARTESIAN_POINT('Ctrl Pts',(-0.726648274150687,0.999488145519468,
2.2193737536191));
#26331=CARTESIAN_POINT('Ctrl Pts',(-0.726645531687645,0.998985247522407,
2.21940553987625));
#26332=CARTESIAN_POINT('Ctrl Pts',(-0.726639505575326,0.99848238887564,
2.21943732613341));
#26333=CARTESIAN_POINT('Ctrl Pts',(-0.726143397020285,0.957083811581739,
2.2220541764793));
#26334=CARTESIAN_POINT('Ctrl Pts',(-0.703391870614066,0.915951936720223,
2.22467102682519));
#26335=CARTESIAN_POINT('Ctrl Pts',(-0.668586981242762,0.893530786015975,
2.22728787717108));
#26336=CARTESIAN_POINT('Ctrl Pts',(-0.633782091871458,0.871109635311727,
2.22990472751698));
#26337=CARTESIAN_POINT('Ctrl Pts',(-0.586923839535069,0.867399208764748,
2.23252157786287));
#26338=CARTESIAN_POINT('Ctrl Pts',(-0.549024021571972,0.884063305528724,
2.23513842820877));
#26339=CARTESIAN_POINT('Ctrl Pts',(-0.511124203608875,0.9007274022927,2.23775527855466));
#26340=CARTESIAN_POINT('Ctrl Pts',(-0.48218282001907,0.93776602236763,2.24037212890055));
#26341=CARTESIAN_POINT('Ctrl Pts',(-0.475177531234974,0.978570608662929,
2.24298897924644));
#26342=CARTESIAN_POINT('Ctrl Pts',(-0.468172242450878,1.01937519495823,
2.24560582959233));
#26343=CARTESIAN_POINT('Ctrl Pts',(-0.483103048472492,1.06394574747389,
2.24822267993823));
#26344=CARTESIAN_POINT('Ctrl Pts',(-0.513274798380673,1.09229629983004,
2.25083953028412));
#26345=CARTESIAN_POINT('Ctrl Pts',(-0.543446548288854,1.12064685218619,
2.25345638063001));
#26346=CARTESIAN_POINT('Ctrl Pts',(-0.588859242083601,1.13277740438282,
2.25607323097591));
#26347=CARTESIAN_POINT('Ctrl Pts',(-0.629149288092737,1.1232484742514,2.2586900813218));
#26348=CARTESIAN_POINT('Ctrl Pts',(-0.669439334101873,1.11371954411997,
2.26130693166769));
#26349=CARTESIAN_POINT('Ctrl Pts',(-0.704606732325397,1.08253113166048,
2.26392378201358));
#26350=CARTESIAN_POINT('Ctrl Pts',(-0.718882003296907,1.04366848854818,
2.26654063235948));
#26351=CARTESIAN_POINT('Ctrl Pts',(-0.723975889834331,1.0298010183647,2.26747441069363));
#26352=CARTESIAN_POINT('Ctrl Pts',(-0.726409587482227,1.01495639047621,
2.26840818902779));
#26353=CARTESIAN_POINT('Ctrl Pts',(-0.726317906690824,1.0000827376849,2.26934196736194));
#26354=CARTESIAN_POINT('Origin',(-0.6,1.,2.15));
#26355=CARTESIAN_POINT('',(-0.72640212307541,0.999893075304641,2.31934196736194));
#26356=CARTESIAN_POINT('',(-0.726626272216059,0.999953562434948,2.30565803263806));
#26357=CARTESIAN_POINT('',(-0.72645,1.,2.15));
#26358=CARTESIAN_POINT('Ctrl Pts',(-0.726626272216059,0.999953562434948,
2.30565803263806));
#26359=CARTESIAN_POINT('Ctrl Pts',(-0.726440890977488,1.03866557446413,
2.30321233490263));
#26360=CARTESIAN_POINT('Ctrl Pts',(-0.707355716298753,1.0775359415853,2.3007666371672));
#26361=CARTESIAN_POINT('Ctrl Pts',(-0.676523957886503,1.10091556401805,
2.29832093943176));
#26362=CARTESIAN_POINT('Ctrl Pts',(-0.643534559198068,1.12593131807613,
2.29570408908587));
#26363=CARTESIAN_POINT('Ctrl Pts',(-0.597096971966626,1.13321234517294,
2.29308723873998));
#26364=CARTESIAN_POINT('Ctrl Pts',(-0.558034355102894,1.11949373616741,
2.29047038839408));
#26365=CARTESIAN_POINT('Ctrl Pts',(-0.518971738239162,1.10577512716188,
2.28785353804819));
#26366=CARTESIAN_POINT('Ctrl Pts',(-0.487284091743139,1.07105688205399,
2.2852366877023));
#26367=CARTESIAN_POINT('Ctrl Pts',(-0.477180536633045,1.03090707975097,
2.28261983735641));
#26368=CARTESIAN_POINT('Ctrl Pts',(-0.467076981522952,0.990757277447954,
2.28000298701051));
#26369=CARTESIAN_POINT('Ctrl Pts',(-0.478557517798788,0.945175917949804,
2.27738613666462));
#26370=CARTESIAN_POINT('Ctrl Pts',(-0.506474134662531,0.914602222071399,
2.27476928631873));
#26371=CARTESIAN_POINT('Ctrl Pts',(-0.534390751526274,0.884028526192994,
2.27215243597283));
#26372=CARTESIAN_POINT('Ctrl Pts',(-0.578743448977924,0.868462493934334,
2.26953558562694));
#26373=CARTESIAN_POINT('Ctrl Pts',(-0.6196439512168,0.874884120514905,2.26691873528105));
#26374=CARTESIAN_POINT('Ctrl Pts',(-0.660544453455676,0.881305747095476,
2.26430188493516));
#26375=CARTESIAN_POINT('Ctrl Pts',(-0.697992760481779,0.909715032515278,
2.26168503458927));
#26376=CARTESIAN_POINT('Ctrl Pts',(-0.715196605800255,0.947372914822063,
2.25906818424337));
#26377=CARTESIAN_POINT('Ctrl Pts',(-0.722669676218981,0.96373088602496,
2.2579314670416));
#26378=CARTESIAN_POINT('Ctrl Pts',(-0.72632283493267,0.981833967767914,
2.25679474983983));
#26379=CARTESIAN_POINT('Ctrl Pts',(-0.726267835011577,0.999958186565595,
2.25565803263806));
#26380=CARTESIAN_POINT('Ctrl Pts',(-0.726317906690824,1.0000827376849,2.26934196736194));
#26381=CARTESIAN_POINT('Ctrl Pts',(-0.726152658292592,0.973273988959771,
2.27102503937368));
#26382=CARTESIAN_POINT('Ctrl Pts',(-0.717783058022956,0.946370945252116,
2.27270811138542));
#26383=CARTESIAN_POINT('Ctrl Pts',(-0.701998511611248,0.924925560916646,
2.27439118339715));
#26384=CARTESIAN_POINT('Ctrl Pts',(-0.677456605234583,0.891582150162549,
2.27700803374305));
#26385=CARTESIAN_POINT('Ctrl Pts',(-0.634989648761757,0.871432202419483,
2.27962488408894));
#26386=CARTESIAN_POINT('Ctrl Pts',(-0.593640329984797,0.873511181412128,
2.28224173443483));
#26387=CARTESIAN_POINT('Ctrl Pts',(-0.552291011207836,0.875590160404774,
2.28485858478073));
#26388=CARTESIAN_POINT('Ctrl Pts',(-0.512059330126741,0.899898066133132,
2.28747543512662));
#26389=CARTESIAN_POINT('Ctrl Pts',(-0.490985651329738,0.935534969012601,
2.29009228547251));
#26390=CARTESIAN_POINT('Ctrl Pts',(-0.469911972532735,0.971171871892071,
2.2927091358184));
#26391=CARTESIAN_POINT('Ctrl Pts',(-0.467996296019824,1.01813777192265,
2.29532598616429));
#26392=CARTESIAN_POINT('Ctrl Pts',(-0.486097632801175,1.0553725535377,2.29794283651019));
#26393=CARTESIAN_POINT('Ctrl Pts',(-0.504198969582526,1.09260733515275,
2.30055968685608));
#26394=CARTESIAN_POINT('Ctrl Pts',(-0.54231731965814,1.12011099835227,2.30317653720197));
#26395=CARTESIAN_POINT('Ctrl Pts',(-0.583359963928024,1.12555066737707,
2.30579338754787));
#26396=CARTESIAN_POINT('Ctrl Pts',(-0.624402608197908,1.13099033640186,
2.30841023789376));
#26397=CARTESIAN_POINT('Ctrl Pts',(-0.668369546662063,1.11436601125193,
2.31102708823965));
#26398=CARTESIAN_POINT('Ctrl Pts',(-0.695545477203344,1.08313205274415,
2.31364393858554));
#26399=CARTESIAN_POINT('Ctrl Pts',(-0.71527010971722,1.0604620524443,2.31554328151101));
#26400=CARTESIAN_POINT('Ctrl Pts',(-0.726149173523156,1.0300956400971,2.31744262443648));
#26401=CARTESIAN_POINT('Ctrl Pts',(-0.72640212307541,0.999893075304641,
2.31934196736194));
#26402=CARTESIAN_POINT('Origin',(-0.6,1.,2.15));
#26403=CARTESIAN_POINT('',(-0.726604172280256,1.00006079745576,2.36934196736194));
#26404=CARTESIAN_POINT('',(-0.726369333664333,1.00010094057762,2.35565803263806));
#26405=CARTESIAN_POINT('',(-0.72645,1.,2.15));
#26406=CARTESIAN_POINT('',(-0.504188384727764,1.08252112989365,2.4));
#26407=CARTESIAN_POINT('Ctrl Pts',(-0.726604172280256,1.00006079745576,
2.36934196736194));
#26408=CARTESIAN_POINT('Ctrl Pts',(-0.7263677230741,0.962556440882506,2.37171076053695));
#26409=CARTESIAN_POINT('Ctrl Pts',(-0.708610935503227,0.92486733001342,
2.37407955371196));
#26410=CARTESIAN_POINT('Ctrl Pts',(-0.679417479773344,0.901356582338566,
2.37644834688697));
#26411=CARTESIAN_POINT('Ctrl Pts',(-0.647166920488327,0.875383817458018,
2.37906519723286));
#26412=CARTESIAN_POINT('Ctrl Pts',(-0.600959009984164,0.866714378341853,
2.38168204757875));
#26413=CARTESIAN_POINT('Ctrl Pts',(-0.561514903279023,0.879318622378776,
2.38429889792465));
#26414=CARTESIAN_POINT('Ctrl Pts',(-0.522070796573882,0.891922866415699,
2.38691574827054));
#26415=CARTESIAN_POINT('Ctrl Pts',(-0.489390493667762,0.92580079360571,
2.38953259861643));
#26416=CARTESIAN_POINT('Ctrl Pts',(-0.478135764397917,0.965573612020961,
2.39214944896232));
#26417=CARTESIAN_POINT('Ctrl Pts',(-0.466881035128071,1.00534643043621,
2.39476629930821));
#26418=CARTESIAN_POINT('Ctrl Pts',(-0.4770518794945,1.0510141400767,2.39738314965411));
#26419=CARTESIAN_POINT('Ctrl Pts',(-0.504188384727764,1.08252112989365,
2.4));
#26420=CARTESIAN_POINT('',(-0.695988964037237,1.08263519275223,2.4));
#26421=CARTESIAN_POINT('Origin',(-0.6,1.,2.4));
#26422=CARTESIAN_POINT('Ctrl Pts',(-0.695989827719566,1.0826357482344,2.4));
#26423=CARTESIAN_POINT('Ctrl Pts',(-0.670163685851419,1.11242103345157,
2.3975091839613));
#26424=CARTESIAN_POINT('Ctrl Pts',(-0.629259696534257,1.12936969176545,
2.3950183679226));
#26425=CARTESIAN_POINT('Ctrl Pts',(-0.589969605883147,1.12624203918417,
2.3925275518839));
#26426=CARTESIAN_POINT('Ctrl Pts',(-0.548691452172472,1.12295612861833,
2.38991070153801));
#26427=CARTESIAN_POINT('Ctrl Pts',(-0.509194654494277,1.09751079858255,
2.38729385119211));
#26428=CARTESIAN_POINT('Ctrl Pts',(-0.489166158833217,1.06128256815865,
2.38467700084622));
#26429=CARTESIAN_POINT('Ctrl Pts',(-0.469137663172157,1.02505433773475,
2.38206015050033));
#26430=CARTESIAN_POINT('Ctrl Pts',(-0.468577469528232,0.978043206922726,
2.37944330015444));
#26431=CARTESIAN_POINT('Ctrl Pts',(-0.487748907242888,0.94134646243954,
2.37682644980854));
#26432=CARTESIAN_POINT('Ctrl Pts',(-0.506920344957544,0.904649717956355,
2.37420959946265));
#26433=CARTESIAN_POINT('Ctrl Pts',(-0.54582341403078,0.878267359802006,
2.37159274911676));
#26434=CARTESIAN_POINT('Ctrl Pts',(-0.587007343519609,0.874020939484002,
2.36897589877086));
#26435=CARTESIAN_POINT('Ctrl Pts',(-0.628191273008439,0.869774519165998,
2.36635904842497));
#26436=CARTESIAN_POINT('Ctrl Pts',(-0.671656062912861,0.887664036684341,
2.36374219807908));
#26437=CARTESIAN_POINT('Ctrl Pts',(-0.697914726064929,0.919672001884272,
2.36112534773319));
#26438=CARTESIAN_POINT('Ctrl Pts',(-0.716201899123246,0.94196312902452,
2.35930290936814));
#26439=CARTESIAN_POINT('Ctrl Pts',(-0.726143981825042,0.971101800838385,
2.3574804710031));
#26440=CARTESIAN_POINT('Ctrl Pts',(-0.726369333664333,1.00010094057762,
2.35565803263806));
#26441=CARTESIAN_POINT('Origin',(0.6,1.,2.51042117235887));
#26442=CARTESIAN_POINT('',(0.44550661348391,1.00007637252271,2.03957882764113));
#26443=CARTESIAN_POINT('',(0.445941879748409,0.999994887077554,2.03542117235887));
#26444=CARTESIAN_POINT('',(0.4457,1.,2.51042117235887));
#26445=CARTESIAN_POINT('',(0.639851384185725,0.850935057178149,2.));
#26446=CARTESIAN_POINT('Ctrl Pts',(0.445941879748409,0.999994887077554,
2.03542117235887));
#26447=CARTESIAN_POINT('Ctrl Pts',(0.445958427563446,1.02606888540753,2.03408151628949));
#26448=CARTESIAN_POINT('Ctrl Pts',(0.464522119816522,1.10309173428669,2.03012500987421));
#26449=CARTESIAN_POINT('Ctrl Pts',(0.585586764715563,1.18108624726655,2.02355165311303));
#26450=CARTESIAN_POINT('Ctrl Pts',(0.74321627607811,1.11199512704675,2.01570110207536));
#26451=CARTESIAN_POINT('Ctrl Pts',(0.772174135599484,0.94213024790789,2.00785055103768));
#26452=CARTESIAN_POINT('Ctrl Pts',(0.688870364005735,0.864039910406678,
2.00261685034589));
#26453=CARTESIAN_POINT('Ctrl Pts',(0.639851384185725,0.850935057178149,
2.));
#26454=CARTESIAN_POINT('',(0.560048264277831,0.850698128346977,2.));
#26455=CARTESIAN_POINT('Origin',(0.6,1.,2.));
#26456=CARTESIAN_POINT('Ctrl Pts',(0.44550661348391,1.00007637252271,2.03957882764113));
#26457=CARTESIAN_POINT('Ctrl Pts',(0.445479076365182,1.00461168797626,2.03934410251636));
#26458=CARTESIAN_POINT('Ctrl Pts',(0.447699955244927,1.0596817411018,2.03649252704569));
#26459=CARTESIAN_POINT('Ctrl Pts',(0.513561617374857,1.15981701056446,2.03102410122914));
#26460=CARTESIAN_POINT('Ctrl Pts',(0.685634169421134,1.1602711276025,2.02317355019146));
#26461=CARTESIAN_POINT('Ctrl Pts',(0.780906782004492,1.01693885807272,2.01532299915378));
#26462=CARTESIAN_POINT('Ctrl Pts',(0.715015266367875,0.861059909554376,
2.00759848242329));
#26463=CARTESIAN_POINT('Ctrl Pts',(0.606562024823064,0.838426846369365,
2.0024908160387));
#26464=CARTESIAN_POINT('Ctrl Pts',(0.560047775926799,0.850696975355777,
2.));
#26465=CARTESIAN_POINT('Origin',(0.6,1.,2.51042117235887));
#26466=CARTESIAN_POINT('',(0.445932524475483,1.00003263872856,2.08957882764113));
#26467=CARTESIAN_POINT('',(0.445538932974414,0.999905097479817,2.08542117235887));
#26468=CARTESIAN_POINT('',(0.4457,1.,2.51042117235887));
#26469=CARTESIAN_POINT('Ctrl Pts',(0.445538932974414,0.999905097479817,
2.08542117235887));
#26470=CARTESIAN_POINT('Ctrl Pts',(0.445863620600756,1.04447123493477,2.08311595169817));
#26471=CARTESIAN_POINT('Ctrl Pts',(0.489384741719965,1.14018208017193,2.07819388069158));
#26472=CARTESIAN_POINT('Ctrl Pts',(0.651047898079357,1.17438225782416,2.0706549593391));
#26473=CARTESIAN_POINT('Ctrl Pts',(0.773614618887169,1.05360877841752,2.06280440830142));
#26474=CARTESIAN_POINT('Ctrl Pts',(0.740475677832241,0.884752178886651,
2.05495385726374));
#26475=CARTESIAN_POINT('Ctrl Pts',(0.581362560637208,0.819263360725568,
2.04710330622607));
#26476=CARTESIAN_POINT('Ctrl Pts',(0.463250898323639,0.899361552534091,
2.04059241125778));
#26477=CARTESIAN_POINT('Ctrl Pts',(0.445926103479307,0.975136595316218,
2.03669836663538));
#26478=CARTESIAN_POINT('Ctrl Pts',(0.445941879748409,0.999994887077554,
2.03542117235887));
#26479=CARTESIAN_POINT('Ctrl Pts',(0.445932524475483,1.00003263872856,2.08957882764113));
#26480=CARTESIAN_POINT('Ctrl Pts',(0.445887391771903,1.02338938965811,2.08837853792505));
#26481=CARTESIAN_POINT('Ctrl Pts',(0.461764469489331,1.09760988546538,2.08456139786307));
#26482=CARTESIAN_POINT('Ctrl Pts',(0.57612672137744,1.18012607114374,2.07812740745521));
#26483=CARTESIAN_POINT('Ctrl Pts',(0.737078048375186,1.11926881624917,2.07027685641753));
#26484=CARTESIAN_POINT('Ctrl Pts',(0.775094502137202,0.951447557128672,
2.06242630537985));
#26485=CARTESIAN_POINT('Ctrl Pts',(0.656082084236305,0.827171040068,2.05457575434217));
#26486=CARTESIAN_POINT('Ctrl Pts',(0.491836019895195,0.856969773295158,
2.04695992842926));
#26487=CARTESIAN_POINT('Ctrl Pts',(0.445786075962011,0.954049389522044,
2.04196095286225));
#26488=CARTESIAN_POINT('Ctrl Pts',(0.44550661348391,1.00007637252271,2.03957882764113));
#26489=CARTESIAN_POINT('Origin',(0.6,1.,2.51042117235887));
#26490=CARTESIAN_POINT('',(0.445609664942012,0.999879240692409,2.13957882764113));
#26491=CARTESIAN_POINT('',(0.445723577648801,1.00013290047684,2.13542117235887));
#26492=CARTESIAN_POINT('',(0.4457,1.,2.51042117235887));
#26493=CARTESIAN_POINT('Ctrl Pts',(0.445723577648801,1.00013290047684,2.13542117235887));
#26494=CARTESIAN_POINT('Ctrl Pts',(0.445613060502099,1.01281442421482,2.13476723745276));
#26495=CARTESIAN_POINT('Ctrl Pts',(0.45279637409468,1.07612012598108,2.13149645220075));
#26496=CARTESIAN_POINT('Ctrl Pts',(0.539792347657613,1.17143637275151,2.12560881660284));
#26497=CARTESIAN_POINT('Ctrl Pts',(0.70978808601476,1.14478245624706,2.11775826556517));
#26498=CARTESIAN_POINT('Ctrl Pts',(0.781323293607615,0.988284239491303,
2.10990771452749));
#26499=CARTESIAN_POINT('Ctrl Pts',(0.690243392316909,0.842292899938004,
2.10205716348982));
#26500=CARTESIAN_POINT('Ctrl Pts',(0.518231205927094,0.837737224374896,
2.09420661245213));
#26501=CARTESIAN_POINT('Ctrl Pts',(0.448527232502997,0.937309583846461,
2.08866128207516));
#26502=CARTESIAN_POINT('Ctrl Pts',(0.445495040298755,0.993880454536856,
2.08573280204407));
#26503=CARTESIAN_POINT('Ctrl Pts',(0.445538932974414,0.999905097479817,
2.08542117235887));
#26504=CARTESIAN_POINT('Ctrl Pts',(0.445609664942012,0.999879240692409,
2.13957882764113));
#26505=CARTESIAN_POINT('Ctrl Pts',(0.445970133311311,1.04180105694513,2.13741297333374));
#26506=CARTESIAN_POINT('Ctrl Pts',(0.485126633726011,1.13496755094661,2.13263026868045));
#26507=CARTESIAN_POINT('Ctrl Pts',(0.641820162707069,1.17682322770038,2.12523071368128));
#26508=CARTESIAN_POINT('Ctrl Pts',(0.770558701511974,1.06265070285456,2.11738016264359));
#26509=CARTESIAN_POINT('Ctrl Pts',(0.746336141641471,0.892291522696776,
2.10952961160592));
#26510=CARTESIAN_POINT('Ctrl Pts',(0.590875851708506,0.818527896169216,
2.10167906056824));
#26511=CARTESIAN_POINT('Ctrl Pts',(0.466115932152929,0.893907603907564,
2.09502879924665));
#26512=CARTESIAN_POINT('Ctrl Pts',(0.445985789291595,0.972467415629669,
2.09099538827094));
#26513=CARTESIAN_POINT('Ctrl Pts',(0.445932524475483,1.00003263872856,2.08957882764113));
#26514=CARTESIAN_POINT('Origin',(0.6,1.,2.51042117235887));
#26515=CARTESIAN_POINT('',(0.445644927187824,1.00012792448195,2.18957882764113));
#26516=CARTESIAN_POINT('',(0.445884646673086,0.999912830487253,2.18542117235887));
#26517=CARTESIAN_POINT('',(0.4457,1.,2.51042117235887));
#26518=CARTESIAN_POINT('Ctrl Pts',(0.445884646673086,0.999912830487253,
2.18542117235887));
#26519=CARTESIAN_POINT('Ctrl Pts',(0.446050503878428,1.03140252422683,2.18380167286145));
#26520=CARTESIAN_POINT('Ctrl Pts',(0.470644510125523,1.11401244662307,2.17956532301813));
#26521=CARTESIAN_POINT('Ctrl Pts',(0.604772735062981,1.18163868139168,2.17271212282892));
#26522=CARTESIAN_POINT('Ctrl Pts',(0.754140428515542,1.09620871962996,2.16486157179123));
#26523=CARTESIAN_POINT('Ctrl Pts',(0.765271321801097,0.924496491715462,
2.15701102075356));
#26524=CARTESIAN_POINT('Ctrl Pts',(0.628182963406343,0.820497603368372,
2.14916046971588));
#26525=CARTESIAN_POINT('Ctrl Pts',(0.479344005128078,0.872734156235485,
2.14196385358432));
#26526=CARTESIAN_POINT('Ctrl Pts',(0.446055316804476,0.962066789442876,
2.13738408779865));
#26527=CARTESIAN_POINT('Ctrl Pts',(0.445723577648801,1.00013290047684,2.13542117235887));
#26528=CARTESIAN_POINT('Ctrl Pts',(0.445644927187824,1.00012792448195,2.18957882764113));
#26529=CARTESIAN_POINT('Ctrl Pts',(0.445556744991309,1.01009369744184,2.18906425908832));
#26530=CARTESIAN_POINT('Ctrl Pts',(0.450939973182116,1.07064584055842,2.18593284018961));
#26531=CARTESIAN_POINT('Ctrl Pts',(0.530872330435983,1.16803793011858,2.18018457094502));
#26532=CARTESIAN_POINT('Ctrl Pts',(0.702033231237909,1.1503482635805,2.17233401990734));
#26533=CARTESIAN_POINT('Ctrl Pts',(0.781688304564893,0.997822700079642,
2.16448346886966));
#26534=CARTESIAN_POINT('Ctrl Pts',(0.698400986961052,0.847249790637147,
2.15663291783198));
#26535=CARTESIAN_POINT('Ctrl Pts',(0.526865324912526,0.833666900912216,
2.14878236679431));
#26536=CARTESIAN_POINT('Ctrl Pts',(0.450147764311532,0.931848543518796,
2.14309767006402));
#26537=CARTESIAN_POINT('Ctrl Pts',(0.445534604580841,0.991149857098978,
2.14002982367963));
#26538=CARTESIAN_POINT('Ctrl Pts',(0.445609664942012,0.999879240692409,
2.13957882764113));
#26539=CARTESIAN_POINT('Origin',(0.6,1.,2.51042117235887));
#26540=CARTESIAN_POINT('',(0.445922292476226,0.999948977361648,2.23957882764113));
#26541=CARTESIAN_POINT('',(0.445458679031241,0.999989078051821,2.23542117235887));
#26542=CARTESIAN_POINT('',(0.4457,1.,2.51042117235887));
#26543=CARTESIAN_POINT('Ctrl Pts',(0.445458679031242,0.999989078051821,
2.23542117235887));
#26544=CARTESIAN_POINT('Ctrl Pts',(0.445510650069037,1.04989637335789,2.23283610827014));
#26545=CARTESIAN_POINT('Ctrl Pts',(0.498659772012076,1.15041990786983,2.22763419383551));
#26546=CARTESIAN_POINT('Ctrl Pts',(0.669127678863374,1.16803795272366,2.21981542905498));
#26547=CARTESIAN_POINT('Ctrl Pts',(0.778293256865801,1.03502719068774,2.21196487801731));
#26548=CARTESIAN_POINT('Ctrl Pts',(0.727561203441069,0.870603211369231,
2.20411432697963));
#26549=CARTESIAN_POINT('Ctrl Pts',(0.562429230156179,0.822225348280642,
2.19626377594195));
#26550=CARTESIAN_POINT('Ctrl Pts',(0.458106037926808,0.910370419295299,
2.1900327244017));
#26551=CARTESIAN_POINT('Ctrl Pts',(0.445782505348105,0.980520250977966,
2.18641852320734));
#26552=CARTESIAN_POINT('Ctrl Pts',(0.445884646673086,0.999912830487253,
2.18542117235887));
#26553=CARTESIAN_POINT('Ctrl Pts',(0.445922292476226,0.999948977361648,
2.23957882764113));
#26554=CARTESIAN_POINT('Ctrl Pts',(0.446009681621634,1.02874647305155,2.23809869449701));
#26555=CARTESIAN_POINT('Ctrl Pts',(0.467487221018094,1.10857850003564,2.23400171100699));
#26556=CARTESIAN_POINT('Ctrl Pts',(0.595227265578502,1.18163865695784,2.22728787717108));
#26557=CARTESIAN_POINT('Ctrl Pts',(0.748875240939872,1.10417074102503,2.21943732613341));
#26558=CARTESIAN_POINT('Ctrl Pts',(0.769008360762544,0.933280028245809,
2.21158677509573));
#26559=CARTESIAN_POINT('Ctrl Pts',(0.637570764789711,0.822225372195567,
2.20373622405805));
#26560=CARTESIAN_POINT('Ctrl Pts',(0.483262475482066,0.867432276377129,
2.19640024157318));
#26561=CARTESIAN_POINT('Ctrl Pts',(0.446005197603095,0.959412527217309,
2.19168110943421));
#26562=CARTESIAN_POINT('Ctrl Pts',(0.445644927187824,1.00012792448195,2.18957882764113));
#26563=CARTESIAN_POINT('Origin',(0.6,1.,2.51042117235887));
#26564=CARTESIAN_POINT('',(0.445484911225394,0.999943334804163,2.28957882764113));
#26565=CARTESIAN_POINT('',(0.445861169326679,1.00010096027373,2.28542117235887));
#26566=CARTESIAN_POINT('',(0.4457,1.,2.51042117235887));
#26567=CARTESIAN_POINT('Ctrl Pts',(0.445861169326679,1.00010096027373,2.28542117235887));
#26568=CARTESIAN_POINT('Ctrl Pts',(0.445749296272184,1.01825046503264,2.28448739402472));
#26569=CARTESIAN_POINT('Ctrl Pts',(0.457041409544473,1.08712805126299,2.28093676534467));
#26570=CARTESIAN_POINT('Ctrl Pts',(0.558179831669208,1.17682325150234,2.27476928631873));
#26571=CARTESIAN_POINT('Ctrl Pts',(0.724423708785572,1.13241650393702,2.26691873528105));
#26572=CARTESIAN_POINT('Ctrl Pts',(0.779081445955335,0.969255483615749,
2.25906818424337));
#26573=CARTESIAN_POINT('Ctrl Pts',(0.673134684925636,0.833666878534013,
2.25121763320569));
#26574=CARTESIAN_POINT('Ctrl Pts',(0.50159899980171,0.84724977008965,2.24336708216802));
#26575=CARTESIAN_POINT('Ctrl Pts',(0.445736890155226,0.948241381044753,
2.23810159521908));
#26576=CARTESIAN_POINT('Ctrl Pts',(0.445458039989146,0.999375411980858,
2.23545295861603));
#26577=CARTESIAN_POINT('Ctrl Pts',(0.445458679031242,0.999989078051821,
2.23542117235887));
#26578=CARTESIAN_POINT('Ctrl Pts',(0.445484911225394,0.999943334804162,
2.28957882764113));
#26579=CARTESIAN_POINT('Ctrl Pts',(0.445711121771824,1.04718147797272,2.2871331299057));
#26580=CARTESIAN_POINT('Ctrl Pts',(0.493918064875951,1.14536352796849,2.28207058182437));
#26581=CARTESIAN_POINT('Ctrl Pts',(0.660207644220989,1.17143634973614,2.27439118339715));
#26582=CARTESIAN_POINT('Ctrl Pts',(0.776207730757634,1.04434204382826,2.26654063235948));
#26583=CARTESIAN_POINT('Ctrl Pts',(0.734180526190243,0.87748075149375,2.2586900813218));
#26584=CARTESIAN_POINT('Ctrl Pts',(0.571817040388558,0.820497627508739,
2.25083953028412));
#26585=CARTESIAN_POINT('Ctrl Pts',(0.460575165814633,0.904888683245033,
2.24446911239056));
#26586=CARTESIAN_POINT('Ctrl Pts',(0.445855179091712,0.977832988101724,
2.2407155448429));
#26587=CARTESIAN_POINT('Ctrl Pts',(0.445922292476226,0.999948977361648,
2.23957882764113));
#26588=CARTESIAN_POINT('Origin',(0.6,1.,2.51042117235887));
#26589=CARTESIAN_POINT('',(0.445798439227784,1.00012317213786,2.33957882764113));
#26590=CARTESIAN_POINT('',(0.445758404806891,0.999869526120069,2.33542117235887));
#26591=CARTESIAN_POINT('',(0.4457,1.,2.51042117235887));
#26592=CARTESIAN_POINT('Ctrl Pts',(0.445758404806891,0.999869526120069,
2.33542117235887));
#26593=CARTESIAN_POINT('Ctrl Pts',(0.446067065282869,1.03672406343128,2.33352182943341));
#26594=CARTESIAN_POINT('Ctrl Pts',(0.477632210806756,1.12483092984331,2.32900563616205));
#26595=CARTESIAN_POINT('Ctrl Pts',(0.623873281963166,1.1801260959606,2.3218725925448));
#26596=CARTESIAN_POINT('Ctrl Pts',(0.76341449322476,1.07944244879737,2.31402204150712));
#26597=CARTESIAN_POINT('Ctrl Pts',(0.756401707578768,0.907512694301026,
2.30617149046944));
#26598=CARTESIAN_POINT('Ctrl Pts',(0.609124149502328,0.818527871661859,
2.29832093943176));
#26599=CARTESIAN_POINT('Ctrl Pts',(0.472154957249585,0.883517743796439,
2.29140416672824));
#26600=CARTESIAN_POINT('Ctrl Pts',(0.446062812907388,0.967387710919709,
2.28710424437061));
#26601=CARTESIAN_POINT('Ctrl Pts',(0.445861169326679,1.00010096027373,2.28542117235887));
#26602=CARTESIAN_POINT('Ctrl Pts',(0.445798439227784,1.00012317213786,2.33957882764113));
#26603=CARTESIAN_POINT('Ctrl Pts',(0.445678571748812,1.01554817070058,2.33878441566028));
#26604=CARTESIAN_POINT('Ctrl Pts',(0.454838216821075,1.08164530296445,2.33537315333353));
#26605=CARTESIAN_POINT('Ctrl Pts',(0.548952109888326,1.17438223097154,2.3293450406609));
#26606=CARTESIAN_POINT('Ctrl Pts',(0.717297767916034,1.1387683610531,2.32149448962322));
#26607=CARTESIAN_POINT('Ctrl Pts',(0.780449022522885,0.978702297157564,
2.31364393858554));
#26608=CARTESIAN_POINT('Ctrl Pts',(0.681768782849741,0.837737246759644,
2.30579338754786));
#26609=CARTESIAN_POINT('Ctrl Pts',(0.509756619949943,0.842292920851884,
2.29794283651019));
#26610=CARTESIAN_POINT('Ctrl Pts',(0.447051029253845,0.942803275635825,
2.29253798320794));
#26611=CARTESIAN_POINT('Ctrl Pts',(0.445469080763202,0.996637557724894,
2.28974998025159));
#26612=CARTESIAN_POINT('Ctrl Pts',(0.445484911225394,0.999943334804162,
2.28957882764113));
#26613=CARTESIAN_POINT('Origin',(0.6,1.,2.51042117235887));
#26614=CARTESIAN_POINT('',(0.445864724392684,0.99983533609866,2.38957882764113));
#26615=CARTESIAN_POINT('',(0.44551185913013,1.0000741974826,2.38542117235887));
#26616=CARTESIAN_POINT('',(0.4457,1.,2.51042117235887));
#26617=CARTESIAN_POINT('',(0.560148615814278,0.850935057178148,2.4));
#26618=CARTESIAN_POINT('Ctrl Pts',(0.560148615814278,0.850935057178148,
2.4));
#26619=CARTESIAN_POINT('Ctrl Pts',(0.511129635994267,0.864039910406677,
2.39738314965411));
#26620=CARTESIAN_POINT('Ctrl Pts',(0.455839024989005,0.915869990257929,
2.39390942553448));
#26621=CARTESIAN_POINT('Ctrl Pts',(0.445750544275333,0.983186184474914,
2.39043570141486));
#26622=CARTESIAN_POINT('Ctrl Pts',(0.445864724392684,0.99983533609866,2.38957882764113));
#26623=CARTESIAN_POINT('',(0.639951772688379,0.850698147244252,2.4));
#26624=CARTESIAN_POINT('Origin',(0.6,1.,2.4));
#26625=CARTESIAN_POINT('Ctrl Pts',(0.639952262351544,0.850696991672977,
2.4));
#26626=CARTESIAN_POINT('Ctrl Pts',(0.593438030028895,0.838426877605595,
2.3975091839613));
#26627=CARTESIAN_POINT('Ctrl Pts',(0.490251767896999,0.859960628309645,
2.39264957474759));
#26628=CARTESIAN_POINT('Ctrl Pts',(0.445800376826071,0.954309672447724,
2.38778996553388));
#26629=CARTESIAN_POINT('Ctrl Pts',(0.445511859130131,1.0000741974826,2.38542117235887));
#26630=CARTESIAN_POINT('Origin',(-0.6,1.,2.51042117235887));
#26631=CARTESIAN_POINT('',(-0.75449339269049,1.00007637145626,2.03957882764113));
#26632=CARTESIAN_POINT('',(-0.754058103775977,0.999994895029031,2.03542117235887));
#26633=CARTESIAN_POINT('',(-0.7543,1.,2.51042117235887));
#26634=CARTESIAN_POINT('',(-0.560148615814275,0.850935057178149,2.));
#26635=CARTESIAN_POINT('Ctrl Pts',(-0.754058103775977,0.999994895029031,
2.03542117235887));
#26636=CARTESIAN_POINT('Ctrl Pts',(-0.754041555268885,1.02606889659328,
2.03408151628949));
#26637=CARTESIAN_POINT('Ctrl Pts',(-0.735477862467914,1.10309174989979,
2.03012500987421));
#26638=CARTESIAN_POINT('Ctrl Pts',(-0.614413230072635,1.18108614472194,
2.02355165311304));
#26639=CARTESIAN_POINT('Ctrl Pts',(-0.456783762484268,1.11199525865091,
2.01570110207535));
#26640=CARTESIAN_POINT('Ctrl Pts',(-0.427825820216639,0.942129974923708,
2.00785055103768));
#26641=CARTESIAN_POINT('Ctrl Pts',(-0.511129635994264,0.864039910406679,
2.00261685034589));
#26642=CARTESIAN_POINT('Ctrl Pts',(-0.560148615814275,0.850935057178149,
2.));
#26643=CARTESIAN_POINT('',(-0.639951747396791,0.850698134330425,2.));
#26644=CARTESIAN_POINT('Origin',(-0.6,1.,2.));
#26645=CARTESIAN_POINT('Ctrl Pts',(-0.754493392690491,1.00007637145626,
2.03957882764113));
#26646=CARTESIAN_POINT('Ctrl Pts',(-0.754520929823858,1.00461168712382,
2.03934410251636));
#26647=CARTESIAN_POINT('Ctrl Pts',(-0.752300051092223,1.05968174304917,
2.03649252704569));
#26648=CARTESIAN_POINT('Ctrl Pts',(-0.686438388751686,1.15981702310584,
2.03102410122914));
#26649=CARTESIAN_POINT('Ctrl Pts',(-0.514365822072695,1.16027112465931,
2.02317355019146));
#26650=CARTESIAN_POINT('Ctrl Pts',(-0.41909321999119,1.01693887482571,2.01532299915378));
#26651=CARTESIAN_POINT('Ctrl Pts',(-0.484984709990756,0.861059878644944,
2.00759848242329));
#26652=CARTESIAN_POINT('Ctrl Pts',(-0.593437992489385,0.838426856238601,
2.0024908160387));
#26653=CARTESIAN_POINT('Ctrl Pts',(-0.63995223616215,0.850696980524376,
2.));
#26654=CARTESIAN_POINT('Origin',(-0.6,1.,2.51042117235887));
#26655=CARTESIAN_POINT('',(-0.754067482051008,1.00003263870824,2.08957882764113));
#26656=CARTESIAN_POINT('',(-0.754461050156182,0.999905097350985,2.08542117235887));
#26657=CARTESIAN_POINT('',(-0.7543,1.,2.51042117235887));
#26658=CARTESIAN_POINT('Ctrl Pts',(-0.754461050156182,0.999905097350985,
2.08542117235887));
#26659=CARTESIAN_POINT('Ctrl Pts',(-0.754136362473472,1.0444712301837,2.08311595169818));
#26660=CARTESIAN_POINT('Ctrl Pts',(-0.71061524567478,1.14018206615738,2.07819388069158));
#26661=CARTESIAN_POINT('Ctrl Pts',(-0.548952108412014,1.17438223594748,
2.0706549593391));
#26662=CARTESIAN_POINT('Ctrl Pts',(-0.426385398697532,1.05360877753029,
2.06280440830142));
#26663=CARTESIAN_POINT('Ctrl Pts',(-0.459524339782119,0.884752182582313,
2.05495385726375));
#26664=CARTESIAN_POINT('Ctrl Pts',(-0.618637434184013,0.819263396393857,
2.04710330622607));
#26665=CARTESIAN_POINT('Ctrl Pts',(-0.736749089275893,0.89936154319225,
2.04059241125778));
#26666=CARTESIAN_POINT('Ctrl Pts',(-0.754073880704865,0.975136600184218,
2.03669836663538));
#26667=CARTESIAN_POINT('Ctrl Pts',(-0.754058103775977,0.999994895029031,
2.03542117235887));
#26668=CARTESIAN_POINT('Ctrl Pts',(-0.754067482051008,1.00003263870824,
2.08957882764113));
#26669=CARTESIAN_POINT('Ctrl Pts',(-0.754112614754579,1.02338939061779,
2.08837853792505));
#26670=CARTESIAN_POINT('Ctrl Pts',(-0.738235536361179,1.09760988955354,
2.08456139786307));
#26671=CARTESIAN_POINT('Ctrl Pts',(-0.623873279675432,1.18012607896462,
2.0781274074552));
#26672=CARTESIAN_POINT('Ctrl Pts',(-0.462921945732953,1.11926882096942,
2.07027685641753));
#26673=CARTESIAN_POINT('Ctrl Pts',(-0.424905490600427,0.951447555675582,
2.06242630537985));
#26674=CARTESIAN_POINT('Ctrl Pts',(-0.54391791306908,0.827171031659744,
2.05457575434217));
#26675=CARTESIAN_POINT('Ctrl Pts',(-0.708163985289881,0.856969769057042,
2.04695992842926));
#26676=CARTESIAN_POINT('Ctrl Pts',(-0.754213930063824,0.954049386283767,
2.04196095286225));
#26677=CARTESIAN_POINT('Ctrl Pts',(-0.754493392690491,1.00007637145626,
2.03957882764113));
#26678=CARTESIAN_POINT('Origin',(-0.6,1.,2.51042117235887));
#26679=CARTESIAN_POINT('',(-0.754390341602871,0.999879240687419,2.13957882764113));
#26680=CARTESIAN_POINT('',(-0.75427640544451,1.00013290045585,2.13542117235887));
#26681=CARTESIAN_POINT('',(-0.7543,1.,2.51042117235887));
#26682=CARTESIAN_POINT('Ctrl Pts',(-0.75427640544451,1.00013290045585,2.13542117235887));
#26683=CARTESIAN_POINT('Ctrl Pts',(-0.754386922579298,1.01281442280347,
2.13476723745276));
#26684=CARTESIAN_POINT('Ctrl Pts',(-0.747203609773684,1.07612011763199,
2.13149645220075));
#26685=CARTESIAN_POINT('Ctrl Pts',(-0.660207645725328,1.17143635399922,
2.12560881660285));
#26686=CARTESIAN_POINT('Ctrl Pts',(-0.490211926051119,1.14478244030651,
2.11775826556517));
#26687=CARTESIAN_POINT('Ctrl Pts',(-0.418676726208604,0.988284240908056,
2.10990771452749));
#26688=CARTESIAN_POINT('Ctrl Pts',(-0.509756617677689,0.842292916978238,
2.10205716348981));
#26689=CARTESIAN_POINT('Ctrl Pts',(-0.681768784928714,0.837737242612945,
2.09420661245213));
#26690=CARTESIAN_POINT('Ctrl Pts',(-0.75147275106401,0.937309590263154,
2.08866128207516));
#26691=CARTESIAN_POINT('Ctrl Pts',(-0.754504942839462,0.993880455032877,
2.08573280204407));
#26692=CARTESIAN_POINT('Ctrl Pts',(-0.754461050156182,0.999905097350985,
2.08542117235887));
#26693=CARTESIAN_POINT('Ctrl Pts',(-0.75439034160287,0.999879240687419,
2.13957882764113));
#26694=CARTESIAN_POINT('Ctrl Pts',(-0.754029873218229,1.04180105871682,
2.13741297333374));
#26695=CARTESIAN_POINT('Ctrl Pts',(-0.714873371143386,1.13496755666601,
2.13263026868045));
#26696=CARTESIAN_POINT('Ctrl Pts',(-0.558179835520779,1.17682323520091,
2.12523071368127));
#26697=CARTESIAN_POINT('Ctrl Pts',(-0.429441291256411,1.0626507055017,2.1173801626436));
#26698=CARTESIAN_POINT('Ctrl Pts',(-0.453663852157743,0.892291518147041,
2.10952961160592));
#26699=CARTESIAN_POINT('Ctrl Pts',(-0.609124148673025,0.818527888446316,
2.10167906056824));
#26700=CARTESIAN_POINT('Ctrl Pts',(-0.733884073530661,0.893907599452349,
2.09502879924664));
#26701=CARTESIAN_POINT('Ctrl Pts',(-0.754014217234906,0.972467414452767,
2.09099538827094));
#26702=CARTESIAN_POINT('Ctrl Pts',(-0.754067482051008,1.00003263870824,
2.08957882764113));
#26703=CARTESIAN_POINT('Origin',(-0.6,1.,2.51042117235887));
#26704=CARTESIAN_POINT('',(-0.754355079355554,1.00012792448738,2.18957882764113));
#26705=CARTESIAN_POINT('',(-0.754115336434833,0.999912830496762,2.18542117235887));
#26706=CARTESIAN_POINT('',(-0.7543,1.,2.51042117235887));
#26707=CARTESIAN_POINT('Ctrl Pts',(-0.754115336434833,0.999912830496762,
2.18542117235887));
#26708=CARTESIAN_POINT('Ctrl Pts',(-0.753949479247709,1.03140252078477,
2.18380167286145));
#26709=CARTESIAN_POINT('Ctrl Pts',(-0.72935547569638,1.11401243412622,2.17956532301813));
#26710=CARTESIAN_POINT('Ctrl Pts',(-0.595227265459685,1.1816386614837,2.17271212282892));
#26711=CARTESIAN_POINT('Ctrl Pts',(-0.445859588380167,1.09620870908317,
2.16486157179124));
#26712=CARTESIAN_POINT('Ctrl Pts',(-0.434728696312199,0.924496499994273,
2.15701102075356));
#26713=CARTESIAN_POINT('Ctrl Pts',(-0.571817039685625,0.820497623037239,
2.14916046971588));
#26714=CARTESIAN_POINT('Ctrl Pts',(-0.720655981642513,0.872734170194251,
2.14196385358432));
#26715=CARTESIAN_POINT('Ctrl Pts',(-0.753944666324598,0.962066793595335,
2.13738408779865));
#26716=CARTESIAN_POINT('Ctrl Pts',(-0.75427640544451,1.00013290045585,2.13542117235887));
#26717=CARTESIAN_POINT('Ctrl Pts',(-0.754355079355553,1.00012792448738,
2.18957882764113));
#26718=CARTESIAN_POINT('Ctrl Pts',(-0.754443261555807,1.01009369786974,
2.18906425908832));
#26719=CARTESIAN_POINT('Ctrl Pts',(-0.749060033136799,1.07064584355324,
2.18593284018961));
#26720=CARTESIAN_POINT('Ctrl Pts',(-0.669127672494447,1.16803793724193,
2.18018457094502));
#26721=CARTESIAN_POINT('Ctrl Pts',(-0.497966764436741,1.15034826995414,
2.17233401990734));
#26722=CARTESIAN_POINT('Ctrl Pts',(-0.418311687733005,0.997822699987136,
2.16448346886966));
#26723=CARTESIAN_POINT('Ctrl Pts',(-0.501599008867606,0.847249784162188,
2.15663291783199));
#26724=CARTESIAN_POINT('Ctrl Pts',(-0.673134678187691,0.833666893860354,
2.1487823667943));
#26725=CARTESIAN_POINT('Ctrl Pts',(-0.749852242041061,0.931848540630513,
2.14309767006402));
#26726=CARTESIAN_POINT('Ctrl Pts',(-0.754465401967237,0.99114985672403,
2.14002982367963));
#26727=CARTESIAN_POINT('Ctrl Pts',(-0.75439034160287,0.999879240687419,
2.13957882764113));
#26728=CARTESIAN_POINT('Origin',(-0.6,1.,2.51042117235887));
#26729=CARTESIAN_POINT('',(-0.75407771405525,0.999948977359204,2.23957882764113));
#26730=CARTESIAN_POINT('',(-0.754541304029948,0.999989078053162,2.23542117235887));
#26731=CARTESIAN_POINT('',(-0.7543,1.,2.51042117235887));
#26732=CARTESIAN_POINT('Ctrl Pts',(-0.754541304029948,0.999989078053162,
2.23542117235887));
#26733=CARTESIAN_POINT('Ctrl Pts',(-0.754489332997837,1.04989636788915,
2.23283610827014));
#26734=CARTESIAN_POINT('Ctrl Pts',(-0.701340216880369,1.15041989138249,
2.2276341938355));
#26735=CARTESIAN_POINT('Ctrl Pts',(-0.530872328713473,1.16803793430571,
2.21981542905499));
#26736=CARTESIAN_POINT('Ctrl Pts',(-0.421706762676398,1.0350271868484,2.2119648780173));
#26737=CARTESIAN_POINT('Ctrl Pts',(-0.472438810540477,0.870603225552124,
2.20411432697963));
#26738=CARTESIAN_POINT('Ctrl Pts',(-0.637570765725878,0.822225367765818,
2.19626377594195));
#26739=CARTESIAN_POINT('Ctrl Pts',(-0.741893946520544,0.910370429119493,
2.1900327244017));
#26740=CARTESIAN_POINT('Ctrl Pts',(-0.754217477748594,0.980520253113081,
2.18641852320734));
#26741=CARTESIAN_POINT('Ctrl Pts',(-0.754115336434833,0.999912830496762,
2.18542117235887));
#26742=CARTESIAN_POINT('Ctrl Pts',(-0.75407771405525,0.999948977359204,
2.23957882764113));
#26743=CARTESIAN_POINT('Ctrl Pts',(-0.753990324906209,1.02874647427002,
2.23809869449701));
#26744=CARTESIAN_POINT('Ctrl Pts',(-0.732512784599607,1.10857850463897,
2.23400171100699));
#26745=CARTESIAN_POINT('Ctrl Pts',(-0.604772734623643,1.18163866465747,
2.22728787717109));
#26746=CARTESIAN_POINT('Ctrl Pts',(-0.451124752749149,1.10417074544119,
2.21943732613341));
#26747=CARTESIAN_POINT('Ctrl Pts',(-0.43099163207285,0.933280025417337,
2.21158677509573));
#26748=CARTESIAN_POINT('Ctrl Pts',(-0.562429233617627,0.822225364659454,
2.20373622405805));
#26749=CARTESIAN_POINT('Ctrl Pts',(-0.716737529466624,0.867432270757321,
2.19640024157319));
#26750=CARTESIAN_POINT('Ctrl Pts',(-0.753994808925007,0.959412525496741,
2.19168110943421));
#26751=CARTESIAN_POINT('Ctrl Pts',(-0.754355079355553,1.00012792448738,
2.18957882764113));
#26752=CARTESIAN_POINT('Origin',(-0.6,1.,2.51042117235887));
#26753=CARTESIAN_POINT('',(-0.754515095317817,0.999943334786189,2.28957882764113));
#26754=CARTESIAN_POINT('',(-0.754138813779314,1.00010096025924,2.28542117235887));
#26755=CARTESIAN_POINT('',(-0.7543,1.,2.51042117235887));
#26756=CARTESIAN_POINT('Ctrl Pts',(-0.754138813779314,1.00010096025924,
2.28542117235887));
#26757=CARTESIAN_POINT('Ctrl Pts',(-0.754250686820938,1.01825046303266,
2.28448739402472));
#26758=CARTESIAN_POINT('Ctrl Pts',(-0.74295857478395,1.08712804172823,2.28093676534467));
#26759=CARTESIAN_POINT('Ctrl Pts',(-0.641820163748749,1.17682323210921,
2.27476928631873));
#26760=CARTESIAN_POINT('Ctrl Pts',(-0.47557630485125,1.13241648942973,2.26691873528105));
#26761=CARTESIAN_POINT('Ctrl Pts',(-0.420918573673669,0.969255486982105,
2.25906818424337));
#26762=CARTESIAN_POINT('Ctrl Pts',(-0.526865323090207,0.833666896767115,
2.2512176332057));
#26763=CARTESIAN_POINT('Ctrl Pts',(-0.698400989412974,0.847249786831145,
2.24336708216802));
#26764=CARTESIAN_POINT('Ctrl Pts',(-0.75426309293647,0.948241386717884,
2.23810159521908));
#26765=CARTESIAN_POINT('Ctrl Pts',(-0.754541943071973,0.999375412049459,
2.23545295861603));
#26766=CARTESIAN_POINT('Ctrl Pts',(-0.754541304029948,0.999989078053162,
2.23542117235887));
#26767=CARTESIAN_POINT('Ctrl Pts',(-0.754515095317817,0.999943334786189,
2.28957882764113));
#26768=CARTESIAN_POINT('Ctrl Pts',(-0.754288884759399,1.04718147995109,
2.2871331299057));
#26769=CARTESIAN_POINT('Ctrl Pts',(-0.706081939633174,1.1453635341575,2.28207058182437));
#26770=CARTESIAN_POINT('Ctrl Pts',(-0.539792353219763,1.17143635698873,
2.27439118339715));
#26771=CARTESIAN_POINT('Ctrl Pts',(-0.423792261776434,1.04434204571596,
2.26654063235948));
#26772=CARTESIAN_POINT('Ctrl Pts',(-0.465819468119529,0.877480746295693,
2.2586900813218));
#26773=CARTESIAN_POINT('Ctrl Pts',(-0.6281829608073,0.820497619901593,2.25083953028412));
#26774=CARTESIAN_POINT('Ctrl Pts',(-0.73942484009554,0.90488867921255,2.24446911239056));
#26775=CARTESIAN_POINT('Ctrl Pts',(-0.754144827442555,0.977832987161639,
2.2407155448429));
#26776=CARTESIAN_POINT('Ctrl Pts',(-0.75407771405525,0.999948977359204,
2.23957882764113));
#26777=CARTESIAN_POINT('Origin',(-0.6,1.,2.51042117235887));
#26778=CARTESIAN_POINT('',(-0.754201567294635,1.0001231722509,2.33957882764113));
#26779=CARTESIAN_POINT('',(-0.754241578414675,0.999869525658411,2.33542117235887));
#26780=CARTESIAN_POINT('',(-0.7543,1.,2.51042117235887));
#26781=CARTESIAN_POINT('Ctrl Pts',(-0.754241578414675,0.999869525658411,
2.33542117235887));
#26782=CARTESIAN_POINT('Ctrl Pts',(-0.753932917948777,1.03672405905087,
2.33352182943341));
#26783=CARTESIAN_POINT('Ctrl Pts',(-0.72236777560142,1.12483091690338,2.32900563616205));
#26784=CARTESIAN_POINT('Ctrl Pts',(-0.576126720758545,1.18012607574093,
2.3218725925448));
#26785=CARTESIAN_POINT('Ctrl Pts',(-0.436585524633584,1.079442440351,2.31402204150712));
#26786=CARTESIAN_POINT('Ctrl Pts',(-0.443598309590693,0.907512704295987,
2.30617149046944));
#26787=CARTESIAN_POINT('Ctrl Pts',(-0.59087585148424,0.818527891629664,
2.29832093943176));
#26788=CARTESIAN_POINT('Ctrl Pts',(-0.727845028742113,0.883517756536112,
2.29140416672824));
#26789=CARTESIAN_POINT('Ctrl Pts',(-0.753937170221803,0.967387714483928,
2.28710424437061));
#26790=CARTESIAN_POINT('Ctrl Pts',(-0.754138813779314,1.00010096025924,
2.28542117235887));
#26791=CARTESIAN_POINT('Ctrl Pts',(-0.754201567294635,1.0001231722509,2.33957882764113));
#26792=CARTESIAN_POINT('Ctrl Pts',(-0.754321434708458,1.01554817119723,
2.33878441566028));
#26793=CARTESIAN_POINT('Ctrl Pts',(-0.745161788983251,1.08164530518807,
2.33537315333353));
#26794=CARTESIAN_POINT('Ctrl Pts',(-0.651047892623131,1.17438223943631,
2.3293450406609));
#26795=CARTESIAN_POINT('Ctrl Pts',(-0.48270222690289,1.13876836634555,2.32149448962322));
#26796=CARTESIAN_POINT('Ctrl Pts',(-0.419550969949932,0.978702296577685,
2.31364393858554));
#26797=CARTESIAN_POINT('Ctrl Pts',(-0.518231213613428,0.837737239705173,
2.30579338754787));
#26798=CARTESIAN_POINT('Ctrl Pts',(-0.690243383915708,0.842292914261777,
2.29794283651019));
#26799=CARTESIAN_POINT('Ctrl Pts',(-0.752948977226896,0.9428032732054,2.29253798320794));
#26800=CARTESIAN_POINT('Ctrl Pts',(-0.754530925780848,0.996637557567215,
2.28974998025159));
#26801=CARTESIAN_POINT('Ctrl Pts',(-0.754515095317817,0.999943334786189,
2.28957882764113));
#26802=CARTESIAN_POINT('Origin',(-0.6,1.,2.51042117235887));
#26803=CARTESIAN_POINT('',(-0.754135271629158,0.999835375941562,2.38957882764113));
#26804=CARTESIAN_POINT('',(-0.754488127978201,1.0000741878009,2.38542117235887));
#26805=CARTESIAN_POINT('',(-0.7543,1.,2.51042117235887));
#26806=CARTESIAN_POINT('',(-0.639851384185722,0.850935057178148,2.4));
#26807=CARTESIAN_POINT('Ctrl Pts',(-0.639851384185722,0.850935057178148,
2.4));
#26808=CARTESIAN_POINT('Ctrl Pts',(-0.688870364005733,0.864039910406677,
2.39738314965411));
#26809=CARTESIAN_POINT('Ctrl Pts',(-0.744160963654378,0.915870060408085,
2.39390942553448));
#26810=CARTESIAN_POINT('Ctrl Pts',(-0.754249449960209,0.983186232192211,
2.39043570141486));
#26811=CARTESIAN_POINT('Ctrl Pts',(-0.754135271629158,0.999835375941562,
2.38957882764113));
#26812=CARTESIAN_POINT('',(-0.560048257412569,0.850698131867252,2.4));
#26813=CARTESIAN_POINT('Origin',(-0.6,1.,2.4));
#26814=CARTESIAN_POINT('Ctrl Pts',(-0.56004776881791,0.850696978396875,
2.4));
#26815=CARTESIAN_POINT('Ctrl Pts',(-0.606562014643699,0.838426852173434,
2.3975091839613));
#26816=CARTESIAN_POINT('Ctrl Pts',(-0.709748176229453,0.859960702974294,
2.39264957474759));
#26817=CARTESIAN_POINT('Ctrl Pts',(-0.754199601979702,0.954309678356425,
2.38778996553388));
#26818=CARTESIAN_POINT('Ctrl Pts',(-0.754488127978201,1.0000741878009,2.38542117235887));
#26819=CARTESIAN_POINT('Origin',(-0.6,1.,2.51042117235887));
#26820=CARTESIAN_POINT('Ctrl Pts',(-0.754488127978201,1.0000741878009,2.38542117235887));
#26821=CARTESIAN_POINT('Ctrl Pts',(-0.754518342073576,1.00486659216084,
2.38517311518799));
#26822=CARTESIAN_POINT('Ctrl Pts',(-0.75215961407118,1.06018735745674,2.38230820767121));
#26823=CARTESIAN_POINT('Ctrl Pts',(-0.685634174422424,1.16027112587027,
2.37682644980854));
#26824=CARTESIAN_POINT('Ctrl Pts',(-0.513561613772921,1.15981701793772,
2.36897589877087));
#26825=CARTESIAN_POINT('Ctrl Pts',(-0.419009660745144,1.01606137072615,
2.36112534773318));
#26826=CARTESIAN_POINT('Ctrl Pts',(-0.486773837186857,0.857888188850051,
2.35327479669551));
#26827=CARTESIAN_POINT('Ctrl Pts',(-0.656082085820325,0.827171035125292,
2.34542424565783));
#26828=CARTESIAN_POINT('Ctrl Pts',(-0.746300935356365,0.921380401738197,
2.33947303754562));
#26829=CARTESIAN_POINT('Ctrl Pts',(-0.754358179883375,0.985947131323567,
2.3361386797793));
#26830=CARTESIAN_POINT('Ctrl Pts',(-0.754241578414675,0.999869525658411,
2.33542117235887));
#26831=CARTESIAN_POINT('Ctrl Pts',(-0.754135271629158,0.999835375941562,
2.38957882764113));
#26832=CARTESIAN_POINT('Ctrl Pts',(-0.753900754954872,1.03403189804748,
2.38781885106897));
#26833=CARTESIAN_POINT('Ctrl Pts',(-0.726011265053425,1.1195363898437,2.38344202415091));
#26834=CARTESIAN_POINT('Ctrl Pts',(-0.585586769094172,1.18108616109394,
2.37644834688697));
#26835=CARTESIAN_POINT('Ctrl Pts',(-0.44099944093888,1.08793753892263,2.36859779584929));
#26836=CARTESIAN_POINT('Ctrl Pts',(-0.438948720197302,0.915842224941729,
2.36074724481161));
#26837=CARTESIAN_POINT('Ctrl Pts',(-0.581362564989717,0.819263390701727,
2.35289669377393));
#26838=CARTESIAN_POINT('Ctrl Pts',(-0.724374710267433,0.878125248400964,
2.34584055471711));
#26839=CARTESIAN_POINT('Ctrl Pts',(-0.753926582804302,0.964737112450477,
2.34140126600617));
#26840=CARTESIAN_POINT('Ctrl Pts',(-0.754201567294635,1.0001231722509,2.33957882764113));
#26841=CARTESIAN_POINT('Ctrl Pts',(-0.504188384727764,1.08252112989365,
2.4));
#26842=CARTESIAN_POINT('Ctrl Pts',(-0.4770518794945,1.0510141400767,2.39738314965411));
#26843=CARTESIAN_POINT('Ctrl Pts',(-0.456710190761643,0.959678720795721,
2.39214944896232));
#26844=CARTESIAN_POINT('Ctrl Pts',(-0.554751099480001,0.858044939225688,
2.38429889792465));
#26845=CARTESIAN_POINT('Ctrl Pts',(-0.69337483099249,0.884053256574183,
2.37644834688697));
#26846=CARTESIAN_POINT('Ctrl Pts',(-0.7482544551901,1.01388152850897,2.36859779584929));
#26847=CARTESIAN_POINT('Ctrl Pts',(-0.670177844171844,1.13134338215356,
2.36074724481161));
#26848=CARTESIAN_POINT('Ctrl Pts',(-0.52916309826044,1.13097123731837,2.35289669377393));
#26849=CARTESIAN_POINT('Ctrl Pts',(-0.451677068057184,1.01316241301569,
2.34504614273626));
#26850=CARTESIAN_POINT('Ctrl Pts',(-0.507210315698497,0.883538311601356,
2.33719559169857));
#26851=CARTESIAN_POINT('Ctrl Pts',(-0.645959687310304,0.858365375188547,
2.3293450406609));
#26852=CARTESIAN_POINT('Ctrl Pts',(-0.743491252981436,0.960210910505111,
2.32149448962322));
#26853=CARTESIAN_POINT('Ctrl Pts',(-0.712336485126218,1.097741686102,2.31364393858554));
#26854=CARTESIAN_POINT('Ctrl Pts',(-0.580435669733753,1.14761466155179,
2.30579338754787));
#26855=CARTESIAN_POINT('Ctrl Pts',(-0.466080619506913,1.06510367195323,
2.29794283651019));
#26856=CARTESIAN_POINT('Ctrl Pts',(-0.471827649045646,0.924205971861489,
2.29009228547251));
#26857=CARTESIAN_POINT('Ctrl Pts',(-0.592522692288931,0.851282254676416,
2.28224173443483));
#26858=CARTESIAN_POINT('Ctrl Pts',(-0.719923561707409,0.911732097905615,
2.27439118339715));
#26859=CARTESIAN_POINT('Ctrl Pts',(-0.739774130548921,1.051342719201,2.26654063235948));
#26860=CARTESIAN_POINT('Ctrl Pts',(-0.634271935878349,1.14490795657946,
2.2586900813218));
#26861=CARTESIAN_POINT('Ctrl Pts',(-0.498033854494106,1.10851629998956,
2.25083953028412));
#26862=CARTESIAN_POINT('Ctrl Pts',(-0.453241436429265,0.974804642442561,
2.24298897924644));
#26863=CARTESIAN_POINT('Ctrl Pts',(-0.540065587198681,0.86368878221777,
2.23513842820877));
#26864=CARTESIAN_POINT('Ctrl Pts',(-0.680640344207846,0.874820061858706,
2.22728787717108));
#26865=CARTESIAN_POINT('Ctrl Pts',(-0.748894923426505,0.998215686443256,
2.21943732613341));
#26866=CARTESIAN_POINT('Ctrl Pts',(-0.68361699553809,1.12321152562211,2.21158677509573));
#26867=CARTESIAN_POINT('Ctrl Pts',(-0.543349358171216,1.13770833955254,
2.20373622405805));
#26868=CARTESIAN_POINT('Ctrl Pts',(-0.453887363191384,1.02870504068037,
2.19588567302037));
#26869=CARTESIAN_POINT('Ctrl Pts',(-0.49546265452264,0.893958378944044,
2.1880351219827));
#26870=CARTESIAN_POINT('Ctrl Pts',(-0.630789522527785,0.854312363927335,
2.18018457094502));
#26871=CARTESIAN_POINT('Ctrl Pts',(-0.73850361471777,0.945322484520081,
2.17233401990734));
#26872=CARTESIAN_POINT('Ctrl Pts',(-0.722004372559477,1.08536870078326,
2.16448346886966));
#26873=CARTESIAN_POINT('Ctrl Pts',(-0.596088708472957,1.14885423684131,
2.15663291783199));
#26874=CARTESIAN_POINT('Ctrl Pts',(-0.473680783866961,1.07884375413848,
2.14878236679431));
#26875=CARTESIAN_POINT('Ctrl Pts',(-0.464558934858572,0.938124319016692,
2.14093181575663));
#26876=CARTESIAN_POINT('Ctrl Pts',(-0.576903853974382,0.85289646424536,
2.13308126471895));
#26877=CARTESIAN_POINT('Ctrl Pts',(-0.709961944003222,0.899594560207548,
2.12523071368127));
#26878=CARTESIAN_POINT('Ctrl Pts',(-0.744403552230901,1.03633863630844,
2.1173801626436));
#26879=CARTESIAN_POINT('Ctrl Pts',(-0.64934061440031,1.14049336981984,2.10952961160591));
#26880=CARTESIAN_POINT('Ctrl Pts',(-0.510027855146882,1.11865028889668,
2.10167906056824));
#26881=CARTESIAN_POINT('Ctrl Pts',(-0.451404225723124,0.99039884810644,
2.09382850953056));
#26882=CARTESIAN_POINT('Ctrl Pts',(-0.526044875601709,0.87075787007063,
2.08597795849289));
#26883=CARTESIAN_POINT('Ctrl Pts',(-0.667010128672949,0.867024460974769,
2.0781274074552));
#26884=CARTESIAN_POINT('Ctrl Pts',(-0.747879322472409,0.982546373509308,
2.07027685641753));
#26885=CARTESIAN_POINT('Ctrl Pts',(-0.696126397524862,1.11372170867476,
2.06242630537985));
#26886=CARTESIAN_POINT('Ctrl Pts',(-0.558165872383014,1.14290754203214,
2.05457575434217));
#26887=CARTESIAN_POINT('Ctrl Pts',(-0.457721540280641,1.04393279273302,
2.04672520330449));
#26888=CARTESIAN_POINT('Ctrl Pts',(-0.484879149484439,0.905553554682652,
2.03887465226682));
#26889=CARTESIAN_POINT('Ctrl Pts',(-0.615273516218849,0.851885006312401,
2.03102410122914));
#26890=CARTESIAN_POINT('Ctrl Pts',(-0.731982722301914,0.931032073672457,
2.02317355019146));
#26891=CARTESIAN_POINT('Ctrl Pts',(-0.730302140552184,1.07206547359851,
2.01532299915378));
#26892=CARTESIAN_POINT('Ctrl Pts',(-0.611811749466523,1.14840144523713,
2.0074724481161));
#26893=CARTESIAN_POINT('Ctrl Pts',(-0.482633225963291,1.09178094916661,
1.99962189707843));
#26894=CARTESIAN_POINT('Ctrl Pts',(-0.45890197645103,0.952575083143895,
1.99177134604075));
#26895=CARTESIAN_POINT('Ctrl Pts',(-0.527170074345267,0.888579693265875,
1.98653764534896));
#26896=CARTESIAN_POINT('Ctrl Pts',(-0.56734149364689,0.877840168374445,
1.98392079500307));
#26897=CARTESIAN_POINT('Ctrl Pts',(-0.497154370004338,1.08857942294107,
2.40535973499898));
#26898=CARTESIAN_POINT('Ctrl Pts',(-0.468025636826573,1.05475934582637,
2.40274288465309));
#26899=CARTESIAN_POINT('Ctrl Pts',(-0.446190561956348,0.956718531983702,
2.3975091839613));
#26900=CARTESIAN_POINT('Ctrl Pts',(-0.551429149092544,0.847623301048373,
2.38965863292362));
#26901=CARTESIAN_POINT('Ctrl Pts',(-0.700229949071154,0.875541020369071,
2.38180808188594));
#26902=CARTESIAN_POINT('Ctrl Pts',(-0.759138563736414,1.01490064164717,
2.37395753084827));
#26903=CARTESIAN_POINT('Ctrl Pts',(-0.675329954255372,1.14098596339246,
2.36610697981059));
#26904=CARTESIAN_POINT('Ctrl Pts',(-0.523962603431266,1.14058649752482,
2.35825642877291));
#26905=CARTESIAN_POINT('Ctrl Pts',(-0.440787932286505,1.01412873225251,
2.35040587773523));
#26906=CARTESIAN_POINT('Ctrl Pts',(-0.500398156194616,0.874988270684254,
2.34255532669756));
#26907=CARTESIAN_POINT('Ctrl Pts',(-0.649333820146978,0.84796726183413,
2.33470477565988));
#26908=CARTESIAN_POINT('Ctrl Pts',(-0.754025670789615,0.957289792428312,
2.3268542246222));
#26909=CARTESIAN_POINT('Ctrl Pts',(-0.720583674030304,1.10491739707588,
2.31900367358452));
#26910=CARTESIAN_POINT('Ctrl Pts',(-0.578999353408684,1.15845179961484,
2.31115312254684));
#26911=CARTESIAN_POINT('Ctrl Pts',(-0.456248921215803,1.06988326141916,
2.30330257150917));
#26912=CARTESIAN_POINT('Ctrl Pts',(-0.462417869227328,0.918641549339655,
2.29545202047149));
#26913=CARTESIAN_POINT('Ctrl Pts',(-0.591973745354034,0.840364133660832,
2.28760146943381));
#26914=CARTESIAN_POINT('Ctrl Pts',(-0.728727756233707,0.905251905277888,
2.27975091839613));
#26915=CARTESIAN_POINT('Ctrl Pts',(-0.750035655620193,1.05511204760418,
2.27190036735845));
#26916=CARTESIAN_POINT('Ctrl Pts',(-0.636788011835149,1.15554638175604,
2.26404981632077));
#26917=CARTESIAN_POINT('Ctrl Pts',(-0.490548004613153,1.11648302980295,
2.2561992652831));
#26918=CARTESIAN_POINT('Ctrl Pts',(-0.442467148844067,0.972954923955743,
2.24834871424542));
#26919=CARTESIAN_POINT('Ctrl Pts',(-0.535665499162523,0.85368148706755,
2.24049816320774));
#26920=CARTESIAN_POINT('Ctrl Pts',(-0.686560559276222,0.865629970182854,
2.23264761217006));
#26921=CARTESIAN_POINT('Ctrl Pts',(-0.759826051981739,0.998084690970592,
2.22479706113239));
#26922=CARTESIAN_POINT('Ctrl Pts',(-0.689755741618848,1.13225710619039,
2.21694651009471));
#26923=CARTESIAN_POINT('Ctrl Pts',(-0.539190348351968,1.14781820447026,
2.20909595905703));
#26924=CARTESIAN_POINT('Ctrl Pts',(-0.443160496353055,1.03081242273638,
2.20124540801935));
#26925=CARTESIAN_POINT('Ctrl Pts',(-0.48778803986192,0.886173327813403,
2.19339485698167));
#26926=CARTESIAN_POINT('Ctrl Pts',(-0.633049936927148,0.843616698540163,
2.185544305944));
#26927=CARTESIAN_POINT('Ctrl Pts',(-0.748671864803154,0.941308331874462,
2.17769375490632));
#26928=CARTESIAN_POINT('Ctrl Pts',(-0.730961329922812,1.09163604839579,
2.16984320386864));
#26929=CARTESIAN_POINT('Ctrl Pts',(-0.595801560801866,1.15978237838877,
2.16199265283096));
#26930=CARTESIAN_POINT('Ctrl Pts',(-0.46440705203803,1.08463207245338,2.15414210179328));
#26931=CARTESIAN_POINT('Ctrl Pts',(-0.454615522009781,0.933581712675886,
2.14629155075561));
#26932=CARTESIAN_POINT('Ctrl Pts',(-0.575208249211462,0.842096850509319,
2.13844099971793));
#26933=CARTESIAN_POINT('Ctrl Pts',(-0.718034805847138,0.892223289617803,
2.13059044868025));
#26934=CARTESIAN_POINT('Ctrl Pts',(-0.755004946535977,1.03900643918491,
2.12273989764257));
#26935=CARTESIAN_POINT('Ctrl Pts',(-0.652962958175316,1.15080769787963,
2.11488934660489));
#26936=CARTESIAN_POINT('Ctrl Pts',(-0.503422545448295,1.12736100603329,
2.10703879556722));
#26937=CARTESIAN_POINT('Ctrl Pts',(-0.440495059218284,0.989693979040313,
2.09918824452954));
#26938=CARTESIAN_POINT('Ctrl Pts',(-0.520615456293703,0.861269552373166,
2.09133769349186));
#26939=CARTESIAN_POINT('Ctrl Pts',(-0.671929680758203,0.857262054854161,
2.08348714245418));
#26940=CARTESIAN_POINT('Ctrl Pts',(-0.758735890630724,0.98126501461181,
2.07563659141651));
#26941=CARTESIAN_POINT('Ctrl Pts',(-0.703183522003752,1.12207059383778,
2.06778604037882));
#26942=CARTESIAN_POINT('Ctrl Pts',(-0.555094617726015,1.15339910667059,
2.05993548934115));
#26943=CARTESIAN_POINT('Ctrl Pts',(-0.447276159752938,1.04715812099878,
2.05208493830347));
#26944=CARTESIAN_POINT('Ctrl Pts',(-0.476427546250332,0.89861976398254,
2.0442343872658));
#26945=CARTESIAN_POINT('Ctrl Pts',(-0.616394822207238,0.841011136339552,
2.03638383622811));
#26946=CARTESIAN_POINT('Ctrl Pts',(-0.74167224073109,0.925968789770463,
2.02853328519044));
#26947=CARTESIAN_POINT('Ctrl Pts',(-0.73986827898471,1.07735616409467,2.02068273415276));
#26948=CARTESIAN_POINT('Ctrl Pts',(-0.612678909668559,1.1592963450654,2.01283218311508));
#26949=CARTESIAN_POINT('Ctrl Pts',(-0.474016738136951,1.09851905232804,
2.0049816320774));
#26950=CARTESIAN_POINT('Ctrl Pts',(-0.448543257706232,0.949093380403833,
1.99713108103973));
#26951=CARTESIAN_POINT('Ctrl Pts',(-0.5218232615616,0.880399765646143,1.99189738034794));
#26952=CARTESIAN_POINT('Ctrl Pts',(-0.564943867702685,0.86887179797568,
1.98928053000205));
#26953=CARTESIAN_POINT('Ctrl Pts',(-0.490120355280912,1.09463771598849,
2.41071946999795));
#26954=CARTESIAN_POINT('Ctrl Pts',(-0.458999394158645,1.05850455157604,
2.40810261965206));
#26955=CARTESIAN_POINT('Ctrl Pts',(-0.435670933151054,0.953758343171685,
2.40286891896027));
#26956=CARTESIAN_POINT('Ctrl Pts',(-0.548107198705087,0.837201662871056,
2.3950183679226));
#26957=CARTESIAN_POINT('Ctrl Pts',(-0.707085067149817,0.867028784163962,
2.38716781688492));
#26958=CARTESIAN_POINT('Ctrl Pts',(-0.770022672282728,1.01591975478537,
2.37931726584724));
#26959=CARTESIAN_POINT('Ctrl Pts',(-0.680482064338898,1.15062854463137,
2.37146671480957));
#26960=CARTESIAN_POINT('Ctrl Pts',(-0.518762108602093,1.15020175773127,
2.36361616377188));
#26961=CARTESIAN_POINT('Ctrl Pts',(-0.429898796515824,1.01509505148933,
2.35576561273421));
#26962=CARTESIAN_POINT('Ctrl Pts',(-0.493585996690737,0.866438229767152,
2.34791506169653));
#26963=CARTESIAN_POINT('Ctrl Pts',(-0.652707952983651,0.837569148479711,
2.34006451065885));
#26964=CARTESIAN_POINT('Ctrl Pts',(-0.764560088597795,0.954368674351516,
2.33221395962117));
#26965=CARTESIAN_POINT('Ctrl Pts',(-0.728830862934391,1.11209310804976,
2.3243634085835));
#26966=CARTESIAN_POINT('Ctrl Pts',(-0.577563037083615,1.16928893767788,
2.31651285754582));
#26967=CARTESIAN_POINT('Ctrl Pts',(-0.446417222924693,1.07466285088508,
2.30866230650814));
#26968=CARTESIAN_POINT('Ctrl Pts',(-0.453008089409011,0.913077126817822,
2.30081175547046));
#26969=CARTESIAN_POINT('Ctrl Pts',(-0.591424798419137,0.829446012645248,
2.29296120443278));
#26970=CARTESIAN_POINT('Ctrl Pts',(-0.737531950760006,0.89877171265016,
2.28511065339511));
#26971=CARTESIAN_POINT('Ctrl Pts',(-0.760297180691466,1.05888137600737,
2.27726010235743));
#26972=CARTESIAN_POINT('Ctrl Pts',(-0.639304087791949,1.16618480693263,
2.26940955131975));
#26973=CARTESIAN_POINT('Ctrl Pts',(-0.483062154732201,1.12444975961634,
2.26155900028207));
#26974=CARTESIAN_POINT('Ctrl Pts',(-0.431692861258868,0.971105205468923,
2.25370844924439));
#26975=CARTESIAN_POINT('Ctrl Pts',(-0.531265411126364,0.843674191917333,
2.24585789820672));
#26976=CARTESIAN_POINT('Ctrl Pts',(-0.692480774344598,0.856439878506999,
2.23800734716904));
#26977=CARTESIAN_POINT('Ctrl Pts',(-0.770757180536974,0.997953695497927,
2.23015679613137));
#26978=CARTESIAN_POINT('Ctrl Pts',(-0.695894487699607,1.14130268675866,
2.22230624509368));
#26979=CARTESIAN_POINT('Ctrl Pts',(-0.53503133853272,1.15792806938798,2.21445569405601));
#26980=CARTESIAN_POINT('Ctrl Pts',(-0.432433629514727,1.03291980479239,
2.20660514301833));
#26981=CARTESIAN_POINT('Ctrl Pts',(-0.480113425201198,0.878388276682764,
2.19875459198065));
#26982=CARTESIAN_POINT('Ctrl Pts',(-0.635310351326514,0.83292103315299,
2.19090404094297));
#26983=CARTESIAN_POINT('Ctrl Pts',(-0.758840114888534,0.937294179228842,
2.18305348990529));
#26984=CARTESIAN_POINT('Ctrl Pts',(-0.739918287286149,1.09790339600832,
2.17520293886762));
#26985=CARTESIAN_POINT('Ctrl Pts',(-0.595514413130776,1.17071051993624,
2.16735238782994));
#26986=CARTESIAN_POINT('Ctrl Pts',(-0.455133320209099,1.09042039076827,
2.15950183679226));
#26987=CARTESIAN_POINT('Ctrl Pts',(-0.44467210916099,0.92903910633508,2.15165128575458));
#26988=CARTESIAN_POINT('Ctrl Pts',(-0.573512644448544,0.831297236773279,
2.14380073471691));
#26989=CARTESIAN_POINT('Ctrl Pts',(-0.726107667691055,0.884852019028058,
2.13595018367922));
#26990=CARTESIAN_POINT('Ctrl Pts',(-0.765606340841053,1.04167424206138,
2.12809963264155));
#26991=CARTESIAN_POINT('Ctrl Pts',(-0.656585301950322,1.16112202593943,
2.12024908160387));
#26992=CARTESIAN_POINT('Ctrl Pts',(-0.496817235749707,1.1360717231699,2.11239853056619));
#26993=CARTESIAN_POINT('Ctrl Pts',(-0.429585892713444,0.988989109974185,
2.10454797952851));
#26994=CARTESIAN_POINT('Ctrl Pts',(-0.515186036985696,0.851781234675702,
2.09669742849084));
#26995=CARTESIAN_POINT('Ctrl Pts',(-0.67684923284346,0.847499648733552,
2.08884687745316));
#26996=CARTESIAN_POINT('Ctrl Pts',(-0.769592458789038,0.979983655714312,
2.08099632641548));
#26997=CARTESIAN_POINT('Ctrl Pts',(-0.710240646482644,1.1304194790008,2.0731457753778));
#26998=CARTESIAN_POINT('Ctrl Pts',(-0.552023363069014,1.16389067130903,
2.06529522434013));
#26999=CARTESIAN_POINT('Ctrl Pts',(-0.436830779225235,1.05038344926453,
2.05744467330245));
#27000=CARTESIAN_POINT('Ctrl Pts',(-0.467975943016225,0.891685973282426,
2.04959412226477));
#27001=CARTESIAN_POINT('Ctrl Pts',(-0.617516128195625,0.830137266366705,
2.04174357122709));
#27002=CARTESIAN_POINT('Ctrl Pts',(-0.751361759160267,0.920905505868468,
2.03389302018941));
#27003=CARTESIAN_POINT('Ctrl Pts',(-0.749434417417234,1.08264685459083,
2.02604246915173));
#27004=CARTESIAN_POINT('Ctrl Pts',(-0.613546069870597,1.17019124489367,
2.01819191811406));
#27005=CARTESIAN_POINT('Ctrl Pts',(-0.465400250310609,1.10525715548948,
2.01034136707638));
#27006=CARTESIAN_POINT('Ctrl Pts',(-0.438184538961436,0.945611677663771,
2.0024908160387));
#27007=CARTESIAN_POINT('Ctrl Pts',(-0.516476448777932,0.872219838026411,
1.99725711534692));
#27008=CARTESIAN_POINT('Ctrl Pts',(-0.56254624175848,0.859903427576914,
1.99464026500102));
#27009=CARTESIAN_POINT('Ctrl Pts',(-0.483086340557485,1.10069600903591,
2.41607920499693));
#27010=CARTESIAN_POINT('Ctrl Pts',(-0.449973151490718,1.0622497573257,2.41346235465104));
#27011=CARTESIAN_POINT('Ctrl Pts',(-0.42515130434576,0.950798154359666,
2.40822865395925));
#27012=CARTESIAN_POINT('Ctrl Pts',(-0.54478524831763,0.826780024693742,
2.40037810292158));
#27013=CARTESIAN_POINT('Ctrl Pts',(-0.71394018522848,0.858516547958849,
2.3925275518839));
#27014=CARTESIAN_POINT('Ctrl Pts',(-0.780906780829043,1.01693886792356,
2.38467700084622));
#27015=CARTESIAN_POINT('Ctrl Pts',(-0.685634174422424,1.16027112587027,
2.37682644980854));
#27016=CARTESIAN_POINT('Ctrl Pts',(-0.513561613772921,1.15981701793772,
2.36897589877087));
#27017=CARTESIAN_POINT('Ctrl Pts',(-0.419009660745144,1.01606137072615,
2.36112534773318));
#27018=CARTESIAN_POINT('Ctrl Pts',(-0.486773837186857,0.857888188850051,
2.35327479669551));
#27019=CARTESIAN_POINT('Ctrl Pts',(-0.656082085820325,0.827171035125292,
2.34542424565783));
#27020=CARTESIAN_POINT('Ctrl Pts',(-0.775094506405975,0.951447556274721,
2.33757369462015));
#27021=CARTESIAN_POINT('Ctrl Pts',(-0.737078051838477,1.11926881902364,
2.32972314358247));
#27022=CARTESIAN_POINT('Ctrl Pts',(-0.576126720758545,1.18012607574093,
2.3218725925448));
#27023=CARTESIAN_POINT('Ctrl Pts',(-0.436585524633584,1.079442440351,2.31402204150712));
#27024=CARTESIAN_POINT('Ctrl Pts',(-0.443598309590693,0.907512704295987,
2.30617149046944));
#27025=CARTESIAN_POINT('Ctrl Pts',(-0.59087585148424,0.818527891629664,
2.29832093943176));
#27026=CARTESIAN_POINT('Ctrl Pts',(-0.746336145286304,0.892291520022432,
2.29047038839408));
#27027=CARTESIAN_POINT('Ctrl Pts',(-0.77055870576274,1.06265070441055,2.28261983735641));
#27028=CARTESIAN_POINT('Ctrl Pts',(-0.641820163748749,1.17682323210921,
2.27476928631873));
#27029=CARTESIAN_POINT('Ctrl Pts',(-0.47557630485125,1.13241648942973,2.26691873528105));
#27030=CARTESIAN_POINT('Ctrl Pts',(-0.420918573673669,0.969255486982105,
2.25906818424337));
#27031=CARTESIAN_POINT('Ctrl Pts',(-0.526865323090207,0.833666896767115,
2.2512176332057));
#27032=CARTESIAN_POINT('Ctrl Pts',(-0.698400989412974,0.847249786831145,
2.24336708216802));
#27033=CARTESIAN_POINT('Ctrl Pts',(-0.781688309092209,0.997822700025263,
2.23551653113034));
#27034=CARTESIAN_POINT('Ctrl Pts',(-0.702033233780365,1.15034826732694,
2.22766598009266));
#27035=CARTESIAN_POINT('Ctrl Pts',(-0.530872328713473,1.16803793430571,
2.21981542905499));
#27036=CARTESIAN_POINT('Ctrl Pts',(-0.421706762676398,1.0350271868484,2.2119648780173));
#27037=CARTESIAN_POINT('Ctrl Pts',(-0.472438810540477,0.870603225552124,
2.20411432697963));
#27038=CARTESIAN_POINT('Ctrl Pts',(-0.637570765725878,0.822225367765818,
2.19626377594195));
#27039=CARTESIAN_POINT('Ctrl Pts',(-0.769008364973917,0.933280026583224,
2.18841322490427));
#27040=CARTESIAN_POINT('Ctrl Pts',(-0.748875244649484,1.10417074362085,
2.18056267386659));
#27041=CARTESIAN_POINT('Ctrl Pts',(-0.595227265459685,1.1816386614837,2.17271212282892));
#27042=CARTESIAN_POINT('Ctrl Pts',(-0.445859588380167,1.09620870908317,
2.16486157179124));
#27043=CARTESIAN_POINT('Ctrl Pts',(-0.434728696312199,0.924496499994273,
2.15701102075356));
#27044=CARTESIAN_POINT('Ctrl Pts',(-0.571817039685625,0.820497623037239,
2.14916046971588));
#27045=CARTESIAN_POINT('Ctrl Pts',(-0.734180529534971,0.877480748438312,
2.14130991867821));
#27046=CARTESIAN_POINT('Ctrl Pts',(-0.776207735146129,1.04434204493786,
2.13345936764052));
#27047=CARTESIAN_POINT('Ctrl Pts',(-0.660207645725328,1.17143635399922,
2.12560881660285));
#27048=CARTESIAN_POINT('Ctrl Pts',(-0.490211926051119,1.14478244030651,
2.11775826556517));
#27049=CARTESIAN_POINT('Ctrl Pts',(-0.418676726208604,0.988284240908056,
2.10990771452749));
#27050=CARTESIAN_POINT('Ctrl Pts',(-0.509756617677689,0.842292916978238,
2.10205716348981));
#27051=CARTESIAN_POINT('Ctrl Pts',(-0.681768784928714,0.837737242612945,
2.09420661245213));
#27052=CARTESIAN_POINT('Ctrl Pts',(-0.780449026947353,0.978702296816814,
2.08635606141446));
#27053=CARTESIAN_POINT('Ctrl Pts',(-0.717297770961535,1.13876836416382,
2.07850551037678));
#27054=CARTESIAN_POINT('Ctrl Pts',(-0.548952108412014,1.17438223594748,
2.0706549593391));
#27055=CARTESIAN_POINT('Ctrl Pts',(-0.426385398697532,1.05360877753029,
2.06280440830142));
#27056=CARTESIAN_POINT('Ctrl Pts',(-0.459524339782119,0.884752182582313,
2.05495385726375));
#27057=CARTESIAN_POINT('Ctrl Pts',(-0.618637434184013,0.819263396393857,
2.04710330622607));
#27058=CARTESIAN_POINT('Ctrl Pts',(-0.761051277589445,0.915842221966472,
2.03925275518839));
#27059=CARTESIAN_POINT('Ctrl Pts',(-0.759000555849758,1.08793754508699,
2.03140220415071));
#27060=CARTESIAN_POINT('Ctrl Pts',(-0.614413230072635,1.18108614472194,
2.02355165311304));
#27061=CARTESIAN_POINT('Ctrl Pts',(-0.456783762484268,1.11199525865091,
2.01570110207535));
#27062=CARTESIAN_POINT('Ctrl Pts',(-0.427825820216639,0.942129974923708,
2.00785055103768));
#27063=CARTESIAN_POINT('Ctrl Pts',(-0.511129635994264,0.864039910406679,
2.00261685034589));
#27064=CARTESIAN_POINT('Ctrl Pts',(-0.560148615814275,0.850935057178149,
2.));
#27065=CARTESIAN_POINT('Ctrl Pts',(-0.560148615814275,0.850935057178149,
2.));
#27066=CARTESIAN_POINT('Ctrl Pts',(-0.550119441743087,0.85459967610481,
2.));
#27067=CARTESIAN_POINT('Ctrl Pts',(-0.540564999899567,0.859362631836586,
2.));
#27068=CARTESIAN_POINT('Ctrl Pts',(-0.531596825272739,0.86507409197529,
2.));
#27069=CARTESIAN_POINT('Ctrl Pts',(-0.527131635014649,0.867917787290334,
2.));
#27070=CARTESIAN_POINT('Ctrl Pts',(-0.522812202969371,0.870997335784893,
2.));
#27071=CARTESIAN_POINT('Ctrl Pts',(-0.518655551555349,0.874297548143145,
2.));
#27072=CARTESIAN_POINT('Ctrl Pts',(-0.515850210886717,0.876524874666724,
2.));
#27073=CARTESIAN_POINT('Ctrl Pts',(-0.51311906464033,0.878852752659134,
2.));
#27074=CARTESIAN_POINT('Ctrl Pts',(-0.510468070497139,0.881276854651557,
2.));
#27075=CARTESIAN_POINT('Ctrl Pts',(-0.508096882944962,0.883445098019579,
2.));
#27076=CARTESIAN_POINT('Ctrl Pts',(-0.505796523707934,0.885684247113283,
2.));
#27077=CARTESIAN_POINT('Ctrl Pts',(-0.503571407093493,0.887989067169883,
2.));
#27078=CARTESIAN_POINT('Ctrl Pts',(-0.496344337828248,0.895475009293033,
2.));
#27079=CARTESIAN_POINT('Ctrl Pts',(-0.489902887206981,0.90365635994166,
2.));
#27080=CARTESIAN_POINT('Ctrl Pts',(-0.4843803033401,0.912413093858066,2.));
#27081=CARTESIAN_POINT('Ctrl Pts',(-0.482085852075076,0.91605122769112,
2.));
#27082=CARTESIAN_POINT('Ctrl Pts',(-0.479950567463666,0.919788922535331,
2.));
#27083=CARTESIAN_POINT('Ctrl Pts',(-0.477986666560954,0.923618208076587,
2.));
#27084=CARTESIAN_POINT('Ctrl Pts',(-0.47650289740366,0.926511315245457,
2.));
#27085=CARTESIAN_POINT('Ctrl Pts',(-0.475117210175375,0.929457020402162,
2.));
#27086=CARTESIAN_POINT('Ctrl Pts',(-0.473840374763333,0.932438174193855,
2.));
#27087=CARTESIAN_POINT('Ctrl Pts',(-0.470678071962382,0.939821514988315,
2.));
#27088=CARTESIAN_POINT('Ctrl Pts',(-0.468171074744705,0.947441922900028,
2.));
#27089=CARTESIAN_POINT('Ctrl Pts',(-0.466390213028648,0.95524361805541,
2.));
#27090=CARTESIAN_POINT('Ctrl Pts',(-0.464752059680358,0.962420128688376,
2.));
#27091=CARTESIAN_POINT('Ctrl Pts',(-0.463728780577517,0.969750541677906,
2.));
#27092=CARTESIAN_POINT('Ctrl Pts',(-0.463308983993722,0.977159407672611,
2.));
#27093=CARTESIAN_POINT('Ctrl Pts',(-0.46313283978449,0.9802681248283,2.));
#27094=CARTESIAN_POINT('Ctrl Pts',(-0.463063521137214,0.983387155046876,
2.));
#27095=CARTESIAN_POINT('Ctrl Pts',(-0.463099420187341,0.986501027428933,
2.));
#27096=CARTESIAN_POINT('Ctrl Pts',(-0.463196744049792,0.994942868824082,
2.));
#27097=CARTESIAN_POINT('Ctrl Pts',(-0.464064111260558,1.00336874731576,
2.));
#27098=CARTESIAN_POINT('Ctrl Pts',(-0.465675457037548,1.01166504030789,
2.));
#27099=CARTESIAN_POINT('Ctrl Pts',(-0.466871286975471,1.01782197799031,
2.));
#27100=CARTESIAN_POINT('Ctrl Pts',(-0.468477483228933,1.02390757245997,
2.));
#27101=CARTESIAN_POINT('Ctrl Pts',(-0.47049180892072,1.02987016754483,2.));
#27102=CARTESIAN_POINT('Ctrl Pts',(-0.471677004317114,1.03337845832122,
2.));
#27103=CARTESIAN_POINT('Ctrl Pts',(-0.473001297362186,1.03683670978256,
2.));
#27104=CARTESIAN_POINT('Ctrl Pts',(-0.474460925722079,1.04022912201569,
2.));
#27105=CARTESIAN_POINT('Ctrl Pts',(-0.476751357662528,1.04555245605566,
2.));
#27106=CARTESIAN_POINT('Ctrl Pts',(-0.479376312983413,1.05071850549913,
2.));
#27107=CARTESIAN_POINT('Ctrl Pts',(-0.482333055615295,1.05568494193306,
2.));
#27108=CARTESIAN_POINT('Ctrl Pts',(-0.484374509820886,1.05911396968661,
2.));
#27109=CARTESIAN_POINT('Ctrl Pts',(-0.486574680171624,1.06244757845398,
2.));
#27110=CARTESIAN_POINT('Ctrl Pts',(-0.488924280031899,1.0656592034053,2.));
#27111=CARTESIAN_POINT('Ctrl Pts',(-0.492216707647991,1.07015956232216,
2.));
#27112=CARTESIAN_POINT('Ctrl Pts',(-0.495805970213506,1.07442716727356,
2.));
#27113=CARTESIAN_POINT('Ctrl Pts',(-0.499690940637682,1.07842077494232,
2.));
#27114=CARTESIAN_POINT('Ctrl Pts',(-0.501092717011139,1.07986174984398,
2.));
#27115=CARTESIAN_POINT('Ctrl Pts',(-0.502533033199793,1.08126699098065,
2.));
#27116=CARTESIAN_POINT('Ctrl Pts',(-0.504010174669742,1.08263575197434,
2.));
#27117=CARTESIAN_POINT('Ctrl Pts',(-0.504188384727764,1.08252112989365,
2.4));
#27118=CARTESIAN_POINT('Ctrl Pts',(-0.497506954663502,1.07628156217526,
2.4));
#27119=CARTESIAN_POINT('Ctrl Pts',(-0.491604269963233,1.06931033894935,
2.4));
#27120=CARTESIAN_POINT('Ctrl Pts',(-0.48648731081533,1.06178682142811,2.4));
#27121=CARTESIAN_POINT('Ctrl Pts',(-0.482497621478512,1.05592074027282,
2.4));
#27122=CARTESIAN_POINT('Ctrl Pts',(-0.478985885254584,1.04971755224006,
2.4));
#27123=CARTESIAN_POINT('Ctrl Pts',(-0.475968008505373,1.04324617240972,
2.4));
#27124=CARTESIAN_POINT('Ctrl Pts',(-0.474670784833122,1.04046447262352,
2.4));
#27125=CARTESIAN_POINT('Ctrl Pts',(-0.473467326409776,1.03763771123602,
2.4));
#27126=CARTESIAN_POINT('Ctrl Pts',(-0.472361166010358,1.03477908326479,
2.4));
#27127=CARTESIAN_POINT('Ctrl Pts',(-0.46880698586937,1.02559408733548,2.4));
#27128=CARTESIAN_POINT('Ctrl Pts',(-0.466243719906724,1.01606060675579,
2.4));
#27129=CARTESIAN_POINT('Ctrl Pts',(-0.464705314070165,1.00636042835626,
2.4));
#27130=CARTESIAN_POINT('Ctrl Pts',(-0.463992227392452,1.00186417137142,
2.4));
#27131=CARTESIAN_POINT('Ctrl Pts',(-0.463499928942431,0.997331640290426,
2.4));
#27132=CARTESIAN_POINT('Ctrl Pts',(-0.463235268916811,0.992779403524773,
2.4));
#27133=CARTESIAN_POINT('Ctrl Pts',(-0.463040851274643,0.989435358134849,
2.4));
#27134=CARTESIAN_POINT('Ctrl Pts',(-0.462969940004504,0.986088143884579,
2.4));
#27135=CARTESIAN_POINT('Ctrl Pts',(-0.463023793901296,0.982751466845985,
2.4));
#27136=CARTESIAN_POINT('Ctrl Pts',(-0.463137062422501,0.975733581485534,
2.4));
#27137=CARTESIAN_POINT('Ctrl Pts',(-0.463800894161501,0.968753185610107,
2.4));
#27138=CARTESIAN_POINT('Ctrl Pts',(-0.465031332332612,0.96187163776825,
2.4));
#27139=CARTESIAN_POINT('Ctrl Pts',(-0.466389645164331,0.954274917384296,
2.4));
#27140=CARTESIAN_POINT('Ctrl Pts',(-0.468438000905081,0.946798204321114,
2.4));
#27141=CARTESIAN_POINT('Ctrl Pts',(-0.471116528460654,0.93949859713407,
2.4));
#27142=CARTESIAN_POINT('Ctrl Pts',(-0.472251134057494,0.936406534425243,
2.4));
#27143=CARTESIAN_POINT('Ctrl Pts',(-0.473496260389133,0.933354194164882,
2.4));
#27144=CARTESIAN_POINT('Ctrl Pts',(-0.474844488633202,0.930349739998837,
2.4));
#27145=CARTESIAN_POINT('Ctrl Pts',(-0.478666411965482,0.9218327893056,2.4));
#27146=CARTESIAN_POINT('Ctrl Pts',(-0.4833179823867,0.913689872025069,2.4));
#27147=CARTESIAN_POINT('Ctrl Pts',(-0.488689869589499,0.906016299690457,
2.4));
#27148=CARTESIAN_POINT('Ctrl Pts',(-0.491565626713204,0.901908370861642,
2.4));
#27149=CARTESIAN_POINT('Ctrl Pts',(-0.494648453197326,0.897935009702848,
2.4));
#27150=CARTESIAN_POINT('Ctrl Pts',(-0.497925430586844,0.894112166139119,
2.4));
#27151=CARTESIAN_POINT('Ctrl Pts',(-0.500336511660046,0.89129945653917,
2.4));
#27152=CARTESIAN_POINT('Ctrl Pts',(-0.502853434868661,0.888568042774596,
2.4));
#27153=CARTESIAN_POINT('Ctrl Pts',(-0.505459753140441,0.885935602377086,
2.4));
#27154=CARTESIAN_POINT('Ctrl Pts',(-0.510032980818731,0.881316538996496,
2.4));
#27155=CARTESIAN_POINT('Ctrl Pts',(-0.514888373574847,0.876993017632294,
2.4));
#27156=CARTESIAN_POINT('Ctrl Pts',(-0.519995790255463,0.872997627556259,
2.4));
#27157=CARTESIAN_POINT('Ctrl Pts',(-0.524771384850184,0.869261812672909,
2.4));
#27158=CARTESIAN_POINT('Ctrl Pts',(-0.529772960099733,0.865810225418053,
2.4));
#27159=CARTESIAN_POINT('Ctrl Pts',(-0.534950219195867,0.86268896384257,
2.4));
#27160=CARTESIAN_POINT('Ctrl Pts',(-0.540826101062414,0.859146517163432,
2.4));
#27161=CARTESIAN_POINT('Ctrl Pts',(-0.546932707573367,0.85602468566073,
2.4));
#27162=CARTESIAN_POINT('Ctrl Pts',(-0.553238064171717,0.853364150883981,
2.4));
#27163=CARTESIAN_POINT('Ctrl Pts',(-0.555483414843566,0.852416728885673,
2.4));
#27164=CARTESIAN_POINT('Ctrl Pts',(-0.557754020887936,0.851527863380312,
2.4));
#27165=CARTESIAN_POINT('Ctrl Pts',(-0.560047768817924,0.850696978396871,
2.4));
#27166=CARTESIAN_POINT('Ctrl Pts',(-0.72640212307541,0.999893075304641,
2.31934196736194));
#27167=CARTESIAN_POINT('Ctrl Pts',(-0.726497678848041,0.988483569383442,
2.32005947478237));
#27168=CARTESIAN_POINT('Ctrl Pts',(-0.725076811113891,0.977097445695636,
2.32077698220279));
#27169=CARTESIAN_POINT('Ctrl Pts',(-0.722043530727044,0.966158450551832,
2.32149448962322));
#27170=CARTESIAN_POINT('Ctrl Pts',(-0.710980731091059,0.926262398732923,
2.32411133996911));
#27171=CARTESIAN_POINT('Ctrl Pts',(-0.678470209200682,0.892313886960735,
2.32672819031501));
#27172=CARTESIAN_POINT('Ctrl Pts',(-0.639090052986859,0.879535120476776,
2.3293450406609));
#27173=CARTESIAN_POINT('Ctrl Pts',(-0.599709896773035,0.866756353992817,
2.33196189100679));
#27174=CARTESIAN_POINT('Ctrl Pts',(-0.553460106235766,0.875147332797086,
2.33457874135268));
#27175=CARTESIAN_POINT('Ctrl Pts',(-0.52107966969358,0.900946839101611,
2.33719559169858));
#27176=CARTESIAN_POINT('Ctrl Pts',(-0.488699233151393,0.926746345406136,
2.33981244204447));
#27177=CARTESIAN_POINT('Ctrl Pts',(-0.470188150604288,0.969954379210915,
2.34242929239036));
#27178=CARTESIAN_POINT('Ctrl Pts',(-0.473846947697945,1.01119320016375,
2.34504614273626));
#27179=CARTESIAN_POINT('Ctrl Pts',(-0.477505744791602,1.05243202111659,
2.34766299308215));
#27180=CARTESIAN_POINT('Ctrl Pts',(-0.503334421526021,1.09170162921748,
2.35027984342804));
#27181=CARTESIAN_POINT('Ctrl Pts',(-0.539751217545131,1.11139845740712,
2.35289669377393));
#27182=CARTESIAN_POINT('Ctrl Pts',(-0.576168013564241,1.13109528559677,
2.35551354411982));
#27183=CARTESIAN_POINT('Ctrl Pts',(-0.623172928868043,1.13121933387517,
2.35813039446572));
#27184=CARTESIAN_POINT('Ctrl Pts',(-0.659688155022986,1.11170438240693,
2.36074724481161));
#27185=CARTESIAN_POINT('Ctrl Pts',(-0.696203381177929,1.0921894309387,2.3633640951575));
#27186=CARTESIAN_POINT('Ctrl Pts',(-0.722228918184014,1.05303547972384,
2.3659809455034));
#27187=CARTESIAN_POINT('Ctrl Pts',(-0.726095082654122,1.01182045879394,
2.36859779584929));
#27188=CARTESIAN_POINT('Ctrl Pts',(-0.726461565140266,1.00791359361693,
2.36884585302017));
#27189=CARTESIAN_POINT('Ctrl Pts',(-0.726628932956602,1.00398820854659,
2.36909391019106));
#27190=CARTESIAN_POINT('Ctrl Pts',(-0.726604172280256,1.00006079745576,
2.36934196736194));
#27191=CARTESIAN_POINT('Ctrl Pts',(-0.639851384185722,0.850935057178148,
2.4));
#27192=CARTESIAN_POINT('Ctrl Pts',(-0.688870364005733,0.864039910406677,
2.39738314965411));
#27193=CARTESIAN_POINT('Ctrl Pts',(-0.772174172732383,0.942130018479807,
2.39214944896232));
#27194=CARTESIAN_POINT('Ctrl Pts',(-0.743216243669936,1.11199523763249,
2.38429889792464));
#27195=CARTESIAN_POINT('Ctrl Pts',(-0.585586769094172,1.18108616109394,
2.37644834688697));
#27196=CARTESIAN_POINT('Ctrl Pts',(-0.44099944093888,1.08793753892263,2.36859779584929));
#27197=CARTESIAN_POINT('Ctrl Pts',(-0.438948720197302,0.915842224941729,
2.36074724481161));
#27198=CARTESIAN_POINT('Ctrl Pts',(-0.581362564989717,0.819263390701727,
2.35289669377393));
#27199=CARTESIAN_POINT('Ctrl Pts',(-0.740475663026546,0.88475218199663,
2.34504614273626));
#27200=CARTESIAN_POINT('Ctrl Pts',(-0.773614604105453,1.05360877766967,
2.33719559169858));
#27201=CARTESIAN_POINT('Ctrl Pts',(-0.651047892623131,1.17438223943631,
2.3293450406609));
#27202=CARTESIAN_POINT('Ctrl Pts',(-0.48270222690289,1.13876836634555,2.32149448962322));
#27203=CARTESIAN_POINT('Ctrl Pts',(-0.419550969949932,0.978702296577685,
2.31364393858554));
#27204=CARTESIAN_POINT('Ctrl Pts',(-0.518231213613428,0.837737239705173,
2.30579338754787));
#27205=CARTESIAN_POINT('Ctrl Pts',(-0.690243383915708,0.842292914261777,
2.29794283651019));
#27206=CARTESIAN_POINT('Ctrl Pts',(-0.781323276950512,0.988284240682119,
2.29009228547251));
#27207=CARTESIAN_POINT('Ctrl Pts',(-0.709788075872465,1.14478244284782,
2.28224173443483));
#27208=CARTESIAN_POINT('Ctrl Pts',(-0.539792353219763,1.17143635698873,
2.27439118339715));
#27209=CARTESIAN_POINT('Ctrl Pts',(-0.423792261776434,1.04434204571596,
2.26654063235948));
#27210=CARTESIAN_POINT('Ctrl Pts',(-0.465819468119529,0.877480746295693,
2.2586900813218));
#27211=CARTESIAN_POINT('Ctrl Pts',(-0.6281829608073,0.820497619901593,2.25083953028412));
#27212=CARTESIAN_POINT('Ctrl Pts',(-0.765271306575456,0.924496498674441,
2.24298897924644));
#27213=CARTESIAN_POINT('Ctrl Pts',(-0.754140414313383,1.09620871076456,
2.23513842820876));
#27214=CARTESIAN_POINT('Ctrl Pts',(-0.604772734623643,1.18163866465747,
2.22728787717109));
#27215=CARTESIAN_POINT('Ctrl Pts',(-0.451124752749149,1.10417074544119,
2.21943732613341));
#27216=CARTESIAN_POINT('Ctrl Pts',(-0.43099163207285,0.933280025417337,
2.21158677509573));
#27217=CARTESIAN_POINT('Ctrl Pts',(-0.562429233617627,0.822225364659454,
2.20373622405805));
#27218=CARTESIAN_POINT('Ctrl Pts',(-0.727561191688486,0.870603223291056,
2.19588567302038));
#27219=CARTESIAN_POINT('Ctrl Pts',(-0.778293240439059,1.03502718746047,
2.1880351219827));
#27220=CARTESIAN_POINT('Ctrl Pts',(-0.669127672494447,1.16803793724193,
2.18018457094502));
#27221=CARTESIAN_POINT('Ctrl Pts',(-0.497966764436741,1.15034826995414,
2.17233401990734));
#27222=CARTESIAN_POINT('Ctrl Pts',(-0.418311687733005,0.997822699987136,
2.16448346886966));
#27223=CARTESIAN_POINT('Ctrl Pts',(-0.501599008867606,0.847249784162188,
2.15663291783199));
#27224=CARTESIAN_POINT('Ctrl Pts',(-0.673134678187691,0.833666893860354,
2.1487823667943));
#27225=CARTESIAN_POINT('Ctrl Pts',(-0.779081429455625,0.969255486445431,
2.14093181575663));
#27226=CARTESIAN_POINT('Ctrl Pts',(-0.724423697322763,1.1324164917425,2.13308126471895));
#27227=CARTESIAN_POINT('Ctrl Pts',(-0.558179835520779,1.17682323520091,
2.12523071368127));
#27228=CARTESIAN_POINT('Ctrl Pts',(-0.429441291256411,1.0626507055017,2.1173801626436));
#27229=CARTESIAN_POINT('Ctrl Pts',(-0.453663852157743,0.892291518147041,
2.10952961160592));
#27230=CARTESIAN_POINT('Ctrl Pts',(-0.609124148673025,0.818527888446316,
2.10167906056824));
#27231=CARTESIAN_POINT('Ctrl Pts',(-0.756401693146515,0.907512702702641,
2.09382850953056));
#27232=CARTESIAN_POINT('Ctrl Pts',(-0.763414478213392,1.07944244169741,
2.08597795849288));
#27233=CARTESIAN_POINT('Ctrl Pts',(-0.623873279675432,1.18012607896462,
2.0781274074552));
#27234=CARTESIAN_POINT('Ctrl Pts',(-0.462921945732953,1.11926882096942,
2.07027685641753));
#27235=CARTESIAN_POINT('Ctrl Pts',(-0.424905490600427,0.951447555675582,
2.06242630537985));
#27236=CARTESIAN_POINT('Ctrl Pts',(-0.54391791306908,0.827171031659744,
2.05457575434217));
#27237=CARTESIAN_POINT('Ctrl Pts',(-0.713226165050295,0.857888187155562,
2.04672520330449));
#27238=CARTESIAN_POINT('Ctrl Pts',(-0.780990341905239,1.01606136962747,
2.03887465226682));
#27239=CARTESIAN_POINT('Ctrl Pts',(-0.686438388751686,1.15981702310584,
2.03102410122914));
#27240=CARTESIAN_POINT('Ctrl Pts',(-0.514365822072695,1.16027112465931,
2.02317355019146));
#27241=CARTESIAN_POINT('Ctrl Pts',(-0.41909321999119,1.01693887482571,2.01532299915378));
#27242=CARTESIAN_POINT('Ctrl Pts',(-0.486059804858393,0.858516534902566,
2.0074724481161));
#27243=CARTESIAN_POINT('Ctrl Pts',(-0.655214768609463,0.826780038590561,
1.99962189707843));
#27244=CARTESIAN_POINT('Ctrl Pts',(-0.774848665287453,0.950798122348591,
1.99177134604075));
#27245=CARTESIAN_POINT('Ctrl Pts',(-0.750026848509283,1.0622497573257,1.98653764534896));
#27246=CARTESIAN_POINT('Ctrl Pts',(-0.716913659442517,1.10069600903591,
1.98392079500307));
#27247=CARTESIAN_POINT('Ctrl Pts',(-0.637453758241517,0.859903427576914,
2.40535973499898));
#27248=CARTESIAN_POINT('Ctrl Pts',(-0.683523551222066,0.872219838026409,
2.40274288465309));
#27249=CARTESIAN_POINT('Ctrl Pts',(-0.761815454411802,0.945611718599352,
2.3975091839613));
#27250=CARTESIAN_POINT('Ctrl Pts',(-0.734599755473333,1.10525713573561,
2.38965863292362));
#27251=CARTESIAN_POINT('Ctrl Pts',(-0.586453929346337,1.17019126028066,
2.38180808188594));
#27252=CARTESIAN_POINT('Ctrl Pts',(-0.450565579564614,1.08264684879734,
2.37395753084827));
#27253=CARTESIAN_POINT('Ctrl Pts',(-0.448638238759637,0.920905508664721,
2.36610697981058));
#27254=CARTESIAN_POINT('Ctrl Pts',(-0.582483871027817,0.830137261017037,
2.35825642877291));
#27255=CARTESIAN_POINT('Ctrl Pts',(-0.732024059623459,0.891685972731981,
2.35040587773523));
#27256=CARTESIAN_POINT('Ctrl Pts',(-0.76316922340911,1.05038344939552,2.34255532669756));
#27257=CARTESIAN_POINT('Ctrl Pts',(-0.647976637903853,1.16389067458796,
2.33470477565988));
#27258=CARTESIAN_POINT('Ctrl Pts',(-0.489759351510266,1.13041948105126,
2.3268542246222));
#27259=CARTESIAN_POINT('Ctrl Pts',(-0.430407538294919,0.979983655489569,
2.31900367358452));
#27260=CARTESIAN_POINT('Ctrl Pts',(-0.523150765786394,0.847499646000726,
2.31115312254684));
#27261=CARTESIAN_POINT('Ctrl Pts',(-0.684813964511835,0.851781232122674,
2.30330257150917));
#27262=CARTESIAN_POINT('Ctrl Pts',(-0.770414110255606,0.98898910976184,
2.29545202047149));
#27263=CARTESIAN_POINT('Ctrl Pts',(-0.703182766058146,1.13607172555832,
2.28760146943381));
#27264=CARTESIAN_POINT('Ctrl Pts',(-0.543414697058237,1.16112202874907,
2.27975091839613));
#27265=CARTESIAN_POINT('Ctrl Pts',(-0.434393656266662,1.04167424279268,
2.27190036735845));
#27266=CARTESIAN_POINT('Ctrl Pts',(-0.47389233010456,0.884852017014347,
2.26404981632077));
#27267=CARTESIAN_POINT('Ctrl Pts',(-0.626487356014725,0.831297233826287,
2.2561992652831));
#27268=CARTESIAN_POINT('Ctrl Pts',(-0.755327893552931,0.929039105094654,
2.24834871424542));
#27269=CARTESIAN_POINT('Ctrl Pts',(-0.744866682322397,1.0904203923485,2.24049816320774));
#27270=CARTESIAN_POINT('Ctrl Pts',(-0.604485586947538,1.17071052291906,
2.23264761217006));
#27271=CARTESIAN_POINT('Ctrl Pts',(-0.460081710268994,1.09790339771914,
2.22479706113239));
#27272=CARTESIAN_POINT('Ctrl Pts',(-0.441159882335912,0.937294178133102,
2.21694651009471));
#27273=CARTESIAN_POINT('Ctrl Pts',(-0.564689648056489,0.832921030233517,
2.20909595905703));
#27274=CARTESIAN_POINT('Ctrl Pts',(-0.719886576893662,0.878388274557731,
2.20124540801935));
#27275=CARTESIAN_POINT('Ctrl Pts',(-0.767566373413291,1.03291980536764,
2.19339485698167));
#27276=CARTESIAN_POINT('Ctrl Pts',(-0.664968662602526,1.15792807214755,
2.185544305944));
#27277=CARTESIAN_POINT('Ctrl Pts',(-0.504105510624766,1.1413026892278,2.17769375490632));
#27278=CARTESIAN_POINT('Ctrl Pts',(-0.429242816479248,0.997953695462094,
2.16984320386864));
#27279=CARTESIAN_POINT('Ctrl Pts',(-0.50751922403943,0.856439875998617,
2.16199265283096));
#27280=CARTESIAN_POINT('Ctrl Pts',(-0.668734590074648,0.843674189185456,
2.15414210179328));
#27281=CARTESIAN_POINT('Ctrl Pts',(-0.768307141682156,0.971105204964537,
2.14629155075561));
#27282=CARTESIAN_POINT('Ctrl Pts',(-0.716937847311012,1.12444976178997,
2.13844099971793));
#27283=CARTESIAN_POINT('Ctrl Pts',(-0.560695911521528,1.16618480983832,
2.13059044868025));
#27284=CARTESIAN_POINT('Ctrl Pts',(-0.439702816507024,1.05888137703287,
2.12273989764257));
#27285=CARTESIAN_POINT('Ctrl Pts',(-0.462468046837819,0.8987717108876,2.11488934660489));
#27286=CARTESIAN_POINT('Ctrl Pts',(-0.608575201728667,0.829446009653423,
2.10703879556722));
#27287=CARTESIAN_POINT('Ctrl Pts',(-0.746991913163515,0.913077125320336,
2.09918824452953));
#27288=CARTESIAN_POINT('Ctrl Pts',(-0.753582779750997,1.07466285215048,
2.09133769349186));
#27289=CARTESIAN_POINT('Ctrl Pts',(-0.622436963324253,1.16928894070762,
2.08348714245418));
#27290=CARTESIAN_POINT('Ctrl Pts',(-0.471169134783152,1.11209310987848,
2.07563659141651));
#27291=CARTESIAN_POINT('Ctrl Pts',(-0.435439908588715,0.954368673788424,
2.06778604037882));
#27292=CARTESIAN_POINT('Ctrl Pts',(-0.547292045972571,0.837569145222665,
2.05993548934115));
#27293=CARTESIAN_POINT('Ctrl Pts',(-0.706414005411818,0.866438228174611,
2.05208493830347));
#27294=CARTESIAN_POINT('Ctrl Pts',(-0.770101205975101,1.01509505045675,
2.04423438726579));
#27295=CARTESIAN_POINT('Ctrl Pts',(-0.681237893770622,1.15020176258845,
2.03638383622811));
#27296=CARTESIAN_POINT('Ctrl Pts',(-0.519517932367091,1.15062854349327,
2.02853328519044));
#27297=CARTESIAN_POINT('Ctrl Pts',(-0.429977328488155,1.01591976127225,
2.02068273415276));
#27298=CARTESIAN_POINT('Ctrl Pts',(-0.492914923533471,0.867028771893199,
2.01283218311508));
#27299=CARTESIAN_POINT('Ctrl Pts',(-0.651892817203601,0.837201675931786,
2.0049816320774));
#27300=CARTESIAN_POINT('Ctrl Pts',(-0.764329038309151,0.95375831308653,
1.99713108103972));
#27301=CARTESIAN_POINT('Ctrl Pts',(-0.741000605841356,1.05850455157603,
1.99189738034794));
#27302=CARTESIAN_POINT('Ctrl Pts',(-0.709879644719091,1.09463771598849,
1.98928053000205));
#27303=CARTESIAN_POINT('Ctrl Pts',(-0.635056132297313,0.868871797975679,
2.41071946999795));
#27304=CARTESIAN_POINT('Ctrl Pts',(-0.678176738438398,0.880399765646142,
2.40810261965206));
#27305=CARTESIAN_POINT('Ctrl Pts',(-0.751456736091222,0.949093418718895,
2.40286891896028));
#27306=CARTESIAN_POINT('Ctrl Pts',(-0.725983267276729,1.09851903383873,
2.3950183679226));
#27307=CARTESIAN_POINT('Ctrl Pts',(-0.587321089598503,1.15929635946738,
2.38716781688492));
#27308=CARTESIAN_POINT('Ctrl Pts',(-0.460131718190347,1.07735615867206,
2.37931726584724));
#27309=CARTESIAN_POINT('Ctrl Pts',(-0.458327757321973,0.925968792387711,
2.37146671480957));
#27310=CARTESIAN_POINT('Ctrl Pts',(-0.583605177065917,0.841011131332347,
2.36361616377189));
#27311=CARTESIAN_POINT('Ctrl Pts',(-0.72357245622037,0.898619763467331,
2.35576561273421));
#27312=CARTESIAN_POINT('Ctrl Pts',(-0.752723842712768,1.04715812112138,
2.34791506169653));
#27313=CARTESIAN_POINT('Ctrl Pts',(-0.644905383184573,1.15339910973961,
2.34006451065885));
#27314=CARTESIAN_POINT('Ctrl Pts',(-0.496816476117644,1.12207059575698,
2.33221395962118));
#27315=CARTESIAN_POINT('Ctrl Pts',(-0.441264106639905,0.981265014401455,
2.3243634085835));
#27316=CARTESIAN_POINT('Ctrl Pts',(-0.528070317959361,0.857262052296277,
2.31651285754582));
#27317=CARTESIAN_POINT('Ctrl Pts',(-0.679384545107962,0.861269549983572,
2.30866230650814));
#27318=CARTESIAN_POINT('Ctrl Pts',(-0.759504943560701,0.989693978841561,
2.30081175547046));
#27319=CARTESIAN_POINT('Ctrl Pts',(-0.696577456243827,1.12736100826881,
2.29296120443279));
#27320=CARTESIAN_POINT('Ctrl Pts',(-0.547037040896711,1.15080770050942,
2.28511065339511));
#27321=CARTESIAN_POINT('Ctrl Pts',(-0.444995050756889,1.03900643986939,
2.27726010235743));
#27322=CARTESIAN_POINT('Ctrl Pts',(-0.481965192089592,0.892223287733,2.26940955131975));
#27323=CARTESIAN_POINT('Ctrl Pts',(-0.624791751222149,0.842096847750981,
2.26155900028208));
#27324=CARTESIAN_POINT('Ctrl Pts',(-0.745384480530408,0.933581711514867,
2.2537084492444));
#27325=CARTESIAN_POINT('Ctrl Pts',(-0.735592950331409,1.08463207393244,
2.24585789820672));
#27326=CARTESIAN_POINT('Ctrl Pts',(-0.604198439271435,1.15978238118065,
2.23800734716904));
#27327=CARTESIAN_POINT('Ctrl Pts',(-0.469038667788838,1.09163604999709,
2.23015679613136));
#27328=CARTESIAN_POINT('Ctrl Pts',(-0.451328132598973,0.941308330848865,
2.22230624509368));
#27329=CARTESIAN_POINT('Ctrl Pts',(-0.56695006249535,0.843616695807582,
2.21445569405601));
#27330=CARTESIAN_POINT('Ctrl Pts',(-0.712211962098838,0.886173325824406,
2.20660514301833));
#27331=CARTESIAN_POINT('Ctrl Pts',(-0.756839506387522,1.0308124232748,2.19875459198065));
#27332=CARTESIAN_POINT('Ctrl Pts',(-0.660809652710606,1.14781820705317,
2.19090404094297));
#27333=CARTESIAN_POINT('Ctrl Pts',(-0.51024425681279,1.13225710850146,2.1830534899053));
#27334=CARTESIAN_POINT('Ctrl Pts',(-0.440173945225492,0.998084690937051,
2.17520293886762));
#27335=CARTESIAN_POINT('Ctrl Pts',(-0.513439439211253,0.865629967835047,
2.16735238782994));
#27336=CARTESIAN_POINT('Ctrl Pts',(-0.664334501961606,0.853681484510555,
2.15950183679226));
#27337=CARTESIAN_POINT('Ctrl Pts',(-0.757532853908686,0.972954923483646,
2.15165128575458));
#27338=CARTESIAN_POINT('Ctrl Pts',(-0.709451997299263,1.11648303183743,
2.1438007347169));
#27339=CARTESIAN_POINT('Ctrl Pts',(-0.563211987522275,1.15554638447572,
2.13595018367923));
#27340=CARTESIAN_POINT('Ctrl Pts',(-0.449964341757637,1.05511204856404,
2.12809963264155));
#27341=CARTESIAN_POINT('Ctrl Pts',(-0.471272241517894,0.905251903628159,
2.12024908160387));
#27342=CARTESIAN_POINT('Ctrl Pts',(-0.608026254784307,0.840364130860531,
2.11239853056619));
#27343=CARTESIAN_POINT('Ctrl Pts',(-0.737582133180516,0.918641547938033,
2.10454797952851));
#27344=CARTESIAN_POINT('Ctrl Pts',(-0.7437510812886,1.06988326260355,2.09669742849084));
#27345=CARTESIAN_POINT('Ctrl Pts',(-0.621000646973074,1.15845180245062,
2.08884687745316));
#27346=CARTESIAN_POINT('Ctrl Pts',(-0.479416323833351,1.10491739878753,
2.08099632641548));
#27347=CARTESIAN_POINT('Ctrl Pts',(-0.445974326577002,0.957289791901268,
2.0731457753778));
#27348=CARTESIAN_POINT('Ctrl Pts',(-0.550666178876061,0.847967258785586,
2.06529522434013));
#27349=CARTESIAN_POINT('Ctrl Pts',(-0.699601845773343,0.87498826919366,
2.05744467330245));
#27350=CARTESIAN_POINT('Ctrl Pts',(-0.759212070044963,1.01412873128603,
2.04959412226477));
#27351=CARTESIAN_POINT('Ctrl Pts',(-0.676037398789558,1.14058650207107,
2.04174357122709));
#27352=CARTESIAN_POINT('Ctrl Pts',(-0.524670042661485,1.14098596232722,
2.03389302018941));
#27353=CARTESIAN_POINT('Ctrl Pts',(-0.440861436985121,1.01490064771879,
2.02604246915174));
#27354=CARTESIAN_POINT('Ctrl Pts',(-0.49977004220855,0.875541008883831,
2.01819191811406));
#27355=CARTESIAN_POINT('Ctrl Pts',(-0.648570865797738,0.847623313273011,
2.01034136707638));
#27356=CARTESIAN_POINT('Ctrl Pts',(-0.753809411330851,0.956718503824468,
2.0024908160387));
#27357=CARTESIAN_POINT('Ctrl Pts',(-0.731974363173429,1.05475934582637,
1.99725711534692));
#27358=CARTESIAN_POINT('Ctrl Pts',(-0.702845629995664,1.08857942294107,
1.99464026500102));
#27359=CARTESIAN_POINT('Ctrl Pts',(-0.632658506353108,0.877840168374445,
2.41607920499693));
#27360=CARTESIAN_POINT('Ctrl Pts',(-0.672829925654731,0.888579693265874,
2.41346235465104));
#27361=CARTESIAN_POINT('Ctrl Pts',(-0.74109801777064,0.952575118838442,
2.40822865395925));
#27362=CARTESIAN_POINT('Ctrl Pts',(-0.717366779080126,1.09178093194185,
2.40037810292158));
#27363=CARTESIAN_POINT('Ctrl Pts',(-0.588188249850668,1.1484014586541,2.3925275518839));
#27364=CARTESIAN_POINT('Ctrl Pts',(-0.469697856816082,1.07206546854677,
2.38467700084622));
#27365=CARTESIAN_POINT('Ctrl Pts',(-0.468017275884308,0.931032076110704,
2.37682644980854));
#27366=CARTESIAN_POINT('Ctrl Pts',(-0.584726483104016,0.851885001647656,
2.36897589877086));
#27367=CARTESIAN_POINT('Ctrl Pts',(-0.715120852817283,0.905553554202683,
2.36112534773319));
#27368=CARTESIAN_POINT('Ctrl Pts',(-0.742278462016426,1.04393279284724,
2.35327479669551));
#27369=CARTESIAN_POINT('Ctrl Pts',(-0.641834128465295,1.14290754489126,
2.34542424565783));
#27370=CARTESIAN_POINT('Ctrl Pts',(-0.50387360072502,1.1137217104627,2.33757369462015));
#27371=CARTESIAN_POINT('Ctrl Pts',(-0.452120674984892,0.98254637331334,
2.32972314358248));
#27372=CARTESIAN_POINT('Ctrl Pts',(-0.532989870132326,0.867024458591828,
2.32187259254479));
#27373=CARTESIAN_POINT('Ctrl Pts',(-0.673955125704091,0.870757867844471,
2.31402204150712));
#27374=CARTESIAN_POINT('Ctrl Pts',(-0.748595776865795,0.990398847921281,
2.30617149046944));
#27375=CARTESIAN_POINT('Ctrl Pts',(-0.689972146429509,1.11865029097931,
2.29832093943176));
#27376=CARTESIAN_POINT('Ctrl Pts',(-0.550659384735185,1.14049337226976,
2.29047038839408));
#27377=CARTESIAN_POINT('Ctrl Pts',(-0.455596445247116,1.0363386369461,2.28261983735641));
#27378=CARTESIAN_POINT('Ctrl Pts',(-0.490038054074624,0.899594558451655,
2.27476928631873));
#27379=CARTESIAN_POINT('Ctrl Pts',(-0.623096146429573,0.852896461675674,
2.26691873528105));
#27380=CARTESIAN_POINT('Ctrl Pts',(-0.735441067507883,0.938124317935081,
2.25906818424337));
#27381=CARTESIAN_POINT('Ctrl Pts',(-0.726319218340423,1.07884375551639,
2.25121763320569));
#27382=CARTESIAN_POINT('Ctrl Pts',(-0.603911291595331,1.14885423944223,
2.24336708216802));
#27383=CARTESIAN_POINT('Ctrl Pts',(-0.477995625308683,1.08536870227504,
2.23551653113034));
#27384=CARTESIAN_POINT('Ctrl Pts',(-0.461496382862034,0.945322483564629,
2.22766598009266));
#27385=CARTESIAN_POINT('Ctrl Pts',(-0.569210476934212,0.854312361381646,
2.21981542905498));
#27386=CARTESIAN_POINT('Ctrl Pts',(-0.704537347304013,0.893958377091083,
2.21196487801731));
#27387=CARTESIAN_POINT('Ctrl Pts',(-0.746112639361755,1.02870504118196,
2.20411432697963));
#27388=CARTESIAN_POINT('Ctrl Pts',(-0.656650642818685,1.1377083419588,2.19626377594195));
#27389=CARTESIAN_POINT('Ctrl Pts',(-0.516383003000816,1.12321152777512,
2.18841322490427));
#27390=CARTESIAN_POINT('Ctrl Pts',(-0.451105073971734,0.998215686412011,
2.18056267386659));
#27391=CARTESIAN_POINT('Ctrl Pts',(-0.519359654383078,0.874820059671476,
2.17271212282892));
#27392=CARTESIAN_POINT('Ctrl Pts',(-0.659934413848564,0.863688779835656,
2.16486157179123));
#27393=CARTESIAN_POINT('Ctrl Pts',(-0.746758566135216,0.974804642002754,
2.15701102075356));
#27394=CARTESIAN_POINT('Ctrl Pts',(-0.701966147287513,1.1085163018849,2.14916046971588));
#27395=CARTESIAN_POINT('Ctrl Pts',(-0.565728063523024,1.14490795911313,
2.1413099186782));
#27396=CARTESIAN_POINT('Ctrl Pts',(-0.46022586700825,1.0513427200952,2.13345936764053));
#27397=CARTESIAN_POINT('Ctrl Pts',(-0.48007643619797,0.91173209636872,2.12560881660285));
#27398=CARTESIAN_POINT('Ctrl Pts',(-0.607477307839948,0.851282252067638,
2.11775826556517));
#27399=CARTESIAN_POINT('Ctrl Pts',(-0.728172353197516,0.924205970555728,
2.10990771452749));
#27400=CARTESIAN_POINT('Ctrl Pts',(-0.733919382826205,1.06510367305662,
2.10205716348981));
#27401=CARTESIAN_POINT('Ctrl Pts',(-0.619564330621895,1.14761466419362,
2.09420661245214));
#27402=CARTESIAN_POINT('Ctrl Pts',(-0.487663512883551,1.09774168769659,
2.08635606141446));
#27403=CARTESIAN_POINT('Ctrl Pts',(-0.456508744565289,0.960210910014111,
2.07850551037678));
#27404=CARTESIAN_POINT('Ctrl Pts',(-0.554040311779553,0.858365372348507,
2.0706549593391));
#27405=CARTESIAN_POINT('Ctrl Pts',(-0.692789686134866,0.883538310212708,
2.06280440830143));
#27406=CARTESIAN_POINT('Ctrl Pts',(-0.748322934114825,1.01316241211532,
2.05495385726374));
#27407=CARTESIAN_POINT('Ctrl Pts',(-0.670836903808495,1.13097124155368,
2.04710330622607));
#27408=CARTESIAN_POINT('Ctrl Pts',(-0.529822152955879,1.13134338116118,
2.03925275518839));
#27409=CARTESIAN_POINT('Ctrl Pts',(-0.451745545482087,1.01388153416533,
2.03140220415071));
#27410=CARTESIAN_POINT('Ctrl Pts',(-0.506625160883627,0.884053245874464,
2.02355165311303));
#27411=CARTESIAN_POINT('Ctrl Pts',(-0.645248914391877,0.858044950614234,
2.01570110207536));
#27412=CARTESIAN_POINT('Ctrl Pts',(-0.743289784352549,0.959678694562408,
2.00785055103768));
#27413=CARTESIAN_POINT('Ctrl Pts',(-0.722948120505502,1.0510141400767,2.00261685034589));
#27414=CARTESIAN_POINT('Ctrl Pts',(-0.695811615272238,1.08252112989365,
2.));
#27415=CARTESIAN_POINT('Ctrl Pts',(-0.695811615272238,1.08252112989365,
2.));
#27416=CARTESIAN_POINT('Ctrl Pts',(-0.702493043757975,1.07628156364939,
2.));
#27417=CARTESIAN_POINT('Ctrl Pts',(-0.708395726655653,1.06931034161853,
2.));
#27418=CARTESIAN_POINT('Ctrl Pts',(-0.713512684042454,1.06178682515746,
2.));
#27419=CARTESIAN_POINT('Ctrl Pts',(-0.717502373507965,1.05592074262065,
2.));
#27420=CARTESIAN_POINT('Ctrl Pts',(-0.721014109525759,1.04971755287119,
2.));
#27421=CARTESIAN_POINT('Ctrl Pts',(-0.724031985841351,1.04324617113496,
2.));
#27422=CARTESIAN_POINT('Ctrl Pts',(-0.72532920883522,1.04046447158453,2.));
#27423=CARTESIAN_POINT('Ctrl Pts',(-0.726532666614568,1.03763771042115,
2.));
#27424=CARTESIAN_POINT('Ctrl Pts',(-0.727638826408048,1.0347790826819,2.));
#27425=CARTESIAN_POINT('Ctrl Pts',(-0.731193005346523,1.0255940855742,2.));
#27426=CARTESIAN_POINT('Ctrl Pts',(-0.733756270098347,1.01606060371262,
2.));
#27427=CARTESIAN_POINT('Ctrl Pts',(-0.73529467500939,1.0063604242084,2.));
#27428=CARTESIAN_POINT('Ctrl Pts',(-0.736007760405585,1.00186417208695,
2.));
#27429=CARTESIAN_POINT('Ctrl Pts',(-0.736500058162718,0.997331645993815,
2.));
#27430=CARTESIAN_POINT('Ctrl Pts',(-0.736764718140032,0.992779414308968,
2.));
#27431=CARTESIAN_POINT('Ctrl Pts',(-0.736959136386439,0.989435361647935,
2.));
#27432=CARTESIAN_POINT('Ctrl Pts',(-0.737030047799371,0.986088140051384,
2.));
#27433=CARTESIAN_POINT('Ctrl Pts',(-0.736976193579456,0.982751455795261,
2.));
#27434=CARTESIAN_POINT('Ctrl Pts',(-0.73686292459887,0.975733568899372,
2.));
#27435=CARTESIAN_POINT('Ctrl Pts',(-0.736199092496592,0.968753171717965,
2.));
#27436=CARTESIAN_POINT('Ctrl Pts',(-0.734968654150234,0.961871622922131,
2.));
#27437=CARTESIAN_POINT('Ctrl Pts',(-0.733610341240648,0.954274902131536,
2.));
#27438=CARTESIAN_POINT('Ctrl Pts',(-0.731561985767923,0.946798189069373,
2.));
#27439=CARTESIAN_POINT('Ctrl Pts',(-0.728883458720402,0.939498582185105,
2.));
#27440=CARTESIAN_POINT('Ctrl Pts',(-0.727748853408495,0.936406519794552,
2.));
#27441=CARTESIAN_POINT('Ctrl Pts',(-0.726503727419379,0.933354179904992,
2.));
#27442=CARTESIAN_POINT('Ctrl Pts',(-0.725155499563838,0.930349726147835,
2.));
#27443=CARTESIAN_POINT('Ctrl Pts',(-0.721333577255107,0.921832776440231,
2.));
#27444=CARTESIAN_POINT('Ctrl Pts',(-0.716682008196949,0.913689860477865,
2.));
#27445=CARTESIAN_POINT('Ctrl Pts',(-0.711310122504209,0.906016289602163,
2.));
#27446=CARTESIAN_POINT('Ctrl Pts',(-0.708434363463016,0.901908357660524,
2.));
#27447=CARTESIAN_POINT('Ctrl Pts',(-0.705351534711708,0.897934993684464,
2.));
#27448=CARTESIAN_POINT('Ctrl Pts',(-0.702074554712817,0.894112147617013,
2.));
#27449=CARTESIAN_POINT('Ctrl Pts',(-0.699663476442214,0.891299441684046,
2.));
#27450=CARTESIAN_POINT('Ctrl Pts',(-0.69714655627776,0.888568031452597,
2.));
#27451=CARTESIAN_POINT('Ctrl Pts',(-0.694540241228364,0.885935594383534,
2.));
#27452=CARTESIAN_POINT('Ctrl Pts',(-0.68996701323731,0.881316530816482,
2.));
#27453=CARTESIAN_POINT('Ctrl Pts',(-0.685111619991385,0.87699300942471,
2.));
#27454=CARTESIAN_POINT('Ctrl Pts',(-0.680004202609246,0.872997619450478,
2.));
#27455=CARTESIAN_POINT('Ctrl Pts',(-0.67522861092298,0.869261807450647,
2.));
#27456=CARTESIAN_POINT('Ctrl Pts',(-0.670227038735164,0.865810222770729,
2.));
#27457=CARTESIAN_POINT('Ctrl Pts',(-0.66504978274748,0.862688963354369,
2.));
#27458=CARTESIAN_POINT('Ctrl Pts',(-0.659173901912074,0.859146517620461,
2.));
#27459=CARTESIAN_POINT('Ctrl Pts',(-0.653067296294555,0.856024686886556,
2.));
#27460=CARTESIAN_POINT('Ctrl Pts',(-0.64676194038029,0.853364152629858,
2.));
#27461=CARTESIAN_POINT('Ctrl Pts',(-0.644516589878667,0.85241673078578,
2.));
#27462=CARTESIAN_POINT('Ctrl Pts',(-0.642245983976318,0.851527865406908,
2.));
#27463=CARTESIAN_POINT('Ctrl Pts',(-0.639952236162157,0.850696980524378,
2.));
#27464=CARTESIAN_POINT('Ctrl Pts',(-0.726369333664333,1.00010094057762,
2.35565803263806));
#27465=CARTESIAN_POINT('Ctrl Pts',(-0.726467565903334,1.01274184217687,
2.35486362065721));
#27466=CARTESIAN_POINT('Ctrl Pts',(-0.724719482090242,1.02535623071191,
2.35406920867636));
#27467=CARTESIAN_POINT('Ctrl Pts',(-0.721011471558047,1.03736537841382,
2.35327479669551));
#27468=CARTESIAN_POINT('Ctrl Pts',(-0.708797017499383,1.07692437686191,
2.35065794634961));
#27469=CARTESIAN_POINT('Ctrl Pts',(-0.675315572982339,1.10991596087659,
2.34804109600372));
#27470=CARTESIAN_POINT('Ctrl Pts',(-0.635581429433771,1.12154744714583,
2.34542424565783));
#27471=CARTESIAN_POINT('Ctrl Pts',(-0.595847285885203,1.13317893341507,
2.34280739531194));
#27472=CARTESIAN_POINT('Ctrl Pts',(-0.549860443305111,1.12345032193889,
2.34019054496604));
#27473=CARTESIAN_POINT('Ctrl Pts',(-0.518241534391711,1.09672346000923,
2.33757369462015));
#27474=CARTESIAN_POINT('Ctrl Pts',(-0.486622625478311,1.06999659807958,
2.33495684427426));
#27475=CARTESIAN_POINT('Ctrl Pts',(-0.469371650231601,1.02627148569646,
2.33233999392837));
#27476=CARTESIAN_POINT('Ctrl Pts',(-0.474224361799485,0.985155277051315,
2.32972314358247));
#27477=CARTESIAN_POINT('Ctrl Pts',(-0.47907707336737,0.944039068406169,
2.32710629323658));
#27478=CARTESIAN_POINT('Ctrl Pts',(-0.506033471749848,0.905531763498998,
2.32448944289069));
#27479=CARTESIAN_POINT('Ctrl Pts',(-0.543005880203048,0.886900345920854,
2.3218725925448));
#27480=CARTESIAN_POINT('Ctrl Pts',(-0.579978288656248,0.868268928342709,
2.3192557421989));
#27481=CARTESIAN_POINT('Ctrl Pts',(-0.62696670718017,0.86951339809359,2.31663889185301));
#27482=CARTESIAN_POINT('Ctrl Pts',(-0.662901024969081,0.890075796315165,
2.31402204150712));
#27483=CARTESIAN_POINT('Ctrl Pts',(-0.698835342757992,0.910638194536741,
2.31140519116123));
#27484=CARTESIAN_POINT('Ctrl Pts',(-0.723715559811894,0.950518521229011,
2.30878834081533));
#27485=CARTESIAN_POINT('Ctrl Pts',(-0.72638506326613,0.991833925084817,
2.30617149046944));
#27486=CARTESIAN_POINT('Ctrl Pts',(-0.726559659603113,0.994536119817981,
2.30600033785898));
#27487=CARTESIAN_POINT('Ctrl Pts',(-0.726639245398498,0.997244453365998,
2.30582918524852));
#27488=CARTESIAN_POINT('Ctrl Pts',(-0.726626272216059,0.999953562434948,
2.30565803263806));
#27489=CARTESIAN_POINT('Ctrl Pts',(-0.639851384185722,0.850935057178148,
2.4));
#27490=CARTESIAN_POINT('Ctrl Pts',(-0.649880557039356,0.854599675659919,
2.4));
#27491=CARTESIAN_POINT('Ctrl Pts',(-0.659434997625568,0.85936263163469,
2.4));
#27492=CARTESIAN_POINT('Ctrl Pts',(-0.668403171068605,0.865074092345247,
2.4));
#27493=CARTESIAN_POINT('Ctrl Pts',(-0.672868373471587,0.86791779605496,
2.4));
#27494=CARTESIAN_POINT('Ctrl Pts',(-0.67718781684999,0.870997354370473,
2.4));
#27495=CARTESIAN_POINT('Ctrl Pts',(-0.681344478651501,0.874297577803816,
2.4));
#27496=CARTESIAN_POINT('Ctrl Pts',(-0.684149819111287,0.8765249060701,2.4));
#27497=CARTESIAN_POINT('Ctrl Pts',(-0.686880965099162,0.878852785859471,
2.4));
#27498=CARTESIAN_POINT('Ctrl Pts',(-0.689531958931665,0.88127688968642,
2.4));
#27499=CARTESIAN_POINT('Ctrl Pts',(-0.691903137355438,0.883445126602317,
2.4));
#27500=CARTESIAN_POINT('Ctrl Pts',(-0.694203487834536,0.885684268626149,
2.4));
#27501=CARTESIAN_POINT('Ctrl Pts',(-0.696428596284293,0.887989081198335,
2.4));
#27502=CARTESIAN_POINT('Ctrl Pts',(-0.703655665265446,0.895475026186606,
2.4));
#27503=CARTESIAN_POINT('Ctrl Pts',(-0.710097115492295,0.903656379805453,
2.4));
#27504=CARTESIAN_POINT('Ctrl Pts',(-0.715619698888934,0.91241311638882,
2.4));
#27505=CARTESIAN_POINT('Ctrl Pts',(-0.717914152011463,0.916051254584994,
2.4));
#27506=CARTESIAN_POINT('Ctrl Pts',(-0.720049438182606,0.919788953917886,
2.4));
#27507=CARTESIAN_POINT('Ctrl Pts',(-0.722013340315698,0.923618244020841,
2.4));
#27508=CARTESIAN_POINT('Ctrl Pts',(-0.723497106826098,0.926511347662634,
2.4));
#27509=CARTESIAN_POINT('Ctrl Pts',(-0.724882791677009,0.929457049049758,
2.4));
#27510=CARTESIAN_POINT('Ctrl Pts',(-0.726159625039968,0.932438198899027,
2.4));
#27511=CARTESIAN_POINT('Ctrl Pts',(-0.7293219265251,0.939821538706109,2.4));
#27512=CARTESIAN_POINT('Ctrl Pts',(-0.731828922840258,0.947441945091078,
2.4));
#27513=CARTESIAN_POINT('Ctrl Pts',(-0.733609784156052,0.955243638029731,
2.4));
#27514=CARTESIAN_POINT('Ctrl Pts',(-0.735247937517986,0.962420148296355,
2.4));
#27515=CARTESIAN_POINT('Ctrl Pts',(-0.736271216774028,0.969750560405923,
2.4));
#27516=CARTESIAN_POINT('Ctrl Pts',(-0.736691013623241,0.977159425155101,
2.4));
#27517=CARTESIAN_POINT('Ctrl Pts',(-0.736867157952635,0.980268141943398,
2.4));
#27518=CARTESIAN_POINT('Ctrl Pts',(-0.736936476729183,0.983387171734525,
2.4));
#27519=CARTESIAN_POINT('Ctrl Pts',(-0.736900577814768,0.986501043637764,
2.4));
#27520=CARTESIAN_POINT('Ctrl Pts',(-0.73680325432052,0.994942883710025,
2.4));
#27521=CARTESIAN_POINT('Ctrl Pts',(-0.735935887531182,1.00336876050526,
2.4));
#27522=CARTESIAN_POINT('Ctrl Pts',(-0.73432454218896,1.01166505164342,2.4));
#27523=CARTESIAN_POINT('Ctrl Pts',(-0.733128713302574,1.01782198419718,
2.4));
#27524=CARTESIAN_POINT('Ctrl Pts',(-0.731522518607655,1.02390757353733,
2.4));
#27525=CARTESIAN_POINT('Ctrl Pts',(-0.729508194962256,1.0298701636783,2.4));
#27526=CARTESIAN_POINT('Ctrl Pts',(-0.728322998806314,1.03337845735825,
2.4));
#27527=CARTESIAN_POINT('Ctrl Pts',(-0.726998704692332,1.03683671166907,
2.4));
#27528=CARTESIAN_POINT('Ctrl Pts',(-0.72553907497761,1.04022912662095,2.4));
#27529=CARTESIAN_POINT('Ctrl Pts',(-0.723248641788982,1.04555246288699,
2.4));
#27530=CARTESIAN_POINT('Ctrl Pts',(-0.720623684757818,1.05071851440316,
2.4));
#27531=CARTESIAN_POINT('Ctrl Pts',(-0.717666939943194,1.055684952745,2.4));
#27532=CARTESIAN_POINT('Ctrl Pts',(-0.715625486572472,1.05911397788213,
2.4));
#27533=CARTESIAN_POINT('Ctrl Pts',(-0.713425317203702,1.06244758415869,
2.4));
#27534=CARTESIAN_POINT('Ctrl Pts',(-0.711075718450412,1.06565920682025,
2.4));
#27535=CARTESIAN_POINT('Ctrl Pts',(-0.707783291943712,1.07015956313241,
2.4));
#27536=CARTESIAN_POINT('Ctrl Pts',(-0.704194030655052,1.07442716580257,
2.4));
#27537=CARTESIAN_POINT('Ctrl Pts',(-0.700309061659577,1.07842077162732,
2.4));
#27538=CARTESIAN_POINT('Ctrl Pts',(-0.69890728532317,1.07986174635546,2.4));
#27539=CARTESIAN_POINT('Ctrl Pts',(-0.697466969165074,1.08126698735129,
2.4));
#27540=CARTESIAN_POINT('Ctrl Pts',(-0.695989827719556,1.08263574823442,
2.4));
#27541=CARTESIAN_POINT('Origin',(0.,0.,2.));
#27542=CARTESIAN_POINT('',(-0.8,0.6,2.));
#27543=CARTESIAN_POINT('',(0.8,0.6,2.));
#27544=CARTESIAN_POINT('Origin',(0.,0.,2.));
#27545=CARTESIAN_POINT('',(-1.8,0.6,2.));
#27546=CARTESIAN_POINT('',(-1.8,0.6,2.));
#27547=CARTESIAN_POINT('',(-1.8,1.4,2.));
#27548=CARTESIAN_POINT('',(-1.8,1.4,2.));
#27549=CARTESIAN_POINT('',(1.8,1.4,2.));
#27550=CARTESIAN_POINT('',(1.8,1.4,2.));
#27551=CARTESIAN_POINT('',(1.8,0.6,2.));
#27552=CARTESIAN_POINT('',(1.8,0.6,2.));
#27553=CARTESIAN_POINT('',(-1.8,0.6,2.));
#27554=CARTESIAN_POINT('Ctrl Pts',(0.504188384727762,1.08252112989365,2.));
#27555=CARTESIAN_POINT('Ctrl Pts',(0.497506952411728,1.07628156007241,2.));
#27556=CARTESIAN_POINT('Ctrl Pts',(0.491604265140002,1.06931033514179,2.));
#27557=CARTESIAN_POINT('Ctrl Pts',(0.486487303479808,1.06178681610824,2.));
#27558=CARTESIAN_POINT('Ctrl Pts',(0.482497614326221,1.0559207369233,2.));
#27559=CARTESIAN_POINT('Ctrl Pts',(0.478985877807952,1.04971755133896,2.));
#27560=CARTESIAN_POINT('Ctrl Pts',(0.47596800043997,1.04324617422688,2.));
#27561=CARTESIAN_POINT('Ctrl Pts',(0.474670775798635,1.04046447410142,2.));
#27562=CARTESIAN_POINT('Ctrl Pts',(0.473467316455455,1.03763771239116,2.));
#27563=CARTESIAN_POINT('Ctrl Pts',(0.472361155190705,1.03477908408591,2.));
#27564=CARTESIAN_POINT('Ctrl Pts',(0.468806973334995,1.02559408983729,2.));
#27565=CARTESIAN_POINT('Ctrl Pts',(0.466243705645806,1.01606061108597,2.));
#27566=CARTESIAN_POINT('Ctrl Pts',(0.464705298489784,1.00636043426204,2.));
#27567=CARTESIAN_POINT('Ctrl Pts',(0.463992209982944,1.00186417033063,2.));
#27568=CARTESIAN_POINT('Ctrl Pts',(0.463499910544365,0.997331632125338,
2.));
#27569=CARTESIAN_POINT('Ctrl Pts',(0.463235250450622,0.992779388102766,
2.));
#27570=CARTESIAN_POINT('Ctrl Pts',(0.463040833672037,0.989435353096635,
2.));
#27571=CARTESIAN_POINT('Ctrl Pts',(0.46296992260639,0.986088149337579,2.));
#27572=CARTESIAN_POINT('Ctrl Pts',(0.46302377604218,0.982751482606387,2.));
#27573=CARTESIAN_POINT('Ctrl Pts',(0.463137043908312,0.975733599437203,
2.));
#27574=CARTESIAN_POINT('Ctrl Pts',(0.463800875129207,0.968753205425666,
2.));
#27575=CARTESIAN_POINT('Ctrl Pts',(0.465031313050322,0.961871658945486,
2.));
#27576=CARTESIAN_POINT('Ctrl Pts',(0.466389625771061,0.954274939141924,
2.));
#27577=CARTESIAN_POINT('Ctrl Pts',(0.468437981894213,0.946798226077515,
2.));
#27578=CARTESIAN_POINT('Ctrl Pts',(0.471116510174533,0.93949861845872,2.));
#27579=CARTESIAN_POINT('Ctrl Pts',(0.472251116178103,0.936406555295212,
2.));
#27580=CARTESIAN_POINT('Ctrl Pts',(0.473496242998671,0.933354214505235,
2.));
#27581=CARTESIAN_POINT('Ctrl Pts',(0.474844471797333,0.930349759755262,
2.));
#27582=CARTESIAN_POINT('Ctrl Pts',(0.478666396590115,0.921832807655503,
2.));
#27583=CARTESIAN_POINT('Ctrl Pts',(0.483317968956197,0.913689888494062,
2.));
#27584=CARTESIAN_POINT('Ctrl Pts',(0.488689858313544,0.906016314077791,
2.));
#27585=CARTESIAN_POINT('Ctrl Pts',(0.491565612706781,0.90190838968258,2.));
#27586=CARTESIAN_POINT('Ctrl Pts',(0.494648435962255,0.897935032536209,
2.));
#27587=CARTESIAN_POINT('Ctrl Pts',(0.497925409635587,0.894112192538158,
2.));
#27588=CARTESIAN_POINT('Ctrl Pts',(0.500336494700513,0.891299477715359,
2.));
#27589=CARTESIAN_POINT('Ctrl Pts',(0.502853422244813,0.888568058918467,
2.));
#27590=CARTESIAN_POINT('Ctrl Pts',(0.505459745106002,0.885935613780059,
2.));
#27591=CARTESIAN_POINT('Ctrl Pts',(0.510032972332535,0.881316550670653,
2.));
#27592=CARTESIAN_POINT('Ctrl Pts',(0.514888364383629,0.876993029350264,
2.));
#27593=CARTESIAN_POINT('Ctrl Pts',(0.519995780056594,0.872997639132679,
2.));
#27594=CARTESIAN_POINT('Ctrl Pts',(0.52477137880872,0.869261820127707,2.));
#27595=CARTESIAN_POINT('Ctrl Pts',(0.529772958435197,0.865810229192487,
2.));
#27596=CARTESIAN_POINT('Ctrl Pts',(0.534950221975527,0.862688964531106,
2.));
#27597=CARTESIAN_POINT('Ctrl Pts',(0.540826105312277,0.859146516504166,
2.));
#27598=CARTESIAN_POINT('Ctrl Pts',(0.546932713096854,0.856024683905292,
2.));
#27599=CARTESIAN_POINT('Ctrl Pts',(0.553238070670066,0.853364148387157,
2.));
#27600=CARTESIAN_POINT('Ctrl Pts',(0.55548342158471,0.852416726168872,2.));
#27601=CARTESIAN_POINT('Ctrl Pts',(0.55775402783163,0.851527860483116,2.));
#27602=CARTESIAN_POINT('Ctrl Pts',(0.560047775926793,0.850696975355778,
2.));
#27603=CARTESIAN_POINT('Ctrl Pts',(0.639851384185725,0.850935057178149,
2.));
#27604=CARTESIAN_POINT('Ctrl Pts',(0.649880550625801,0.854599673316433,
2.));
#27605=CARTESIAN_POINT('Ctrl Pts',(0.659434984589242,0.859362630571034,
2.));
#27606=CARTESIAN_POINT('Ctrl Pts',(0.668403151796856,0.865074094293816,
2.));
#27607=CARTESIAN_POINT('Ctrl Pts',(0.672868418174611,0.867917842223432,
2.));
#27608=CARTESIAN_POINT('Ctrl Pts',(0.677187921251714,0.870997452272092,
2.));
#27609=CARTESIAN_POINT('Ctrl Pts',(0.68134463777063,0.874297734044997,2.));
#27610=CARTESIAN_POINT('Ctrl Pts',(0.684149977150149,0.876525071506887,
2.));
#27611=CARTESIAN_POINT('Ctrl Pts',(0.686881121795098,0.878852960779101,
2.));
#27612=CARTESIAN_POINT('Ctrl Pts',(0.689532114008666,0.881277074288136,
2.));
#27613=CARTESIAN_POINT('Ctrl Pts',(0.691903244332041,0.883445277204446,
2.));
#27614=CARTESIAN_POINT('Ctrl Pts',(0.694203548662863,0.885684381973589,
2.));
#27615=CARTESIAN_POINT('Ctrl Pts',(0.696428614090338,0.88798915510679,2.));
#27616=CARTESIAN_POINT('Ctrl Pts',(0.703655681573731,0.895475115187732,
2.));
#27617=CARTESIAN_POINT('Ctrl Pts',(0.710097129721786,0.903656484453022,
2.));
#27618=CARTESIAN_POINT('Ctrl Pts',(0.715619710640267,0.912413235085866,
2.));
#27619=CARTESIAN_POINT('Ctrl Pts',(0.717914173550032,0.916051396270592,
2.));
#27620=CARTESIAN_POINT('Ctrl Pts',(0.720049467939456,0.919789119253813,
2.));
#27621=CARTESIAN_POINT('Ctrl Pts',(0.722013376555431,0.923618433392056,
2.));
#27622=CARTESIAN_POINT('Ctrl Pts',(0.723497129119939,0.926511518450447,
2.));
#27623=CARTESIAN_POINT('Ctrl Pts',(0.724882801444961,0.929457199976584,
2.));
#27624=CARTESIAN_POINT('Ctrl Pts',(0.726159624011702,0.932438329054375,
2.));
#27625=CARTESIAN_POINT('Ctrl Pts',(0.729321918563565,0.939821663659088,
2.));
#27626=CARTESIAN_POINT('Ctrl Pts',(0.731828910123054,0.947442062000798,
2.));
#27627=CARTESIAN_POINT('Ctrl Pts',(0.733609769329411,0.955243743262114,
2.));
#27628=CARTESIAN_POINT('Ctrl Pts',(0.735247922763181,0.962420251602462,
2.));
#27629=CARTESIAN_POINT('Ctrl Pts',(0.736271202825978,0.969750659080777,
2.));
#27630=CARTESIAN_POINT('Ctrl Pts',(0.736691001072906,0.977159517273332,
2.));
#27631=CARTESIAN_POINT('Ctrl Pts',(0.736867146035702,0.980268232138734,
2.));
#27632=CARTESIAN_POINT('Ctrl Pts',(0.736936465492878,0.983387259690693,
2.));
#27633=CARTESIAN_POINT('Ctrl Pts',(0.736900567292279,0.986501129084147,
2.));
#27634=CARTESIAN_POINT('Ctrl Pts',(0.736803245735092,0.994942962189629,
2.));
#27635=CARTESIAN_POINT('Ctrl Pts',(0.73593588116366,1.00336883005034,2.));
#27636=CARTESIAN_POINT('Ctrl Pts',(0.734324538110121,1.01166511142386,2.));
#27637=CARTESIAN_POINT('Ctrl Pts',(0.733128714763866,1.01782201695168,2.));
#27638=CARTESIAN_POINT('Ctrl Pts',(0.731522528281544,1.02390757926145,2.));
#27639=CARTESIAN_POINT('Ctrl Pts',(0.729508215420297,1.02987014335002,2.));
#27640=CARTESIAN_POINT('Ctrl Pts',(0.728323015262132,1.03337845233062,2.));
#27641=CARTESIAN_POINT('Ctrl Pts',(0.726998715515976,1.03683672165704,2.));
#27642=CARTESIAN_POINT('Ctrl Pts',(0.725539078662676,1.04022915093548,2.));
#27643=CARTESIAN_POINT('Ctrl Pts',(0.723248638897094,1.04555249893377,2.));
#27644=CARTESIAN_POINT('Ctrl Pts',(0.72062367285432,1.05071856137362,2.));
#27645=CARTESIAN_POINT('Ctrl Pts',(0.717666916538866,1.05568500977016,2.));
#27646=CARTESIAN_POINT('Ctrl Pts',(0.71562546757316,1.05911402111255,2.));
#27647=CARTESIAN_POINT('Ctrl Pts',(0.713425303385499,1.06244761425647,2.));
#27648=CARTESIAN_POINT('Ctrl Pts',(0.711075710473028,1.06565922484506,2.));
#27649=CARTESIAN_POINT('Ctrl Pts',(0.707783289804617,1.0701595674468,2.));
#27650=CARTESIAN_POINT('Ctrl Pts',(0.704194035235276,1.07442715810878,2.));
#27651=CARTESIAN_POINT('Ctrl Pts',(0.700309073757905,1.07842075422663,2.));
#27652=CARTESIAN_POINT('Ctrl Pts',(0.698907297616712,1.07986172804018,2.));
#27653=CARTESIAN_POINT('Ctrl Pts',(0.697466981619643,1.08126696829348,2.));
#27654=CARTESIAN_POINT('Ctrl Pts',(0.695989840302895,1.08263572859343,2.));
#27655=CARTESIAN_POINT('Origin',(0.6,1.,2.51042117235887));
#27656=CARTESIAN_POINT('Ctrl Pts',(0.445511859130131,1.0000741974826,2.38542117235887));
#27657=CARTESIAN_POINT('Ctrl Pts',(0.445481645904189,1.00486660347515,2.38517311518799));
#27658=CARTESIAN_POINT('Ctrl Pts',(0.447840382858598,1.06018738535655,2.38230820767121));
#27659=CARTESIAN_POINT('Ctrl Pts',(0.514365803623529,1.16027111832567,2.37682644980854));
#27660=CARTESIAN_POINT('Ctrl Pts',(0.686438402045863,1.1598170503231,2.36897589877086));
#27661=CARTESIAN_POINT('Ctrl Pts',(0.780990355889297,1.01606136385454,2.36112534773319));
#27662=CARTESIAN_POINT('Ctrl Pts',(0.713226176840859,0.857888178208998,
2.35327479669551));
#27663=CARTESIAN_POINT('Ctrl Pts',(0.54391790721615,0.827171013394288,2.34542424565783));
#27664=CARTESIAN_POINT('Ctrl Pts',(0.453699048722976,0.921380393628473,
2.33947303754562));
#27665=CARTESIAN_POINT('Ctrl Pts',(0.445641803334383,0.985947130304853,
2.3361386797793));
#27666=CARTESIAN_POINT('Ctrl Pts',(0.445758404806891,0.999869526120069,
2.33542117235887));
#27667=CARTESIAN_POINT('Ctrl Pts',(0.445864724392684,0.99983533609866,2.38957882764113));
#27668=CARTESIAN_POINT('Ctrl Pts',(0.446099244735942,1.0340318743782,2.38781885106897));
#27669=CARTESIAN_POINT('Ctrl Pts',(0.47398874803022,1.11953643095444,2.38344202415091));
#27670=CARTESIAN_POINT('Ctrl Pts',(0.614413228882944,1.18108612135922,2.37644834688697));
#27671=CARTESIAN_POINT('Ctrl Pts',(0.759000551270414,1.08793755388759,2.36859779584929));
#27672=CARTESIAN_POINT('Ctrl Pts',(0.761051274433651,0.91584221771742,2.36074724481161));
#27673=CARTESIAN_POINT('Ctrl Pts',(0.618637433005314,0.819263404514795,
2.35289669377393));
#27674=CARTESIAN_POINT('Ctrl Pts',(0.475625295654385,0.878125251073759,
2.34584055471711));
#27675=CARTESIAN_POINT('Ctrl Pts',(0.446073423867575,0.964737113217481,
2.34140126600617));
#27676=CARTESIAN_POINT('Ctrl Pts',(0.445798439227784,1.00012317213786,2.33957882764113));
#27677=CARTESIAN_POINT('Ctrl Pts',(0.695811615272236,1.08252112989365,2.4));
#27678=CARTESIAN_POINT('Ctrl Pts',(0.7229481205055,1.0510141400767,2.39738314965411));
#27679=CARTESIAN_POINT('Ctrl Pts',(0.743289653273766,0.959678556377187,
2.39214944896232));
#27680=CARTESIAN_POINT('Ctrl Pts',(0.645248987396393,0.85804501052042,2.38429889792465));
#27681=CARTESIAN_POINT('Ctrl Pts',(0.506625118128944,0.884053189554221,
2.37644834688697));
#27682=CARTESIAN_POINT('Ctrl Pts',(0.45174554898112,1.01388156392493,2.36859779584929));
#27683=CARTESIAN_POINT('Ctrl Pts',(0.529822137836651,1.13134337597071,2.36074724481161));
#27684=CARTESIAN_POINT('Ctrl Pts',(0.670836914703171,1.13097126385843,2.35289669377393));
#27685=CARTESIAN_POINT('Ctrl Pts',(0.748322945574864,1.01316240738436,2.34504614273625));
#27686=CARTESIAN_POINT('Ctrl Pts',(0.692789695797321,0.883538302880933,
2.33719559169858));
#27687=CARTESIAN_POINT('Ctrl Pts',(0.554040306983033,0.858365357379829,
2.3293450406609));
#27688=CARTESIAN_POINT('Ctrl Pts',(0.456508731628746,0.960210907421746,
2.32149448962322));
#27689=CARTESIAN_POINT('Ctrl Pts',(0.487663502390397,1.09774169610628,2.31364393858554));
#27690=CARTESIAN_POINT('Ctrl Pts',(0.619564332496711,1.14761467812196,2.30579338754787));
#27691=CARTESIAN_POINT('Ctrl Pts',(0.733919395128131,1.0651036788751,2.29794283651019));
#27692=CARTESIAN_POINT('Ctrl Pts',(0.728172365024857,0.924205963670542,
2.29009228547251));
#27693=CARTESIAN_POINT('Ctrl Pts',(0.607477308519567,0.851282238312653,
2.28224173443483));
#27694=CARTESIAN_POINT('Ctrl Pts',(0.480076425153724,0.911732088265042,
2.27439118339715));
#27695=CARTESIAN_POINT('Ctrl Pts',(0.46022585412805,1.05134272481009,2.26654063235948));
#27696=CARTESIAN_POINT('Ctrl Pts',(0.565728060366633,1.14490797247226,2.2586900813218));
#27697=CARTESIAN_POINT('Ctrl Pts',(0.701966156681371,1.1085163118784,2.25083953028412));
#27698=CARTESIAN_POINT('Ctrl Pts',(0.746758579656851,0.974804639683806,
2.24298897924644));
#27699=CARTESIAN_POINT('Ctrl Pts',(0.659934419370361,0.863688767275607,
2.23513842820876));
#27700=CARTESIAN_POINT('Ctrl Pts',(0.519359646953508,0.874820048138925,
2.22728787717109));
#27701=CARTESIAN_POINT('Ctrl Pts',(0.451105060253533,0.998215686247253,
2.21943732613341));
#27702=CARTESIAN_POINT('Ctrl Pts',(0.516382995296938,1.12321153912718,2.21158677509573));
#27703=CARTESIAN_POINT('Ctrl Pts',(0.656650648038066,1.13770835464619,2.20373622405805));
#27704=CARTESIAN_POINT('Ctrl Pts',(0.746112652823594,1.02870504382673,2.19588567302037));
#27705=CARTESIAN_POINT('Ctrl Pts',(0.704537356935342,0.893958367321059,
2.1880351219827));
#27706=CARTESIAN_POINT('Ctrl Pts',(0.569210474097529,0.854312347959086,
2.18018457094502));
#27707=CARTESIAN_POINT('Ctrl Pts',(0.461496370101168,0.945322478526838,
2.17233401990734));
#27708=CARTESIAN_POINT('Ctrl Pts',(0.477995614068202,1.08536871014064,2.16448346886966));
#27709=CARTESIAN_POINT('Ctrl Pts',(0.603911291955373,1.14885425315604,2.15663291783199));
#27710=CARTESIAN_POINT('Ctrl Pts',(0.726319229979197,1.07884376278165,2.14878236679431));
#27711=CARTESIAN_POINT('Ctrl Pts',(0.73544107998541,0.938124312232147,2.14093181575663));
#27712=CARTESIAN_POINT('Ctrl Pts',(0.623096148559508,0.852896448126576,
2.13308126471895));
#27713=CARTESIAN_POINT('Ctrl Pts',(0.490038043939787,0.899594549193445,
2.12523071368128));
#27714=CARTESIAN_POINT('Ctrl Pts',(0.455596431949525,1.03633864030821,2.11738016264359));
#27715=CARTESIAN_POINT('Ctrl Pts',(0.550659380176962,1.14049338518748,2.10952961160592));
#27716=CARTESIAN_POINT('Ctrl Pts',(0.689972154741195,1.11865030196008,2.10167906056824));
#27717=CARTESIAN_POINT('Ctrl Pts',(0.748595790516416,0.990398846945399,
2.09382850953056));
#27718=CARTESIAN_POINT('Ctrl Pts',(0.673955132588938,0.870757856106032,
2.08597795849288));
#27719=CARTESIAN_POINT('Ctrl Pts',(0.532989863833319,0.867024446028552,
2.0781274074552));
#27720=CARTESIAN_POINT('Ctrl Pts',(0.45212066157753,0.982546372277999,2.07027685641753));
#27721=CARTESIAN_POINT('Ctrl Pts',(0.503873591498137,1.11372171989345,2.06242630537985));
#27722=CARTESIAN_POINT('Ctrl Pts',(0.641834132936712,1.14290755996024,2.05457575434217));
#27723=CARTESIAN_POINT('Ctrl Pts',(0.742278474130153,1.04393279346011,2.04672520330449));
#27724=CARTESIAN_POINT('Ctrl Pts',(0.71512086495066,0.905553551654031,2.03887465226682));
#27725=CARTESIAN_POINT('Ctrl Pts',(0.584726479537104,0.851884977081971,
2.03102410122914));
#27726=CARTESIAN_POINT('Ctrl Pts',(0.468017266318098,0.931032088917713,
2.02317355019146));
#27727=CARTESIAN_POINT('Ctrl Pts',(0.469697842938816,1.07206544198931,2.01532299915378));
#27728=CARTESIAN_POINT('Ctrl Pts',(0.588188246262365,1.1484015292732,2.0074724481161));
#27729=CARTESIAN_POINT('Ctrl Pts',(0.717366805638866,1.09178084131602,1.99962189707843));
#27730=CARTESIAN_POINT('Ctrl Pts',(0.741097987339953,0.952575306856465,
1.99177134604075));
#27731=CARTESIAN_POINT('Ctrl Pts',(0.672829925654733,0.888579693265875,
1.98653764534896));
#27732=CARTESIAN_POINT('Ctrl Pts',(0.63265850635311,0.877840168374445,1.98392079500307));
#27733=CARTESIAN_POINT('Ctrl Pts',(0.702845629995662,1.08857942294107,2.40535973499898));
#27734=CARTESIAN_POINT('Ctrl Pts',(0.731974363173428,1.05475934582637,2.40274288465309));
#27735=CARTESIAN_POINT('Ctrl Pts',(0.753809270628911,0.956718355494374,
2.3975091839613));
#27736=CARTESIAN_POINT('Ctrl Pts',(0.648570944161886,0.84762337757721,2.38965863292362));
#27737=CARTESIAN_POINT('Ctrl Pts',(0.499769996315029,0.875540948428836,
2.38180808188594));
#27738=CARTESIAN_POINT('Ctrl Pts',(0.440861440741036,1.01490067966319,2.37395753084827));
#27739=CARTESIAN_POINT('Ctrl Pts',(0.524670026432277,1.1409859567557,2.36610697981059));
#27740=CARTESIAN_POINT('Ctrl Pts',(0.676037410484068,1.14058652601332,2.35825642877291));
#27741=CARTESIAN_POINT('Ctrl Pts',(0.759212082346341,1.01412872620776,2.35040587773524));
#27742=CARTESIAN_POINT('Ctrl Pts',(0.699601856145167,0.87498826132362,2.34255532669755));
#27743=CARTESIAN_POINT('Ctrl Pts',(0.550666173727406,0.847967242717983,
2.33470477565988));
#27744=CARTESIAN_POINT('Ctrl Pts',(0.445974312690722,0.957289789118585,
2.32685422462219));
#27745=CARTESIAN_POINT('Ctrl Pts',(0.479416312569843,1.10491740781463,2.31900367358452));
#27746=CARTESIAN_POINT('Ctrl Pts',(0.62100064898553,1.15845181740151,2.31115312254684));
#27747=CARTESIAN_POINT('Ctrl Pts',(0.743751094493674,1.06988326884919,2.30330257150917));
#27748=CARTESIAN_POINT('Ctrl Pts',(0.737582145876161,0.918641540547371,
2.29545202047149));
#27749=CARTESIAN_POINT('Ctrl Pts',(0.608026255513821,0.840364116095719,
2.28760146943381));
#27750=CARTESIAN_POINT('Ctrl Pts',(0.471272229662835,0.905251894929553,
2.27975091839613));
#27751=CARTESIAN_POINT('Ctrl Pts',(0.449964327931837,1.05511205362507,2.27190036735845));
#27752=CARTESIAN_POINT('Ctrl Pts',(0.563211984134157,1.15554639881562,2.26404981632078));
#27753=CARTESIAN_POINT('Ctrl Pts',(0.709452007382772,1.11648304256461,2.2561992652831));
#27754=CARTESIAN_POINT('Ctrl Pts',(0.757532868423012,0.972954920994454,
2.24834871424542));
#27755=CARTESIAN_POINT('Ctrl Pts',(0.664334507888787,0.853681471028408,
2.24049816320774));
#27756=CARTESIAN_POINT('Ctrl Pts',(0.513439431236242,0.865629955455834,
2.23264761217006));
#27757=CARTESIAN_POINT('Ctrl Pts',(0.440173930500167,0.998084690760198,
2.22479706113238));
#27758=CARTESIAN_POINT('Ctrl Pts',(0.510244248543333,1.13225712068693,2.21694651009471));
#27759=CARTESIAN_POINT('Ctrl Pts',(0.660809658313168,1.14781822067201,2.20909595905703));
#27760=CARTESIAN_POINT('Ctrl Pts',(0.756839520837664,1.03081242611373,2.20124540801935));
#27761=CARTESIAN_POINT('Ctrl Pts',(0.71221197243725,0.886173315337117,2.19339485698167));
#27762=CARTESIAN_POINT('Ctrl Pts',(0.566950059450412,0.843616681399604,
2.18554430594399));
#27763=CARTESIAN_POINT('Ctrl Pts',(0.451328118901268,0.941308325441225,
2.17769375490632));
#27764=CARTESIAN_POINT('Ctrl Pts',(0.469038655723137,1.09163605844015,2.16984320386864));
#27765=CARTESIAN_POINT('Ctrl Pts',(0.604198439657909,1.15978239590126,2.16199265283096));
#27766=CARTESIAN_POINT('Ctrl Pts',(0.735592962824645,1.08463208173108,2.15414210179328));
#27767=CARTESIAN_POINT('Ctrl Pts',(0.745384493923972,0.933581705393252,
2.14629155075561));
#27768=CARTESIAN_POINT('Ctrl Pts',(0.624791753508452,0.842096833207175,
2.13844099971793));
#27769=CARTESIAN_POINT('Ctrl Pts',(0.481965181210706,0.892223277795097,
2.13059044868025));
#27770=CARTESIAN_POINT('Ctrl Pts',(0.444995036483054,1.03900644347833,2.12273989764257));
#27771=CARTESIAN_POINT('Ctrl Pts',(0.547037036003845,1.15080771437549,2.11488934660489));
#27772=CARTESIAN_POINT('Ctrl Pts',(0.696577465165717,1.12736102005574,2.10703879556722));
#27773=CARTESIAN_POINT('Ctrl Pts',(0.759504958213481,0.989693977794033,
2.09918824452954));
#27774=CARTESIAN_POINT('Ctrl Pts',(0.679384552498262,0.861269537383356,
2.09133769349186));
#27775=CARTESIAN_POINT('Ctrl Pts',(0.52807031119791,0.857262038810666,2.08348714245418));
#27776=CARTESIAN_POINT('Ctrl Pts',(0.441264092248243,0.981265013290105,
2.07563659141651));
#27777=CARTESIAN_POINT('Ctrl Pts',(0.496816466213367,1.12207060588009,2.06778604037882));
#27778=CARTESIAN_POINT('Ctrl Pts',(0.644905387984261,1.15339912591488,2.05993548934115));
#27779=CARTESIAN_POINT('Ctrl Pts',(0.752723855715824,1.04715812177925,2.05208493830347));
#27780=CARTESIAN_POINT('Ctrl Pts',(0.723572469244521,0.89861976073157,2.04423438726579));
#27781=CARTESIAN_POINT('Ctrl Pts',(0.583605173237138,0.84101110496317,2.03638383622811));
#27782=CARTESIAN_POINT('Ctrl Pts',(0.458327747053459,0.92596880613495,2.02853328519044));
#27783=CARTESIAN_POINT('Ctrl Pts',(0.460131703294282,1.07735613016487,2.02068273415276));
#27784=CARTESIAN_POINT('Ctrl Pts',(0.587321085746765,1.15929643527098,2.01283218311508));
#27785=CARTESIAN_POINT('Ctrl Pts',(0.72598329578528,1.09851893655959,2.0049816320774));
#27786=CARTESIAN_POINT('Ctrl Pts',(0.751456703426463,0.949093620540274,
1.99713108103973));
#27787=CARTESIAN_POINT('Ctrl Pts',(0.6781767384384,0.880399765646143,1.99189738034794));
#27788=CARTESIAN_POINT('Ctrl Pts',(0.635056132297315,0.86887179797568,1.98928053000205));
#27789=CARTESIAN_POINT('Ctrl Pts',(0.709879644719089,1.09463771598849,2.41071946999795));
#27790=CARTESIAN_POINT('Ctrl Pts',(0.741000605841355,1.05850455157604,2.40810261965206));
#27791=CARTESIAN_POINT('Ctrl Pts',(0.764328887984058,0.953758154611561,
2.40286891896028));
#27792=CARTESIAN_POINT('Ctrl Pts',(0.651892900927377,0.837201744634001,
2.3950183679226));
#27793=CARTESIAN_POINT('Ctrl Pts',(0.492914874501113,0.867028707303451,
2.38716781688492));
#27794=CARTESIAN_POINT('Ctrl Pts',(0.429977332500953,1.01591979540145,2.37931726584724));
#27795=CARTESIAN_POINT('Ctrl Pts',(0.519517915027903,1.15062853754068,2.37146671480957));
#27796=CARTESIAN_POINT('Ctrl Pts',(0.681237906264966,1.15020178816821,2.36361616377189));
#27797=CARTESIAN_POINT('Ctrl Pts',(0.770101219117818,1.01509504503115,2.35576561273421));
#27798=CARTESIAN_POINT('Ctrl Pts',(0.706414016493014,0.866438219766308,
2.34791506169653));
#27799=CARTESIAN_POINT('Ctrl Pts',(0.547292040471776,0.837569128056136,
2.34006451065885));
#27800=CARTESIAN_POINT('Ctrl Pts',(0.435439893752698,0.954368670815423,
2.33221395962117));
#27801=CARTESIAN_POINT('Ctrl Pts',(0.471169122749288,1.11209311952297,2.3243634085835));
#27802=CARTESIAN_POINT('Ctrl Pts',(0.622436965474348,1.16928895668105,2.31651285754582));
#27803=CARTESIAN_POINT('Ctrl Pts',(0.753582793859216,1.07466285882328,2.30866230650814));
#27804=CARTESIAN_POINT('Ctrl Pts',(0.746991926727465,0.913077117424199,
2.30081175547046));
#27805=CARTESIAN_POINT('Ctrl Pts',(0.608575202508074,0.829445993878789,
2.29296120443279));
#27806=CARTESIAN_POINT('Ctrl Pts',(0.462468034171945,0.898771701594062,
2.28511065339511));
#27807=CARTESIAN_POINT('Ctrl Pts',(0.439702801735622,1.05888138244004,2.27726010235743));
#27808=CARTESIAN_POINT('Ctrl Pts',(0.560695907901683,1.16618482515898,2.26940955131976));
#27809=CARTESIAN_POINT('Ctrl Pts',(0.716937858084172,1.12444977325082,2.26155900028207));
#27810=CARTESIAN_POINT('Ctrl Pts',(0.768307157189173,0.9711052023051,2.2537084492444));
#27811=CARTESIAN_POINT('Ctrl Pts',(0.668734596407212,0.843674174781211,
2.24585789820672));
#27812=CARTESIAN_POINT('Ctrl Pts',(0.507519215518976,0.856439862772741,
2.23800734716904));
#27813=CARTESIAN_POINT('Ctrl Pts',(0.429242800746802,0.997953695273144,
2.23015679613136));
#27814=CARTESIAN_POINT('Ctrl Pts',(0.504105501789727,1.14130270224668,2.22230624509369));
#27815=CARTESIAN_POINT('Ctrl Pts',(0.664968668588271,1.15792808669784,2.214455694056));
#27816=CARTESIAN_POINT('Ctrl Pts',(0.767566388851732,1.03291980840074,2.20660514301833));
#27817=CARTESIAN_POINT('Ctrl Pts',(0.71988658793916,0.878388263353175,2.19875459198065));
#27818=CARTESIAN_POINT('Ctrl Pts',(0.564689644803295,0.832921014840122,
2.19090404094297));
#27819=CARTESIAN_POINT('Ctrl Pts',(0.441159867701366,0.937294172355611,
2.1830534899053));
#27820=CARTESIAN_POINT('Ctrl Pts',(0.460081697378071,1.09790340673965,2.17520293886761));
#27821=CARTESIAN_POINT('Ctrl Pts',(0.604485587360446,1.17071053864647,2.16735238782994));
#27822=CARTESIAN_POINT('Ctrl Pts',(0.744866695670093,1.09042040068052,2.15950183679226));
#27823=CARTESIAN_POINT('Ctrl Pts',(0.755327907862536,0.929039098554358,
2.15165128575458));
#27824=CARTESIAN_POINT('Ctrl Pts',(0.626487358457396,0.831297218287773,
2.1438007347169));
#27825=CARTESIAN_POINT('Ctrl Pts',(0.473892318481626,0.884852006396751,
2.13595018367923));
#27826=CARTESIAN_POINT('Ctrl Pts',(0.434393641016582,1.04167424664844,2.12809963264155));
#27827=CARTESIAN_POINT('Ctrl Pts',(0.54341469183073,1.1611220435635,2.12024908160387));
#27828=CARTESIAN_POINT('Ctrl Pts',(0.703182775590238,1.1360717381514,2.11239853056619));
#27829=CARTESIAN_POINT('Ctrl Pts',(0.770414125910549,0.988989108642668,
2.10454797952851));
#27830=CARTESIAN_POINT('Ctrl Pts',(0.684813972407585,0.851781218660681,
2.09669742849084));
#27831=CARTESIAN_POINT('Ctrl Pts',(0.523150758562502,0.84749963159278,2.08884687745316));
#27832=CARTESIAN_POINT('Ctrl Pts',(0.430407522918953,0.979983654302211,
2.08099632641548));
#27833=CARTESIAN_POINT('Ctrl Pts',(0.489759340928599,1.13041949186674,2.0731457753778));
#27834=CARTESIAN_POINT('Ctrl Pts',(0.647976643031809,1.16389069186952,2.06529522434013));
#27835=CARTESIAN_POINT('Ctrl Pts',(0.763169237301496,1.05038345009838,2.05744467330245));
#27836=CARTESIAN_POINT('Ctrl Pts',(0.732024073538381,0.89168596980911,2.04959412226477));
#27837=CARTESIAN_POINT('Ctrl Pts',(0.582483866937173,0.830137232844369,
2.04174357122709));
#27838=CARTESIAN_POINT('Ctrl Pts',(0.448638227788819,0.920905523352185,
2.03389302018941));
#27839=CARTESIAN_POINT('Ctrl Pts',(0.450565563649749,1.08264681834044,2.02604246915174));
#27840=CARTESIAN_POINT('Ctrl Pts',(0.586453925231163,1.17019134126876,2.01819191811406));
#27841=CARTESIAN_POINT('Ctrl Pts',(0.734599785931696,1.10525703180317,2.01034136707638));
#27842=CARTESIAN_POINT('Ctrl Pts',(0.761815419512973,0.945611934224082,
2.0024908160387));
#27843=CARTESIAN_POINT('Ctrl Pts',(0.683523551222068,0.872219838026411,
1.99725711534692));
#27844=CARTESIAN_POINT('Ctrl Pts',(0.63745375824152,0.859903427576914,1.99464026500102));
#27845=CARTESIAN_POINT('Ctrl Pts',(0.716913659442515,1.10069600903591,2.41607920499693));
#27846=CARTESIAN_POINT('Ctrl Pts',(0.750026848509282,1.0622497573257,2.41346235465104));
#27847=CARTESIAN_POINT('Ctrl Pts',(0.774848505339203,0.950797953728747,
2.40822865395925));
#27848=CARTESIAN_POINT('Ctrl Pts',(0.65521485769287,0.826780111690792,2.40037810292158));
#27849=CARTESIAN_POINT('Ctrl Pts',(0.486059752687198,0.858516466178065,
2.3925275518839));
#27850=CARTESIAN_POINT('Ctrl Pts',(0.419093224260869,1.01693891113971,2.38467700084622));
#27851=CARTESIAN_POINT('Ctrl Pts',(0.514365803623529,1.16027111832567,2.37682644980854));
#27852=CARTESIAN_POINT('Ctrl Pts',(0.686438402045863,1.1598170503231,2.36897589877086));
#27853=CARTESIAN_POINT('Ctrl Pts',(0.780990355889297,1.01606136385454,2.36112534773319));
#27854=CARTESIAN_POINT('Ctrl Pts',(0.713226176840859,0.857888178208998,
2.35327479669551));
#27855=CARTESIAN_POINT('Ctrl Pts',(0.54391790721615,0.827171013394288,2.34542424565783));
#27856=CARTESIAN_POINT('Ctrl Pts',(0.424905474814674,0.951447552512262,
2.33757369462016));
#27857=CARTESIAN_POINT('Ctrl Pts',(0.462921932928734,1.11926883123131,2.32972314358247));
#27858=CARTESIAN_POINT('Ctrl Pts',(0.623873281963166,1.1801260959606,2.3218725925448));
#27859=CARTESIAN_POINT('Ctrl Pts',(0.76341449322476,1.07944244879737,2.31402204150712));
#27860=CARTESIAN_POINT('Ctrl Pts',(0.756401707578768,0.907512694301026,
2.30617149046944));
#27861=CARTESIAN_POINT('Ctrl Pts',(0.609124149502328,0.818527871661859,
2.29832093943176));
#27862=CARTESIAN_POINT('Ctrl Pts',(0.453663838681055,0.892291508258571,
2.29047038839408));
#27863=CARTESIAN_POINT('Ctrl Pts',(0.429441275539409,1.06265071125502,2.28261983735641));
#27864=CARTESIAN_POINT('Ctrl Pts',(0.558179831669208,1.17682325150234,2.27476928631873));
#27865=CARTESIAN_POINT('Ctrl Pts',(0.724423708785572,1.13241650393702,2.26691873528105));
#27866=CARTESIAN_POINT('Ctrl Pts',(0.779081445955335,0.969255483615749,
2.25906818424337));
#27867=CARTESIAN_POINT('Ctrl Pts',(0.673134684925636,0.833666878534013,
2.25121763320569));
#27868=CARTESIAN_POINT('Ctrl Pts',(0.50159899980171,0.84724977008965,2.24336708216802));
#27869=CARTESIAN_POINT('Ctrl Pts',(0.418311670993437,0.997822699786089,
2.23551653113034));
#27870=CARTESIAN_POINT('Ctrl Pts',(0.497966755036121,1.15034828380644,2.22766598009266));
#27871=CARTESIAN_POINT('Ctrl Pts',(0.669127678863374,1.16803795272366,2.21981542905498));
#27872=CARTESIAN_POINT('Ctrl Pts',(0.778293256865801,1.03502719068774,2.21196487801731));
#27873=CARTESIAN_POINT('Ctrl Pts',(0.727561203441069,0.870603211369231,
2.20411432697963));
#27874=CARTESIAN_POINT('Ctrl Pts',(0.562429230156179,0.822225348280642,
2.19626377594195));
#27875=CARTESIAN_POINT('Ctrl Pts',(0.430991616501465,0.933280019269996,
2.18841322490427));
#27876=CARTESIAN_POINT('Ctrl Pts',(0.451124739033006,1.10417075503916,2.18056267386659));
#27877=CARTESIAN_POINT('Ctrl Pts',(0.604772735062981,1.18163868139168,2.17271212282892));
#27878=CARTESIAN_POINT('Ctrl Pts',(0.754140428515542,1.09620871962996,2.16486157179123));
#27879=CARTESIAN_POINT('Ctrl Pts',(0.765271321801097,0.924496491715462,
2.15701102075356));
#27880=CARTESIAN_POINT('Ctrl Pts',(0.628182963406343,0.820497603368372,
2.14916046971588));
#27881=CARTESIAN_POINT('Ctrl Pts',(0.465819455752544,0.877480734998406,
2.1413099186782));
#27882=CARTESIAN_POINT('Ctrl Pts',(0.423792245550112,1.04434204981856,2.13345936764053));
#27883=CARTESIAN_POINT('Ctrl Pts',(0.539792347657613,1.17143637275151,2.12560881660284));
#27884=CARTESIAN_POINT('Ctrl Pts',(0.70978808601476,1.14478245624706,2.11775826556517));
#27885=CARTESIAN_POINT('Ctrl Pts',(0.781323293607615,0.988284239491303,
2.10990771452749));
#27886=CARTESIAN_POINT('Ctrl Pts',(0.690243392316909,0.842292899938004,
2.10205716348982));
#27887=CARTESIAN_POINT('Ctrl Pts',(0.518231205927094,0.837737224374896,
2.09420661245213));
#27888=CARTESIAN_POINT('Ctrl Pts',(0.419550953589664,0.978702295314315,
2.08635606141446));
#27889=CARTESIAN_POINT('Ctrl Pts',(0.482702215643831,1.13876837785338,2.07850551037678));
#27890=CARTESIAN_POINT('Ctrl Pts',(0.651047898079357,1.17438225782416,2.0706549593391));
#27891=CARTESIAN_POINT('Ctrl Pts',(0.773614618887169,1.05360877841752,2.06280440830142));
#27892=CARTESIAN_POINT('Ctrl Pts',(0.740475677832241,0.884752178886651,
2.05495385726374));
#27893=CARTESIAN_POINT('Ctrl Pts',(0.581362560637208,0.819263360725568,
2.04710330622607));
#27894=CARTESIAN_POINT('Ctrl Pts',(0.438948708524181,0.915842240569421,
2.03925275518839));
#27895=CARTESIAN_POINT('Ctrl Pts',(0.440999424005214,1.08793750651601,2.03140220415071));
#27896=CARTESIAN_POINT('Ctrl Pts',(0.585586764715563,1.18108624726655,2.02355165311303));
#27897=CARTESIAN_POINT('Ctrl Pts',(0.74321627607811,1.11199512704675,2.01570110207536));
#27898=CARTESIAN_POINT('Ctrl Pts',(0.772174135599484,0.94213024790789,2.00785055103768));
#27899=CARTESIAN_POINT('Ctrl Pts',(0.688870364005735,0.864039910406678,
2.00261685034589));
#27900=CARTESIAN_POINT('Ctrl Pts',(0.639851384185725,0.850935057178149,
2.));
#27901=CARTESIAN_POINT('Ctrl Pts',(0.695811615272236,1.08252112989365,2.4));
#27902=CARTESIAN_POINT('Ctrl Pts',(0.702493035444011,1.07628157141353,2.4));
#27903=CARTESIAN_POINT('Ctrl Pts',(0.708395708847424,1.0693103556765,2.4));
#27904=CARTESIAN_POINT('Ctrl Pts',(0.713512656958279,1.06178684479855,2.4));
#27905=CARTESIAN_POINT('Ctrl Pts',(0.717502347100726,1.05592075498562,2.4));
#27906=CARTESIAN_POINT('Ctrl Pts',(0.721014082031974,1.04971755619462,2.4));
#27907=CARTESIAN_POINT('Ctrl Pts',(0.724031956062882,1.04324616442023,2.4));
#27908=CARTESIAN_POINT('Ctrl Pts',(0.725329175480596,1.04046446611758,2.4));
#27909=CARTESIAN_POINT('Ctrl Pts',(0.726532629865294,1.03763770614082,2.4));
#27910=CARTESIAN_POINT('Ctrl Pts',(0.727638786465014,1.03477907962968,2.4));
#27911=CARTESIAN_POINT('Ctrl Pts',(0.731192959070153,1.02559407631572,2.4));
#27912=CARTESIAN_POINT('Ctrl Pts',(0.733756217444906,1.01606058770234,2.4));
#27913=CARTESIAN_POINT('Ctrl Pts',(0.735294617481607,1.0063604023791,2.4));
#27914=CARTESIAN_POINT('Ctrl Pts',(0.736007696124321,1.00186417589745,2.4));
#27915=CARTESIAN_POINT('Ctrl Pts',(0.736499990230692,0.997331676100057,
2.4));
#27916=CARTESIAN_POINT('Ctrl Pts',(0.736764649954775,0.992779471200463,
2.4));
#27917=CARTESIAN_POINT('Ctrl Pts',(0.736959071387571,0.989435380209583,
2.4));
#27918=CARTESIAN_POINT('Ctrl Pts',(0.737029983554064,0.98608811988667,2.4));
#27919=CARTESIAN_POINT('Ctrl Pts',(0.736976127631269,0.982751397582665,
2.4));
#27920=CARTESIAN_POINT('Ctrl Pts',(0.736862856230108,0.975733502594741,
2.4));
#27921=CARTESIAN_POINT('Ctrl Pts',(0.736199022212823,0.968753098529686,
2.4));
#27922=CARTESIAN_POINT('Ctrl Pts',(0.73496858294117,0.96187154470407,2.4));
#27923=CARTESIAN_POINT('Ctrl Pts',(0.733610269619415,0.954274821768571,
2.4));
#27924=CARTESIAN_POINT('Ctrl Pts',(0.731561915556015,0.946798108708432,
2.4));
#27925=CARTESIAN_POINT('Ctrl Pts',(0.728883391181877,0.939498503415491,
2.4));
#27926=CARTESIAN_POINT('Ctrl Pts',(0.727748787370213,0.936406442701396,
2.4));
#27927=CARTESIAN_POINT('Ctrl Pts',(0.726503663184753,0.933354104764928,
2.4));
#27928=CARTESIAN_POINT('Ctrl Pts',(0.725155437375267,0.93034965316141,2.4));
#27929=CARTESIAN_POINT('Ctrl Pts',(0.721333520454809,0.921832708641144,
2.4));
#27930=CARTESIAN_POINT('Ctrl Pts',(0.716681958573065,0.913689799617633,
2.4));
#27931=CARTESIAN_POINT('Ctrl Pts',(0.711310080831161,0.906016236422445,
2.4));
#27932=CARTESIAN_POINT('Ctrl Pts',(0.708434311712215,0.901908288116612,
2.4));
#27933=CARTESIAN_POINT('Ctrl Pts',(0.705351471044678,0.897934909331024,
2.4));
#27934=CARTESIAN_POINT('Ctrl Pts',(0.702074477330367,0.894112050103086,
2.4));
#27935=CARTESIAN_POINT('Ctrl Pts',(0.699663413790917,0.891299363444374,
2.4));
#27936=CARTESIAN_POINT('Ctrl Pts',(0.697146509627061,0.888567971784173,
2.4));
#27937=CARTESIAN_POINT('Ctrl Pts',(0.694540211514707,0.885935552211034,
2.4));
#27938=CARTESIAN_POINT('Ctrl Pts',(0.689966981858787,0.881316487645227,
2.4));
#27939=CARTESIAN_POINT('Ctrl Pts',(0.685111586013864,0.876992966093948,
2.4));
#27940=CARTESIAN_POINT('Ctrl Pts',(0.680004164916354,0.87299757664439,2.4));
#27941=CARTESIAN_POINT('Ctrl Pts',(0.67522858856925,0.869261779852135,2.4));
#27942=CARTESIAN_POINT('Ctrl Pts',(0.670227032530533,0.865810208752244,
2.4));
#27943=CARTESIAN_POINT('Ctrl Pts',(0.665049792940119,0.862688960723077,
2.4));
#27944=CARTESIAN_POINT('Ctrl Pts',(0.659173917535639,0.859146519967616,
2.4));
#27945=CARTESIAN_POINT('Ctrl Pts',(0.653067316624201,0.856024693283448,
2.4));
#27946=CARTESIAN_POINT('Ctrl Pts',(0.646761964313973,0.85336416176701,2.4));
#27947=CARTESIAN_POINT('Ctrl Pts',(0.644516614709207,0.852416740735641,
2.4));
#27948=CARTESIAN_POINT('Ctrl Pts',(0.642246009555221,0.851527876023459,
2.4));
#27949=CARTESIAN_POINT('Ctrl Pts',(0.63995226235153,0.850696991672974,2.4));
#27950=CARTESIAN_POINT('Ctrl Pts',(0.473597863174539,0.999893075682974,
2.31934196736194));
#27951=CARTESIAN_POINT('Ctrl Pts',(0.473502307398787,0.988483568548598,
2.32005947478237));
#27952=CARTESIAN_POINT('Ctrl Pts',(0.474923175284874,0.977097443610316,
2.3207769822028));
#27953=CARTESIAN_POINT('Ctrl Pts',(0.477956455981403,0.966158447195516,
2.32149448962322));
#27954=CARTESIAN_POINT('Ctrl Pts',(0.489019256746842,0.926262390741107,
2.32411133996911));
#27955=CARTESIAN_POINT('Ctrl Pts',(0.521529781864938,0.892313874060468,
2.32672819031501));
#27956=CARTESIAN_POINT('Ctrl Pts',(0.5609099425597,0.879535106636999,2.3293450406609));
#27957=CARTESIAN_POINT('Ctrl Pts',(0.600290103254463,0.86675633921353,2.33196189100679));
#27958=CARTESIAN_POINT('Ctrl Pts',(0.646539899525892,0.875147321047232,
2.33457874135269));
#27959=CARTESIAN_POINT('Ctrl Pts',(0.678920339291197,0.90094682938132,2.33719559169858));
#27960=CARTESIAN_POINT('Ctrl Pts',(0.711300779056502,0.926746337715409,
2.33981244204447));
#27961=CARTESIAN_POINT('Ctrl Pts',(0.729811862315683,0.969954372549885,
2.34242929239036));
#27962=CARTESIAN_POINT('Ctrl Pts',(0.726153065466658,1.01119319937947,2.34504614273626));
#27963=CARTESIAN_POINT('Ctrl Pts',(0.722494268617633,1.05243202620905,2.34766299308215));
#27964=CARTESIAN_POINT('Ctrl Pts',(0.696665591660402,1.09170164503374,2.35027984342804));
#27965=CARTESIAN_POINT('Ctrl Pts',(0.6602487903707,1.11139847313147,2.35289669377393));
#27966=CARTESIAN_POINT('Ctrl Pts',(0.623831989080998,1.13109530122919,2.35551354411983));
#27967=CARTESIAN_POINT('Ctrl Pts',(0.576827063458825,1.13121933859995,2.35813039446572));
#27968=CARTESIAN_POINT('Ctrl Pts',(0.540311835838483,1.11170438861103,2.36074724481161));
#27969=CARTESIAN_POINT('Ctrl Pts',(0.503796608218141,1.09218943862212,2.3633640951575));
#27970=CARTESIAN_POINT('Ctrl Pts',(0.477771078599631,1.05303550127352,2.3659809455034));
#27971=CARTESIAN_POINT('Ctrl Pts',(0.473904908648346,1.01182047020411,2.36859779584929));
#27972=CARTESIAN_POINT('Ctrl Pts',(0.473538425642629,1.00791360406595,2.36884585302017));
#27973=CARTESIAN_POINT('Ctrl Pts',(0.473371057191087,1.00398821781876,2.36909391019106));
#27974=CARTESIAN_POINT('Ctrl Pts',(0.473395817154925,1.00006080538999,2.36934196736194));
#27975=CARTESIAN_POINT('Ctrl Pts',(0.560148615814278,0.850935057178148,
2.4));
#27976=CARTESIAN_POINT('Ctrl Pts',(0.511129635994267,0.864039910406677,
2.39738314965411));
#27977=CARTESIAN_POINT('Ctrl Pts',(0.427825810157124,0.942129912787787,
2.39214944896232));
#27978=CARTESIAN_POINT('Ctrl Pts',(0.456783771264579,1.11199528864852,2.38429889792464));
#27979=CARTESIAN_POINT('Ctrl Pts',(0.614413228882944,1.18108612135922,2.37644834688697));
#27980=CARTESIAN_POINT('Ctrl Pts',(0.759000551270414,1.08793755388759,2.36859779584929));
#27981=CARTESIAN_POINT('Ctrl Pts',(0.761051274433651,0.91584221771742,2.36074724481161));
#27982=CARTESIAN_POINT('Ctrl Pts',(0.618637433005314,0.819263404514795,
2.35289669377393));
#27983=CARTESIAN_POINT('Ctrl Pts',(0.459524343787705,0.884752183415202,
2.34504614273626));
#27984=CARTESIAN_POINT('Ctrl Pts',(0.426385402694383,1.05360877733288,2.33719559169858));
#27985=CARTESIAN_POINT('Ctrl Pts',(0.548952109888326,1.17438223097154,2.3293450406609));
#27986=CARTESIAN_POINT('Ctrl Pts',(0.717297767916034,1.1387683610531,2.32149448962322));
#27987=CARTESIAN_POINT('Ctrl Pts',(0.780449022522885,0.978702297157564,
2.31364393858554));
#27988=CARTESIAN_POINT('Ctrl Pts',(0.681768782849741,0.837737246759644,
2.30579338754786));
#27989=CARTESIAN_POINT('Ctrl Pts',(0.509756619949943,0.842292920851884,
2.29794283651019));
#27990=CARTESIAN_POINT('Ctrl Pts',(0.418676730713559,0.988284241230286,
2.29009228547251));
#27991=CARTESIAN_POINT('Ctrl Pts',(0.490211928794195,1.14478243668251,2.28224173443483));
#27992=CARTESIAN_POINT('Ctrl Pts',(0.660207644220989,1.17143634973614,2.27439118339715));
#27993=CARTESIAN_POINT('Ctrl Pts',(0.776207730757634,1.04434204382826,2.26654063235948));
#27994=CARTESIAN_POINT('Ctrl Pts',(0.734180526190243,0.87748075149375,2.2586900813218));
#27995=CARTESIAN_POINT('Ctrl Pts',(0.571817040388558,0.820497627508739,
2.25083953028412));
#27996=CARTESIAN_POINT('Ctrl Pts',(0.434728700430063,0.92449650187637,2.24298897924644));
#27997=CARTESIAN_POINT('Ctrl Pts',(0.445859592221225,1.09620870668547,2.23513842820877));
#27998=CARTESIAN_POINT('Ctrl Pts',(0.595227265578502,1.18163865695784,2.22728787717108));
#27999=CARTESIAN_POINT('Ctrl Pts',(0.748875240939872,1.10417074102503,2.21943732613341));
#28000=CARTESIAN_POINT('Ctrl Pts',(0.769008360762544,0.933280028245809,
2.21158677509573));
#28001=CARTESIAN_POINT('Ctrl Pts',(0.637570764789711,0.822225372195567,
2.20373622405805));
#28002=CARTESIAN_POINT('Ctrl Pts',(0.472438813719035,0.870603228776448,
2.19588567302037));
#28003=CARTESIAN_POINT('Ctrl Pts',(0.421706767119107,1.03502718597557,2.1880351219827));
#28004=CARTESIAN_POINT('Ctrl Pts',(0.530872330435983,1.16803793011858,2.18018457094502));
#28005=CARTESIAN_POINT('Ctrl Pts',(0.702033231237909,1.1503482635805,2.17233401990734));
#28006=CARTESIAN_POINT('Ctrl Pts',(0.781688304564893,0.997822700079642,
2.16448346886966));
#28007=CARTESIAN_POINT('Ctrl Pts',(0.698400986961052,0.847249790637147,
2.15663291783198));
#28008=CARTESIAN_POINT('Ctrl Pts',(0.526865324912526,0.833666900912216,
2.14878236679431));
#28009=CARTESIAN_POINT('Ctrl Pts',(0.420918578136115,0.969255487747401,
2.14093181575663));
#28010=CARTESIAN_POINT('Ctrl Pts',(0.475576307951429,1.13241648613165,2.13308126471895));
#28011=CARTESIAN_POINT('Ctrl Pts',(0.641820162707069,1.17682322770038,2.12523071368128));
#28012=CARTESIAN_POINT('Ctrl Pts',(0.770558701511974,1.06265070285456,2.11738016264359));
#28013=CARTESIAN_POINT('Ctrl Pts',(0.746336141641471,0.892291522696776,
2.10952961160592));
#28014=CARTESIAN_POINT('Ctrl Pts',(0.590875851708506,0.818527896169216,
2.10167906056824));
#28015=CARTESIAN_POINT('Ctrl Pts',(0.443598313494032,0.907512706568079,
2.09382850953057));
#28016=CARTESIAN_POINT('Ctrl Pts',(0.436585528693405,1.07944243843108,2.08597795849288));
#28017=CARTESIAN_POINT('Ctrl Pts',(0.57612672137744,1.18012607114374,2.07812740745521));
#28018=CARTESIAN_POINT('Ctrl Pts',(0.737078048375186,1.11926881624917,2.07027685641753));
#28019=CARTESIAN_POINT('Ctrl Pts',(0.775094502137202,0.951447557128672,
2.06242630537985));
#28020=CARTESIAN_POINT('Ctrl Pts',(0.656082084236305,0.827171040068,2.05457575434217));
#28021=CARTESIAN_POINT('Ctrl Pts',(0.48677384037764,0.857888191265152,2.04672520330449));
#28022=CARTESIAN_POINT('Ctrl Pts',(0.419009664523655,1.01606137229499,2.03887465226682));
#28023=CARTESIAN_POINT('Ctrl Pts',(0.513561617374857,1.15981701056446,2.03102410122914));
#28024=CARTESIAN_POINT('Ctrl Pts',(0.685634169421134,1.1602711276025,2.02317355019146));
#28025=CARTESIAN_POINT('Ctrl Pts',(0.780906782004492,1.01693885807272,2.01532299915378));
#28026=CARTESIAN_POINT('Ctrl Pts',(0.713940171081941,0.858516566589665,
2.0074724481161));
#28027=CARTESIAN_POINT('Ctrl Pts',(0.544785272473601,0.826780004858426,
1.99962189707843));
#28028=CARTESIAN_POINT('Ctrl Pts',(0.425151261024703,0.95079820002532,1.99177134604075));
#28029=CARTESIAN_POINT('Ctrl Pts',(0.449973151490716,1.0622497573257,1.98653764534896));
#28030=CARTESIAN_POINT('Ctrl Pts',(0.483086340557483,1.10069600903591,1.98392079500307));
#28031=CARTESIAN_POINT('Ctrl Pts',(0.562546241758482,0.859903427576914,
2.40535973499898));
#28032=CARTESIAN_POINT('Ctrl Pts',(0.516476448777934,0.872219838026409,
2.40274288465309));
#28033=CARTESIAN_POINT('Ctrl Pts',(0.438184529507143,0.945611619266206,
2.3975091839613));
#28034=CARTESIAN_POINT('Ctrl Pts',(0.46540025856266,1.1052571836823,2.38965863292362));
#28035=CARTESIAN_POINT('Ctrl Pts',(0.613546068752483,1.17019122293655,2.38180808188594));
#28036=CARTESIAN_POINT('Ctrl Pts',(0.749434413113403,1.08264686286195,2.37395753084827));
#28037=CARTESIAN_POINT('Ctrl Pts',(0.751361756194339,0.920905501875057,
2.36610697981059));
#28038=CARTESIAN_POINT('Ctrl Pts',(0.617516127087842,0.830137273999053,
2.35825642877291));
#28039=CARTESIAN_POINT('Ctrl Pts',(0.467975946780819,0.891685974065206,
2.35040587773523));
#28040=CARTESIAN_POINT('Ctrl Pts',(0.436830782981619,1.050383449079,2.34255532669756));
#28041=CARTESIAN_POINT('Ctrl Pts',(0.552023364456505,1.16389066663247,2.33470477565987));
#28042=CARTESIAN_POINT('Ctrl Pts',(0.710240643620372,1.13041947607723,2.3268542246222));
#28043=CARTESIAN_POINT('Ctrl Pts',(0.769592454630765,0.979983656034563,
2.31900367358452));
#28044=CARTESIAN_POINT('Ctrl Pts',(0.676849230889565,0.847499652630768,
2.31115312254684));
#28045=CARTESIAN_POINT('Ctrl Pts',(0.515186039121242,0.851781238316293,
2.30330257150916));
#28046=CARTESIAN_POINT('Ctrl Pts',(0.429585896947362,0.988989110277028,
2.29545202047149));
#28047=CARTESIAN_POINT('Ctrl Pts',(0.496817238327747,1.13607171976393,2.28760146943381));
#28048=CARTESIAN_POINT('Ctrl Pts',(0.65658530053649,1.16112202193283,2.27975091839613));
#28049=CARTESIAN_POINT('Ctrl Pts',(0.765606336716589,1.04167424101854,2.27190036735845));
#28050=CARTESIAN_POINT('Ctrl Pts',(0.726107664547559,0.884852021899667,
2.26404981632077));
#28051=CARTESIAN_POINT('Ctrl Pts',(0.573512645109186,0.831297240975754,
2.2561992652831));
#28052=CARTESIAN_POINT('Ctrl Pts',(0.444672113031105,0.929039108103942,
2.24834871424542));
#28053=CARTESIAN_POINT('Ctrl Pts',(0.455133323819063,1.09042038851482,2.24049816320774));
#28054=CARTESIAN_POINT('Ctrl Pts',(0.595514413242444,1.17071051568267,2.23264761217006));
#28055=CARTESIAN_POINT('Ctrl Pts',(0.739918283799722,1.09790339356867,2.22479706113239));
#28056=CARTESIAN_POINT('Ctrl Pts',(0.758840110930535,0.9372941807914,2.21694651009471));
#28057=CARTESIAN_POINT('Ctrl Pts',(0.635310350446671,0.832921037316226,
2.20909595905703));
#28058=CARTESIAN_POINT('Ctrl Pts',(0.480113428188521,0.878388279713101,
2.20124540801935));
#28059=CARTESIAN_POINT('Ctrl Pts',(0.432433633690143,1.03291980397207,2.19339485698167));
#28060=CARTESIAN_POINT('Ctrl Pts',(0.535031340151599,1.15792806545277,2.185544305944));
#28061=CARTESIAN_POINT('Ctrl Pts',(0.695894485310114,1.14130268323763,2.17769375490632));
#28062=CARTESIAN_POINT('Ctrl Pts',(0.770757176282041,0.997953695549035,
2.16984320386864));
#28063=CARTESIAN_POINT('Ctrl Pts',(0.692480772040193,0.856439882084015,
2.16199265283096));
#28064=CARTESIAN_POINT('Ctrl Pts',(0.531265412839046,0.843674195813048,
2.15414210179328));
#28065=CARTESIAN_POINT('Ctrl Pts',(0.431692865452835,0.971105206188175,
2.1462915507556));
#28066=CARTESIAN_POINT('Ctrl Pts',(0.483062157645861,1.12444975651669,2.13844099971793));
#28067=CARTESIAN_POINT('Ctrl Pts',(0.639304086812941,1.16618480278905,2.13059044868025));
#28068=CARTESIAN_POINT('Ctrl Pts',(0.760297176696446,1.05888137454499,2.12273989764257));
#28069=CARTESIAN_POINT('Ctrl Pts',(0.73753194733446,0.898771715163604,2.11488934660489));
#28070=CARTESIAN_POINT('Ctrl Pts',(0.591424798629911,0.829446016911682,
2.10703879556722));
#28071=CARTESIAN_POINT('Ctrl Pts',(0.453008093077508,0.913077128953215,
2.09918824452954));
#28072=CARTESIAN_POINT('Ctrl Pts',(0.44641722674026,1.07466284908066,2.09133769349186));
#28073=CARTESIAN_POINT('Ctrl Pts',(0.577563037665274,1.16928893335727,2.08348714245418));
#28074=CARTESIAN_POINT('Ctrl Pts',(0.728830859679466,1.11209310544222,2.0756365914165));
#28075=CARTESIAN_POINT('Ctrl Pts',(0.76456008458585,0.954368675154091,2.06778604037883));
#28076=CARTESIAN_POINT('Ctrl Pts',(0.652707951494933,0.837569153125047,
2.05993548934115));
#28077=CARTESIAN_POINT('Ctrl Pts',(0.493585999689548,0.866438232036949,
2.05208493830347));
#28078=CARTESIAN_POINT('Ctrl Pts',(0.429898800067004,1.01509505296379,2.04423438726579));
#28079=CARTESIAN_POINT('Ctrl Pts',(0.518762111987321,1.15020175080161,2.03638383622811));
#28080=CARTESIAN_POINT('Ctrl Pts',(0.680482059638507,1.15062854625939,2.02853328519044));
#28081=CARTESIAN_POINT('Ctrl Pts',(0.770022673387457,1.01591974552719,2.02068273415276));
#28082=CARTESIAN_POINT('Ctrl Pts',(0.707085053854394,0.867028801673869,
2.01283218311508));
#28083=CARTESIAN_POINT('Ctrl Pts',(0.548107221407733,0.837201644229118,
2.0049816320774));
#28084=CARTESIAN_POINT('Ctrl Pts',(0.435670892436373,0.953758386089901,
1.99713108103972));
#28085=CARTESIAN_POINT('Ctrl Pts',(0.458999394158644,1.05850455157603,1.99189738034794));
#28086=CARTESIAN_POINT('Ctrl Pts',(0.490120355280909,1.09463771598849,1.98928053000205));
#28087=CARTESIAN_POINT('Ctrl Pts',(0.564943867702687,0.868871797975679,
2.41071946999795));
#28088=CARTESIAN_POINT('Ctrl Pts',(0.521823261561601,0.880399765646142,
2.40810261965206));
#28089=CARTESIAN_POINT('Ctrl Pts',(0.448543248857163,0.949093325744624,
2.40286891896027));
#28090=CARTESIAN_POINT('Ctrl Pts',(0.474016745860739,1.09851907871609,2.3950183679226));
#28091=CARTESIAN_POINT('Ctrl Pts',(0.612678908622024,1.15929632451388,2.38716781688491));
#28092=CARTESIAN_POINT('Ctrl Pts',(0.739868274956389,1.07735617183631,2.37931726584725));
#28093=CARTESIAN_POINT('Ctrl Pts',(0.741672237955028,0.925968786032693,
2.37146671480956));
#28094=CARTESIAN_POINT('Ctrl Pts',(0.616394821170369,0.841011143483312,
2.36361616377189));
#28095=CARTESIAN_POINT('Ctrl Pts',(0.476427549773933,0.898619764715207,
2.35576561273421));
#28096=CARTESIAN_POINT('Ctrl Pts',(0.447276163268855,1.04715812082513,2.34791506169653));
#28097=CARTESIAN_POINT('Ctrl Pts',(0.555094619024684,1.15339910229339,2.34006451065885));
#28098=CARTESIAN_POINT('Ctrl Pts',(0.703183519324712,1.12207059110137,2.33221395962117));
#28099=CARTESIAN_POINT('Ctrl Pts',(0.758735886738644,0.981265014911558,
2.3243634085835));
#28100=CARTESIAN_POINT('Ctrl Pts',(0.67192967892939,0.857262058501895,2.31651285754582));
#28101=CARTESIAN_POINT('Ctrl Pts',(0.52061545829254,0.861269555780702,2.30866230650814));
#28102=CARTESIAN_POINT('Ctrl Pts',(0.440495063181165,0.989693979323769,
2.30081175547046));
#28103=CARTESIAN_POINT('Ctrl Pts',(0.5034225478613,1.12736100284536,2.29296120443278));
#28104=CARTESIAN_POINT('Ctrl Pts',(0.652962956851991,1.15080769412952,2.28511065339511));
#28105=CARTESIAN_POINT('Ctrl Pts',(0.755004942675543,1.03900643820883,2.27726010235743));
#28106=CARTESIAN_POINT('Ctrl Pts',(0.718034802904875,0.892223292305585,
2.26940955131975));
#28107=CARTESIAN_POINT('Ctrl Pts',(0.575208249829814,0.84209685444277,2.26155900028207));
#28108=CARTESIAN_POINT('Ctrl Pts',(0.454615525632148,0.933581714331513,
2.25370844924439));
#28109=CARTESIAN_POINT('Ctrl Pts',(0.4644070554169,1.08463207034418,2.24585789820672));
#28110=CARTESIAN_POINT('Ctrl Pts',(0.595801560906386,1.1597823744075,2.23800734716904));
#28111=CARTESIAN_POINT('Ctrl Pts',(0.730961326659572,1.09163604611232,2.23015679613136));
#28112=CARTESIAN_POINT('Ctrl Pts',(0.748671861098526,0.941308333336992,
2.22230624509368));
#28113=CARTESIAN_POINT('Ctrl Pts',(0.63304993610363,0.843616702436886,2.214455694056));
#28114=CARTESIAN_POINT('Ctrl Pts',(0.487788042658006,0.886173330649751,
2.20660514301833));
#28115=CARTESIAN_POINT('Ctrl Pts',(0.443160500261181,1.03081242196857,2.19875459198065));
#28116=CARTESIAN_POINT('Ctrl Pts',(0.539190349867211,1.14781820078696,2.19090404094297));
#28117=CARTESIAN_POINT('Ctrl Pts',(0.689755739382323,1.13225710289476,2.18305348990529));
#28118=CARTESIAN_POINT('Ctrl Pts',(0.759826047999188,0.998084691018425,
2.17520293886762));
#28119=CARTESIAN_POINT('Ctrl Pts',(0.686560557119336,0.865629973530885,
2.16735238782994));
#28120=CARTESIAN_POINT('Ctrl Pts',(0.535665500765565,0.853681490713878,
2.15950183679226));
#28121=CARTESIAN_POINT('Ctrl Pts',(0.442467152769555,0.972954924628952,
2.15165128575459));
#28122=CARTESIAN_POINT('Ctrl Pts',(0.490548007340293,1.11648302690173,2.1438007347169));
#28123=CARTESIAN_POINT('Ctrl Pts',(0.636788010918814,1.15554637787772,2.13595018367923));
#28124=CARTESIAN_POINT('Ctrl Pts',(0.750035651880915,1.05511204623542,2.12809963264155));
#28125=CARTESIAN_POINT('Ctrl Pts',(0.728727753027451,0.905251907630433,
2.12024908160387));
#28126=CARTESIAN_POINT('Ctrl Pts',(0.591973745551315,0.840364137654146,
2.11239853056619));
#28127=CARTESIAN_POINT('Ctrl Pts',(0.462417872660985,0.918641551338351,
2.10454797952851));
#28128=CARTESIAN_POINT('Ctrl Pts',(0.456248924787112,1.06988325973025,2.09669742849084));
#28129=CARTESIAN_POINT('Ctrl Pts',(0.578999353953109,1.15845179557081,2.08884687745316));
#28130=CARTESIAN_POINT('Ctrl Pts',(0.720583670983745,1.10491739463527,2.08099632641548));
#28131=CARTESIAN_POINT('Ctrl Pts',(0.754025667034497,0.957289793179509,
2.0731457753778));
#28132=CARTESIAN_POINT('Ctrl Pts',(0.649333818753561,0.847967266182092,
2.06529522434013));
#28133=CARTESIAN_POINT('Ctrl Pts',(0.500398159001457,0.874988272808748,
2.05744467330245));
#28134=CARTESIAN_POINT('Ctrl Pts',(0.440787935610353,1.01412873363258,2.04959412226477));
#28135=CARTESIAN_POINT('Ctrl Pts',(0.523962606599787,1.14058649103877,2.04174357122709));
#28136=CARTESIAN_POINT('Ctrl Pts',(0.675329949855879,1.14098596491627,2.03389302018941));
#28137=CARTESIAN_POINT('Ctrl Pts',(0.759138564770422,1.01490063298166,2.02604246915174));
#28138=CARTESIAN_POINT('Ctrl Pts',(0.700229936626846,0.875541036758072,
2.01819191811406));
#28139=CARTESIAN_POINT('Ctrl Pts',(0.551429170341866,0.847623283599809,
2.01034136707638));
#28140=CARTESIAN_POINT('Ctrl Pts',(0.446190523848043,0.956718572154482,
2.0024908160387));
#28141=CARTESIAN_POINT('Ctrl Pts',(0.468025636826571,1.05475934582637,1.99725711534692));
#28142=CARTESIAN_POINT('Ctrl Pts',(0.497154370004336,1.08857942294107,1.99464026500102));
#28143=CARTESIAN_POINT('Ctrl Pts',(0.567341493646892,0.877840168374445,
2.41607920499693));
#28144=CARTESIAN_POINT('Ctrl Pts',(0.527170074345269,0.888579693265874,
2.41346235465104));
#28145=CARTESIAN_POINT('Ctrl Pts',(0.458901968207183,0.952575032223043,
2.40822865395925));
#28146=CARTESIAN_POINT('Ctrl Pts',(0.482633233158821,1.09178097374987,2.40037810292158));
#28147=CARTESIAN_POINT('Ctrl Pts',(0.611811748491563,1.14840142609121,2.3925275518839));
#28148=CARTESIAN_POINT('Ctrl Pts',(0.730302136799378,1.07206548081067,2.38467700084622));
#28149=CARTESIAN_POINT('Ctrl Pts',(0.731982719715716,0.931032070190328,
2.37682644980854));
#28150=CARTESIAN_POINT('Ctrl Pts',(0.615273515252898,0.85188501296757,2.36897589877086));
#28151=CARTESIAN_POINT('Ctrl Pts',(0.484879152767046,0.905553555365211,
2.36112534773319));
#28152=CARTESIAN_POINT('Ctrl Pts',(0.457721543556091,1.04393279257125,2.35327479669551));
#28153=CARTESIAN_POINT('Ctrl Pts',(0.558165873592863,1.14290753795432,2.34542424565783));
#28154=CARTESIAN_POINT('Ctrl Pts',(0.69612639502905,1.1137217061255,2.33757369462015));
#28155=CARTESIAN_POINT('Ctrl Pts',(0.747879318846525,0.982546373788555,
2.32972314358248));
#28156=CARTESIAN_POINT('Ctrl Pts',(0.667010126969215,0.86702446437302,2.32187259254479));
#28157=CARTESIAN_POINT('Ctrl Pts',(0.526044877463838,0.870757873245112,
2.31402204150712));
#28158=CARTESIAN_POINT('Ctrl Pts',(0.451404229414968,0.99039884837051,2.30617149046944));
#28159=CARTESIAN_POINT('Ctrl Pts',(0.510027857394853,1.11865028592679,2.29832093943177));
#28160=CARTESIAN_POINT('Ctrl Pts',(0.649340613167492,1.14049336632621,2.29047038839408));
#28161=CARTESIAN_POINT('Ctrl Pts',(0.744403548634497,1.03633863539911,2.28261983735641));
#28162=CARTESIAN_POINT('Ctrl Pts',(0.709961941262192,0.899594562711502,
2.27476928631873));
#28163=CARTESIAN_POINT('Ctrl Pts',(0.576903854550442,0.852896467909786,
2.26691873528105));
#28164=CARTESIAN_POINT('Ctrl Pts',(0.464558938233191,0.938124320559086,
2.25906818424337));
#28165=CARTESIAN_POINT('Ctrl Pts',(0.473680787014737,1.07884375217354,2.2512176332057));
#28166=CARTESIAN_POINT('Ctrl Pts',(0.596088708570328,1.14885423313233,2.24336708216801));
#28167=CARTESIAN_POINT('Ctrl Pts',(0.722004369519422,1.08536869865596,2.23551653113034));
#28168=CARTESIAN_POINT('Ctrl Pts',(0.738503611266517,0.945322485882583,
2.22766598009266));
#28169=CARTESIAN_POINT('Ctrl Pts',(0.63078952176059,0.854312367557547,2.21981542905498));
#28170=CARTESIAN_POINT('Ctrl Pts',(0.495462657127491,0.893958381586401,
2.21196487801731));
#28171=CARTESIAN_POINT('Ctrl Pts',(0.453887366832218,1.02870503996507,2.20411432697962));
#28172=CARTESIAN_POINT('Ctrl Pts',(0.543349359582825,1.13770833612116,2.19626377594195));
#28173=CARTESIAN_POINT('Ctrl Pts',(0.683616993454529,1.12321152255188,2.18841322490427));
#28174=CARTESIAN_POINT('Ctrl Pts',(0.748894919716335,0.998215686487819,
2.18056267386659));
#28175=CARTESIAN_POINT('Ctrl Pts',(0.680640342198477,0.874820064977753,
2.17271212282892));
#28176=CARTESIAN_POINT('Ctrl Pts',(0.540065588692086,0.863688785614711,
2.16486157179124));
#28177=CARTESIAN_POINT('Ctrl Pts',(0.453241440086272,0.974804643069725,
2.15701102075356));
#28178=CARTESIAN_POINT('Ctrl Pts',(0.498033857034726,1.10851629728676,2.14916046971588));
#28179=CARTESIAN_POINT('Ctrl Pts',(0.634271935024686,1.14490795296639,2.1413099186782));
#28180=CARTESIAN_POINT('Ctrl Pts',(0.739774127065386,1.05134271792586,2.13345936764053));
#28181=CARTESIAN_POINT('Ctrl Pts',(0.719923558720441,0.911732100097261,
2.12560881660285));
#28182=CARTESIAN_POINT('Ctrl Pts',(0.592522692472719,0.851282258396612,
2.11775826556517));
#28183=CARTESIAN_POINT('Ctrl Pts',(0.471827652244461,0.924205973723485,
2.10990771452749));
#28184=CARTESIAN_POINT('Ctrl Pts',(0.466080622833967,1.06510367037984,2.10205716348981));
#28185=CARTESIAN_POINT('Ctrl Pts',(0.580435670240942,1.14761465778435,2.09420661245214));
#28186=CARTESIAN_POINT('Ctrl Pts',(0.712336482288025,1.09774168382831,2.08635606141445));
#28187=CARTESIAN_POINT('Ctrl Pts',(0.743491249483144,0.960210911204929,
2.07850551037678));
#28188=CARTESIAN_POINT('Ctrl Pts',(0.645959686012189,0.858365379239137,
2.0706549593391));
#28189=CARTESIAN_POINT('Ctrl Pts',(0.507210318313367,0.883538313580547,
2.06280440830142));
#28190=CARTESIAN_POINT('Ctrl Pts',(0.451677071153702,1.01316241430137,2.05495385726375));
#28191=CARTESIAN_POINT('Ctrl Pts',(0.529163101212253,1.13097123127593,2.04710330622607));
#28192=CARTESIAN_POINT('Ctrl Pts',(0.670177840073251,1.13134338357315,2.03925275518839));
#28193=CARTESIAN_POINT('Ctrl Pts',(0.748254456153389,1.01388152043613,2.03140220415071));
#28194=CARTESIAN_POINT('Ctrl Pts',(0.693374819399297,0.884053271842277,
2.02355165311304));
#28195=CARTESIAN_POINT('Ctrl Pts',(0.554751119276,0.858044922970499,2.01570110207535));
#28196=CARTESIAN_POINT('Ctrl Pts',(0.456710155259713,0.959678758219065,
2.00785055103768));
#28197=CARTESIAN_POINT('Ctrl Pts',(0.477051879494498,1.0510141400767,2.00261685034589));
#28198=CARTESIAN_POINT('Ctrl Pts',(0.504188384727762,1.08252112989365,2.));
#28199=CARTESIAN_POINT('Ctrl Pts',(0.473630671680838,1.00010094048498,2.35565803263806));
#28200=CARTESIAN_POINT('Ctrl Pts',(0.473532439388447,1.01274184176985,2.35486362065721));
#28201=CARTESIAN_POINT('Ctrl Pts',(0.475280523076927,1.02535622997532,2.35406920867636));
#28202=CARTESIAN_POINT('Ctrl Pts',(0.478988533430712,1.03736537726742,2.35327479669551));
#28203=CARTESIAN_POINT('Ctrl Pts',(0.491202986901682,1.0769243743656,2.35065794634962));
#28204=CARTESIAN_POINT('Ctrl Pts',(0.524684430247273,1.10991595615996,2.34804109600373));
#28205=CARTESIAN_POINT('Ctrl Pts',(0.564418572159433,1.12154744175234,2.34542424565783));
#28206=CARTESIAN_POINT('Ctrl Pts',(0.604152714071593,1.13317892734471,2.34280739531194));
#28207=CARTESIAN_POINT('Ctrl Pts',(0.650139554550321,1.12345031673511,2.34019054496604));
#28208=CARTESIAN_POINT('Ctrl Pts',(0.681758462092598,1.09672345604081,2.33757369462015));
#28209=CARTESIAN_POINT('Ctrl Pts',(0.713377369634875,1.06999659534652,2.33495684427426));
#28210=CARTESIAN_POINT('Ctrl Pts',(0.7306283442407,1.02627148456754,2.33233999392837));
#28211=CARTESIAN_POINT('Ctrl Pts',(0.725775632897394,0.98515527760879,2.32972314358247));
#28212=CARTESIAN_POINT('Ctrl Pts',(0.720922921554088,0.944039070650043,
2.32710629323658));
#28213=CARTESIAN_POINT('Ctrl Pts',(0.693966524261651,0.905531767511531,
2.32448944289069));
#28214=CARTESIAN_POINT('Ctrl Pts',(0.656994117364537,0.886900350754291,
2.32187259254479));
#28215=CARTESIAN_POINT('Ctrl Pts',(0.620021710467422,0.86826893399705,2.3192557421989));
#28216=CARTESIAN_POINT('Ctrl Pts',(0.57303329396563,0.869513403621081,2.31663889185301));
#28217=CARTESIAN_POINT('Ctrl Pts',(0.537098977706589,0.890075800953996,
2.31402204150712));
#28218=CARTESIAN_POINT('Ctrl Pts',(0.501164661447548,0.910638198286911,
2.31140519116123));
#28219=CARTESIAN_POINT('Ctrl Pts',(0.476284445431258,0.95051852332871,2.30878834081533));
#28220=CARTESIAN_POINT('Ctrl Pts',(0.473614942086427,0.991833925442323,
2.30617149046944));
#28221=CARTESIAN_POINT('Ctrl Pts',(0.4734403457566,0.99453612006154,2.30600033785898));
#28222=CARTESIAN_POINT('Ctrl Pts',(0.4733607599644,0.997244453495218,2.30582918524852));
#28223=CARTESIAN_POINT('Ctrl Pts',(0.473373733146151,0.999953562449677,
2.30565803263806));
#28224=CARTESIAN_POINT('Ctrl Pts',(0.560148615814278,0.850935057178148,
2.4));
#28225=CARTESIAN_POINT('Ctrl Pts',(0.550119440006157,0.854599676739477,
2.4));
#28226=CARTESIAN_POINT('Ctrl Pts',(0.540564996368976,0.859362632124605,
2.4));
#28227=CARTESIAN_POINT('Ctrl Pts',(0.531596820053353,0.865074091447543,
2.4));
#28228=CARTESIAN_POINT('Ctrl Pts',(0.527131647122934,0.867917774785653,
2.4));
#28229=CARTESIAN_POINT('Ctrl Pts',(0.522812231247153,0.870997309268362,
2.4));
#28230=CARTESIAN_POINT('Ctrl Pts',(0.518655594653448,0.874297505825464,
2.4));
#28231=CARTESIAN_POINT('Ctrl Pts',(0.515850253684945,0.876524829864272,
2.4));
#28232=CARTESIAN_POINT('Ctrl Pts',(0.513119107067925,0.878852705294647,
2.4));
#28233=CARTESIAN_POINT('Ctrl Pts',(0.510468112479774,0.881276804671575,
2.4));
#28234=CARTESIAN_POINT('Ctrl Pts',(0.508096911905004,0.883445057244236,
2.4));
#28235=CARTESIAN_POINT('Ctrl Pts',(0.505796540173907,0.885684216423859,
2.4));
#28236=CARTESIAN_POINT('Ctrl Pts',(0.503571411911721,0.887989047157772,
2.4));
#28237=CARTESIAN_POINT('Ctrl Pts',(0.496344342241171,0.895474985193744,
2.4));
#28238=CARTESIAN_POINT('Ctrl Pts',(0.489902891057215,0.903656331605307,
2.4));
#28239=CARTESIAN_POINT('Ctrl Pts',(0.484380306519488,0.912413061717332,
2.4));
#28240=CARTESIAN_POINT('Ctrl Pts',(0.482085857904318,0.91605118932619,2.4));
#28241=CARTESIAN_POINT('Ctrl Pts',(0.479950575517979,0.919788877767087,
2.4));
#28242=CARTESIAN_POINT('Ctrl Pts',(0.477986676370491,0.923618156800881,
2.4));
#28243=CARTESIAN_POINT('Ctrl Pts',(0.476502903437523,0.92651126900086,2.4));
#28244=CARTESIAN_POINT('Ctrl Pts',(0.475117212818011,0.929456979534617,
2.4));
#28245=CARTESIAN_POINT('Ctrl Pts',(0.473840374483033,0.932438138949923,
2.4));
#28246=CARTESIAN_POINT('Ctrl Pts',(0.470678069804683,0.939821481153613,
2.4));
#28247=CARTESIAN_POINT('Ctrl Pts',(0.468171071299299,0.947441891244077,
2.4));
#28248=CARTESIAN_POINT('Ctrl Pts',(0.466390209012142,0.955243589562609,
2.4));
#28249=CARTESIAN_POINT('Ctrl Pts',(0.464752055683344,0.962420100718438,
2.4));
#28250=CARTESIAN_POINT('Ctrl Pts',(0.46372877679908,0.9697505149636,2.4));
#28251=CARTESIAN_POINT('Ctrl Pts',(0.463308980593947,0.977159382735458,
2.4));
#28252=CARTESIAN_POINT('Ctrl Pts',(0.463132836556449,0.980268100410063,
2.4));
#28253=CARTESIAN_POINT('Ctrl Pts',(0.463063518093533,0.983387131233213,
2.4));
#28254=CARTESIAN_POINT('Ctrl Pts',(0.463099417336848,0.986501004293148,
2.4));
#28255=CARTESIAN_POINT('Ctrl Pts',(0.463196741723633,0.994942847577307,
2.4));
#28256=CARTESIAN_POINT('Ctrl Pts',(0.464064109534936,1.00336872849097,2.4));
#28257=CARTESIAN_POINT('Ctrl Pts',(0.46567545593174,1.01166502412979,2.4));
#28258=CARTESIAN_POINT('Ctrl Pts',(0.466871287371351,1.0178219691398,2.4));
#28259=CARTESIAN_POINT('Ctrl Pts',(0.468477485851221,1.02390757093803,2.4));
#28260=CARTESIAN_POINT('Ctrl Pts',(0.47049181446679,1.02987017308613,2.4));
#28261=CARTESIAN_POINT('Ctrl Pts',(0.471677008778134,1.0333784597143,2.4));
#28262=CARTESIAN_POINT('Ctrl Pts',(0.473001300296321,1.03683670710464,2.4));
#28263=CARTESIAN_POINT('Ctrl Pts',(0.474460926720988,1.04022911545352,2.4));
#28264=CARTESIAN_POINT('Ctrl Pts',(0.476751356878834,1.04555244631317,2.4));
#28265=CARTESIAN_POINT('Ctrl Pts',(0.479376309757289,1.05071849279536,2.4));
#28266=CARTESIAN_POINT('Ctrl Pts',(0.482333049272134,1.05568492650343,2.4));
#28267=CARTESIAN_POINT('Ctrl Pts',(0.48437450467299,1.05911395799755,2.4));
#28268=CARTESIAN_POINT('Ctrl Pts',(0.486574676429565,1.06244757032586,2.4));
#28269=CARTESIAN_POINT('Ctrl Pts',(0.4889242778747,1.06565919855071,2.4));
#28270=CARTESIAN_POINT('Ctrl Pts',(0.492216707071327,1.07015956117947,2.4));
#28271=CARTESIAN_POINT('Ctrl Pts',(0.495805971455815,1.07442716938164,2.4));
#28272=CARTESIAN_POINT('Ctrl Pts',(0.499690943915119,1.07842077967776,2.4));
#28273=CARTESIAN_POINT('Ctrl Pts',(0.501092720341441,1.07986175482692,2.4));
#28274=CARTESIAN_POINT('Ctrl Pts',(0.502533036573698,1.08126699616446,2.4));
#28275=CARTESIAN_POINT('Ctrl Pts',(0.504010178078511,1.08263575731582,2.4));
#28276=CARTESIAN_POINT('Origin',(-0.6,1.,2.15));
#28277=CARTESIAN_POINT('Origin',(0.6,1.,2.15));
#28278=CARTESIAN_POINT('Origin',(-4.61329551933804E-18,0.,7.7));
#28279=CARTESIAN_POINT('Ctrl Pts',(-0.163512932725147,-0.0319230454628249,
7.7));
#28280=CARTESIAN_POINT('Ctrl Pts',(-0.162868713187189,-0.0402193670799747,
7.7));
#28281=CARTESIAN_POINT('Ctrl Pts',(-0.161555734105899,-0.0484297746987163,
7.7));
#28282=CARTESIAN_POINT('Ctrl Pts',(-0.159632542759909,-0.0565029299462262,
7.7));
#28283=CARTESIAN_POINT('Ctrl Pts',(-0.158570730810153,-0.0609601945506607,
7.7));
#28284=CARTESIAN_POINT('Ctrl Pts',(-0.157322623531278,-0.0653756867109852,
7.7));
#28285=CARTESIAN_POINT('Ctrl Pts',(-0.155896079860197,-0.0697409359454714,
7.7));
#28286=CARTESIAN_POINT('Ctrl Pts',(-0.154356538303328,-0.0744519607383432,
7.7));
#28287=CARTESIAN_POINT('Ctrl Pts',(-0.152611566158709,-0.0790965634596896,
7.7));
#28288=CARTESIAN_POINT('Ctrl Pts',(-0.150674785237903,-0.0836580319983892,
7.7));
#28289=CARTESIAN_POINT('Ctrl Pts',(-0.147454105252843,-0.0912433144984649,
7.7));
#28290=CARTESIAN_POINT('Ctrl Pts',(-0.143701880264036,-0.0986043779779707,
7.7));
#28291=CARTESIAN_POINT('Ctrl Pts',(-0.139461085361289,-0.105692986452679,
7.7));
#28292=CARTESIAN_POINT('Ctrl Pts',(-0.137608088276184,-0.10879032342424,
7.7));
#28293=CARTESIAN_POINT('Ctrl Pts',(-0.135661951863532,-0.111834721508838,
7.7));
#28294=CARTESIAN_POINT('Ctrl Pts',(-0.13363213961135,-0.11481369464043,
7.7));
#28295=CARTESIAN_POINT('Ctrl Pts',(-0.126756583131934,-0.124904331345827,
7.7));
#28296=CARTESIAN_POINT('Ctrl Pts',(-0.118909175019161,-0.134272394153242,
7.7));
#28297=CARTESIAN_POINT('Ctrl Pts',(-0.110223618856625,-0.142769381443324,
7.7));
#28298=CARTESIAN_POINT('Ctrl Pts',(-0.105993896729624,-0.146907273649781,
7.7));
#28299=CARTESIAN_POINT('Ctrl Pts',(-0.101564626738699,-0.150838400565212,
7.7));
#28300=CARTESIAN_POINT('Ctrl Pts',(-0.0969473135927398,-0.154543558394273,
7.7));
#28301=CARTESIAN_POINT('Ctrl Pts',(-0.0930422781223282,-0.157677149790086,
7.7));
#28302=CARTESIAN_POINT('Ctrl Pts',(-0.08899818904879,-0.160651578311767,
7.7));
#28303=CARTESIAN_POINT('Ctrl Pts',(-0.0848474066780018,-0.163437744444605,
7.7));
#28304=CARTESIAN_POINT('Ctrl Pts',(-0.079772253597363,-0.166844384053503,
7.7));
#28305=CARTESIAN_POINT('Ctrl Pts',(-0.0745321224498625,-0.169974878347106,
7.7));
#28306=CARTESIAN_POINT('Ctrl Pts',(-0.0691422613850421,-0.172811109554059,
7.7));
#28307=CARTESIAN_POINT('Ctrl Pts',(-0.0615696806179204,-0.176795922823006,
7.7));
#28308=CARTESIAN_POINT('Ctrl Pts',(-0.0537018592997504,-0.18020049056539,
7.7));
#28309=CARTESIAN_POINT('Ctrl Pts',(-0.0456056057838966,-0.183040542196704,
7.7));
#28310=CARTESIAN_POINT('Ctrl Pts',(-0.0396967750000661,-0.18511327676139,
7.7));
#28311=CARTESIAN_POINT('Ctrl Pts',(-0.0336660415152703,-0.186885115293174,
7.7));
#28312=CARTESIAN_POINT('Ctrl Pts',(-0.0275371423493659,-0.188358530007864,
7.7));
#28313=CARTESIAN_POINT('Ctrl Pts',(-0.024009864278576,-0.189206503399434,
7.7));
#28314=CARTESIAN_POINT('Ctrl Pts',(-0.0204545422857024,-0.189954336779538,
7.7));
#28315=CARTESIAN_POINT('Ctrl Pts',(-0.0168840012680182,-0.190601758687094,
7.7));
#28316=CARTESIAN_POINT('Ctrl Pts',(-0.00536605034748104,-0.192690230355445,
7.7));
#28317=CARTESIAN_POINT('Ctrl Pts',(0.00633317552139851,-0.193742280465429,
7.7));
#28318=CARTESIAN_POINT('Ctrl Pts',(0.0180567949009463,-0.193791221918947,
7.7));
#28319=CARTESIAN_POINT('Ctrl Pts',(0.0247195011198704,-0.193819036070547,
7.7));
#28320=CARTESIAN_POINT('Ctrl Pts',(0.0313904746155388,-0.193522273036976,
7.7));
#28321=CARTESIAN_POINT('Ctrl Pts',(0.0380425876903635,-0.192902235229704,
7.7));
#28322=CARTESIAN_POINT('Ctrl Pts',(0.0421423475916298,-0.192520100092953,
7.7));
#28323=CARTESIAN_POINT('Ctrl Pts',(0.0462370105106329,-0.192014780875721,
7.7));
#28324=CARTESIAN_POINT('Ctrl Pts',(0.0503137405327971,-0.191386921964521,
7.7));
#28325=CARTESIAN_POINT('Ctrl Pts',(0.0635704399020003,-0.189345252099999,
7.7));
#28326=CARTESIAN_POINT('Ctrl Pts',(0.0765507573577913,-0.186026204674558,
7.7));
#28327=CARTESIAN_POINT('Ctrl Pts',(0.0890404097591069,-0.181462425248743,
7.7));
#28328=CARTESIAN_POINT('Ctrl Pts',(0.0993752126604044,-0.177686038257715,
7.7));
#28329=CARTESIAN_POINT('Ctrl Pts',(0.10937505445883,-0.17305651193581,7.7));
#28330=CARTESIAN_POINT('Ctrl Pts',(0.118916725392593,-0.167565356836862,
7.7));
#28331=CARTESIAN_POINT('Ctrl Pts',(0.120071034691086,-0.166901061093047,
7.7));
#28332=CARTESIAN_POINT('Ctrl Pts',(0.121218627187633,-0.166224125239918,
7.7));
#28333=CARTESIAN_POINT('Ctrl Pts',(0.122359422806361,-0.16553471763581,
7.7));
#28334=CARTESIAN_POINT('Ctrl Pts',(0.188262750966371,-0.0823232180103171,
7.7));
#28335=CARTESIAN_POINT('Ctrl Pts',(0.190918677948539,-0.0742706170903244,
7.7));
#28336=CARTESIAN_POINT('Ctrl Pts',(0.193028141056754,-0.0660604186529042,
7.7));
#28337=CARTESIAN_POINT('Ctrl Pts',(0.194603503553809,-0.057743966976229,
7.7));
#28338=CARTESIAN_POINT('Ctrl Pts',(0.195790000725462,-0.0514803632589782,
7.7));
#28339=CARTESIAN_POINT('Ctrl Pts',(0.196673340762519,-0.0451564294165951,
7.7));
#28340=CARTESIAN_POINT('Ctrl Pts',(0.197255694122567,-0.038794370326094,
7.7));
#28341=CARTESIAN_POINT('Ctrl Pts',(0.197691802090699,-0.0340300041294915,
7.7));
#28342=CARTESIAN_POINT('Ctrl Pts',(0.197958654381779,-0.0292456271837883,
7.7));
#28343=CARTESIAN_POINT('Ctrl Pts',(0.198057134112497,-0.0244628264544613,
7.7));
#28344=CARTESIAN_POINT('Ctrl Pts',(0.1982631637461,-0.0144567198712174,
7.7));
#28345=CARTESIAN_POINT('Ctrl Pts',(0.197734824507455,-0.00444255766703843,
7.7));
#28346=CARTESIAN_POINT('Ctrl Pts',(0.196479778415613,0.00549131122160059,
7.7));
#28347=CARTESIAN_POINT('Ctrl Pts',(0.195824459991882,0.0106782500471663,
7.7));
#28348=CARTESIAN_POINT('Ctrl Pts',(0.194969728524037,0.0158462023683286,
7.7));
#28349=CARTESIAN_POINT('Ctrl Pts',(0.193921197678987,0.020957521647447,
7.7));
#28350=CARTESIAN_POINT('Ctrl Pts',(0.191354737801022,0.0334683561310013,
7.7));
#28351=CARTESIAN_POINT('Ctrl Pts',(0.187627993625845,0.0456724030605818,
7.7));
#28352=CARTESIAN_POINT('Ctrl Pts',(0.182754547435098,0.0573811610434715,
7.7));
#28353=CARTESIAN_POINT('Ctrl Pts',(0.180516962808123,0.0627570974625973,
7.7));
#28354=CARTESIAN_POINT('Ctrl Pts',(0.178037027139388,0.0680282734604574,
7.7));
#28355=CARTESIAN_POINT('Ctrl Pts',(0.17531313072872,0.0731739851680651,
7.7));
#28356=CARTESIAN_POINT('Ctrl Pts',(0.173532663111309,0.0765374658893014,
7.7));
#28357=CARTESIAN_POINT('Ctrl Pts',(0.171646852120024,0.0798490434275999,
7.7));
#28358=CARTESIAN_POINT('Ctrl Pts',(0.169658294487776,0.0830968889931883,
7.7));
#28359=CARTESIAN_POINT('Ctrl Pts',(0.165386261266014,0.0900742598927501,
7.7));
#28360=CARTESIAN_POINT('Ctrl Pts',(0.160657770577514,0.0967310568420072,
7.7));
#28361=CARTESIAN_POINT('Ctrl Pts',(0.155474920208509,0.103014960516334,
7.7));
#28362=CARTESIAN_POINT('Ctrl Pts',(0.149769902176698,0.109931962015469,
7.7));
#28363=CARTESIAN_POINT('Ctrl Pts',(0.143514168159607,0.116397450963363,
7.7));
#28364=CARTESIAN_POINT('Ctrl Pts',(0.136780000787126,0.122378418898736,
7.7));
#28365=CARTESIAN_POINT('Ctrl Pts',(0.13253962121023,0.126144522840088,7.7));
#28366=CARTESIAN_POINT('Ctrl Pts',(0.128109373210913,0.129718271038147,
7.7));
#28367=CARTESIAN_POINT('Ctrl Pts',(0.123506439942429,0.133088658006456,
7.7));
#28368=CARTESIAN_POINT('Ctrl Pts',(0.120698151327833,0.135144959672763,
7.7));
#28369=CARTESIAN_POINT('Ctrl Pts',(0.117828933115805,0.137122882548733,
7.7));
#28370=CARTESIAN_POINT('Ctrl Pts',(0.11490983233649,0.139016243048957,7.7));
#28371=CARTESIAN_POINT('Ctrl Pts',(0.10629614374237,0.144603175114098,7.7));
#28372=CARTESIAN_POINT('Ctrl Pts',(0.0972315481938087,0.14946836034174,
7.7));
#28373=CARTESIAN_POINT('Ctrl Pts',(0.087825129619459,0.153560681874093,
7.7));
#28374=CARTESIAN_POINT('Ctrl Pts',(0.0790043519078121,0.157398216667612,
7.7));
#28375=CARTESIAN_POINT('Ctrl Pts',(0.0698823201879155,0.160556069597663,
7.7));
#28376=CARTESIAN_POINT('Ctrl Pts',(0.0605484824963349,0.162970283178604,
7.7));
#28377=CARTESIAN_POINT('Ctrl Pts',(0.0570499058412824,0.163875196200845,
7.7));
#28378=CARTESIAN_POINT('Ctrl Pts',(0.0535300157362907,0.164673163118735,
7.7));
#28379=CARTESIAN_POINT('Ctrl Pts',(0.0499970990922767,0.165361152486414,
7.7));
#28380=CARTESIAN_POINT('Ctrl Pts',(0.0389156579059496,0.167519118406066,
7.7));
#28381=CARTESIAN_POINT('Ctrl Pts',(0.027694369523137,0.1686015574444,7.7));
#28382=CARTESIAN_POINT('Ctrl Pts',(0.0164838938501993,0.168511920108317,
7.7));
#28383=CARTESIAN_POINT('Ctrl Pts',(0.0102987918414279,0.168462464930531,
7.7));
#28384=CARTESIAN_POINT('Ctrl Pts',(0.00411708598692211,0.168055390254949,
7.7));
#28385=CARTESIAN_POINT('Ctrl Pts',(-0.00203360988862401,0.167267947758606,
7.7));
#28386=CARTESIAN_POINT('Ctrl Pts',(-0.00310929540839016,0.167130233179946,
7.7));
#28387=CARTESIAN_POINT('Ctrl Pts',(-0.00418402611025386,0.166980872543433,
7.7));
#28388=CARTESIAN_POINT('Ctrl Pts',(-0.00525764907570514,0.166819936918742,
7.7));
#28389=CARTESIAN_POINT('Origin',(0.,0.,8.75459252805377));
#28390=CARTESIAN_POINT('Ctrl Pts',(-0.205656479110814,0.000149599810560778,
8.57959252805377));
#28391=CARTESIAN_POINT('Ctrl Pts',(-0.205738361598484,0.00997856061592459,
8.57905813053169));
#28392=CARTESIAN_POINT('Ctrl Pts',(-0.200629066917608,0.0878617486383526,
8.57481913665734));
#28393=CARTESIAN_POINT('Ctrl Pts',(-0.101094553526346,0.220843047088143,
8.56687554643072));
#28394=CARTESIAN_POINT('Ctrl Pts',(0.130699637719291,0.204687395831059,
8.55576175737394));
#28395=CARTESIAN_POINT('Ctrl Pts',(0.242861169103291,0.00121341226084251,
8.5446479683171));
#28396=CARTESIAN_POINT('Ctrl Pts',(0.132730025418579,-0.203388545171364,
8.53353417926033));
#28397=CARTESIAN_POINT('Ctrl Pts',(-0.0988908732032454,-0.221817926612619,
8.5224203902035));
#28398=CARTESIAN_POINT('Ctrl Pts',(-0.200214859662634,-0.089261959020885,
8.51443983980133));
#28399=CARTESIAN_POINT('Ctrl Pts',(-0.205728077932475,-0.0106740791790422,
8.51016388575142));
#28400=CARTESIAN_POINT('Ctrl Pts',(-0.205637856381221,-0.000160393794940828,
8.50959252805377));
#28401=CARTESIAN_POINT('Ctrl Pts',(-0.205267617401664,-0.000235214789251429,
8.58540747194623));
#28402=CARTESIAN_POINT('Ctrl Pts',(-0.204912371893322,0.0467865688130083,
8.58286245525962));
#28403=CARTESIAN_POINT('Ctrl Pts',(-0.165653744048178,0.162957645782203,
8.57661284222074));
#28404=CARTESIAN_POINT('Ctrl Pts',(0.027212997215315,0.241280498724425,
8.56665863282958));
#28405=CARTESIAN_POINT('Ctrl Pts',(0.217474198098902,0.108094945242369,
8.5555448437728));
#28406=CARTESIAN_POINT('Ctrl Pts',(0.208761552554325,-0.124138522922833,
8.54443105471596));
#28407=CARTESIAN_POINT('Ctrl Pts',(0.00892537992430322,-0.24269250748312,
8.53331726565919));
#28408=CARTESIAN_POINT('Ctrl Pts',(-0.172124770298785,-0.152545548970925,
8.52364273806925));
#28409=CARTESIAN_POINT('Ctrl Pts',(-0.204991280139091,-0.0417919262244986,
8.51767280683161));
#28410=CARTESIAN_POINT('Ctrl Pts',(-0.205208153945529,0.00011616087473525,
8.51540747194623));
#28411=CARTESIAN_POINT('Ctrl Pts',(0.126907087985233,0.107935865304858,
8.6));
#28412=CARTESIAN_POINT('Ctrl Pts',(0.162798331100656,0.0657362393039593,
8.59629540364773));
#28413=CARTESIAN_POINT('Ctrl Pts',(0.188528583981656,-0.0565786457595969,
8.5888862109432));
#28414=CARTESIAN_POINT('Ctrl Pts',(0.0545086267819675,-0.189344482047467,
8.57777242188639));
#28415=CARTESIAN_POINT('Ctrl Pts',(-0.129420383958987,-0.148353651561752,
8.56665863282959));
#28416=CARTESIAN_POINT('Ctrl Pts',(-0.194878571858316,0.0282081923545751,
8.55554484377279));
#28417=CARTESIAN_POINT('Ctrl Pts',(-0.0819678920427756,0.179060477648788,
8.54443105471597));
#28418=CARTESIAN_POINT('Ctrl Pts',(0.105971819657057,0.165961407205034,
8.53331726565919));
#28419=CARTESIAN_POINT('Ctrl Pts',(0.196912864205418,0.00098383979878997,
8.52220347660236));
#28420=CARTESIAN_POINT('Ctrl Pts',(0.107618066600488,-0.164908293590701,
8.51108968754557));
#28421=CARTESIAN_POINT('Ctrl Pts',(-0.0801811387062207,-0.179850914094962,
8.49997589848876));
#28422=CARTESIAN_POINT('Ctrl Pts',(-0.194589451459316,-0.0301775235439226,
8.48886210943196));
#28423=CARTESIAN_POINT('Ctrl Pts',(-0.130887926765565,0.147119496537145,
8.47774832037516));
#28424=CARTESIAN_POINT('Ctrl Pts',(0.0526168491933447,0.189755465499352,
8.46663453131834));
#28425=CARTESIAN_POINT('Ctrl Pts',(0.187960802408794,0.0587065624392284,
8.45552074226155));
#28426=CARTESIAN_POINT('Ctrl Pts',(0.151262113639308,-0.126077353665056,
8.44440695320474));
#28427=CARTESIAN_POINT('Ctrl Pts',(-0.0238885092637228,-0.195461121852156,
8.43329316414793));
#28428=CARTESIAN_POINT('Ctrl Pts',(-0.177173705652972,-0.0859371671587494,
8.42217937509113));
#28429=CARTESIAN_POINT('Ctrl Pts',(-0.168289801519644,0.102246080788216,
8.41106558603433));
#28430=CARTESIAN_POINT('Ctrl Pts',(-0.00536833273875009,0.196842316537561,
8.39995179697752));
#28431=CARTESIAN_POINT('Ctrl Pts',(0.162466831485467,0.111266555129785,
8.38883800792072));
#28432=CARTESIAN_POINT('Ctrl Pts',(0.181594262550234,-0.0761527498248231,
8.37772421886392));
#28433=CARTESIAN_POINT('Ctrl Pts',(0.0345064055837472,-0.193868577324089,
8.36661042980711));
#28434=CARTESIAN_POINT('Ctrl Pts',(-0.144165555692373,-0.134134298342242,
8.3554966407503));
#28435=CARTESIAN_POINT('Ctrl Pts',(-0.190881148920086,0.0483746255840866,
8.34438285169351));
#28436=CARTESIAN_POINT('Ctrl Pts',(-0.0628810617889658,0.186605705863002,
8.3332690626367));
#28437=CARTESIAN_POINT('Ctrl Pts',(0.122674774310876,0.154034467436257,
8.3221552735799));
#28438=CARTESIAN_POINT('Ctrl Pts',(0.195944998260667,-0.019526265966773,
8.31104148452309));
#28439=CARTESIAN_POINT('Ctrl Pts',(0.0898645431334079,-0.175214386656136,
8.29992769546628));
#28440=CARTESIAN_POINT('Ctrl Pts',(-0.0984699474562653,-0.170526792188656,
8.28881390640949));
#28441=CARTESIAN_POINT('Ctrl Pts',(-0.19667377841448,-0.00975409091757148,
8.27770011735268));
#28442=CARTESIAN_POINT('Ctrl Pts',(-0.114859869557362,0.159946640385262,
8.26658632829587));
#28443=CARTESIAN_POINT('Ctrl Pts',(0.0720865805050185,0.183246397827218,
8.25547253923907));
#28444=CARTESIAN_POINT('Ctrl Pts',(0.193051365913784,0.0388186491814046,
8.24435875018227));
#28445=CARTESIAN_POINT('Ctrl Pts',(0.13731404675024,-0.141140249293057,
8.23324496112546));
#28446=CARTESIAN_POINT('Ctrl Pts',(-0.0441083766509897,-0.19191187695055,
8.22213117206866));
#28447=CARTESIAN_POINT('Ctrl Pts',(-0.185157902680562,-0.0670243872063616,
8.21101738301184));
#28448=CARTESIAN_POINT('Ctrl Pts',(-0.156730300553177,0.119211284255993,
8.19990359395506));
#28449=CARTESIAN_POINT('Ctrl Pts',(0.0151543231130278,0.196331515290955,
8.18878980489823));
#28450=CARTESIAN_POINT('Ctrl Pts',(0.173168022972167,0.0937472838292696,
8.17767601584145));
#28451=CARTESIAN_POINT('Ctrl Pts',(0.17267906754593,-0.0946448996878474,
8.16656222678463));
#28452=CARTESIAN_POINT('Ctrl Pts',(0.014135003281085,-0.196407533174517,
8.15544843772784));
#28453=CARTESIAN_POINT('Ctrl Pts',(-0.157346989788777,-0.118396124133627,
8.14433464867103));
#28454=CARTESIAN_POINT('Ctrl Pts',(-0.184807498668741,0.0679846000301397,
8.13322085961422));
#28455=CARTESIAN_POINT('Ctrl Pts',(-0.0431116081576236,0.192138248788519,
8.12210707055742));
#28456=CARTESIAN_POINT('Ctrl Pts',(0.138044826219057,0.14042557943482,8.11099328150061));
#28457=CARTESIAN_POINT('Ctrl Pts',(0.192847265622626,-0.0398202153099506,
8.09987949244382));
#28458=CARTESIAN_POINT('Ctrl Pts',(0.0711344157650659,-0.183618115389575,
8.08876570338701));
#28459=CARTESIAN_POINT('Ctrl Pts',(-0.115688571561406,-0.159348272082047,
8.0776519143302));
#28460=CARTESIAN_POINT('Ctrl Pts',(-0.196620497340079,0.0107748517944625,
8.06653812527341));
#28461=CARTESIAN_POINT('Ctrl Pts',(-0.0975834520752944,0.171035631628434,
8.05542433621659));
#28462=CARTESIAN_POINT('Ctrl Pts',(0.0907728335456545,0.174745558156785,
8.0443105471598));
#28463=CARTESIAN_POINT('Ctrl Pts',(0.196043715188255,0.0185088935550664,
8.03319675810298));
#28464=CARTESIAN_POINT('Ctrl Pts',(0.121873561032224,-0.154669171223235,
8.02208296904619));
#28465=CARTESIAN_POINT('Ctrl Pts',(-0.0638488456770328,-0.186276789512212,
8.01096917998937));
#28466=CARTESIAN_POINT('Ctrl Pts',(-0.19112967984246,-0.0473831498401582,
7.99985539093258));
#28467=CARTESIAN_POINT('Ctrl Pts',(-0.143467350491047,0.134880824245969,
7.98874160187577));
#28468=CARTESIAN_POINT('Ctrl Pts',(0.0355122717971353,0.193686850239423,
7.97762781281897));
#28469=CARTESIAN_POINT('Ctrl Pts',(0.181987108969079,0.075209105665833,
7.96651402376217));
#28470=CARTESIAN_POINT('Ctrl Pts',(0.161887081434908,-0.112108386283467,
7.95540023470535));
#28471=CARTESIAN_POINT('Ctrl Pts',(-0.00639002767582873,-0.196811800811433,
7.94428644564855));
#28472=CARTESIAN_POINT('Ctrl Pts',(-0.168818271957638,-0.101371142179071,
7.93317265659175));
#28473=CARTESIAN_POINT('Ctrl Pts',(-0.176725237445514,0.086855672754766,
7.92205886753494));
#28474=CARTESIAN_POINT('Ctrl Pts',(-0.0228735887833459,0.195582504933715,
7.91094507847814));
#28475=CARTESIAN_POINT('Ctrl Pts',(0.151914514866951,0.125290453226829,
7.89983128942133));
#28476=CARTESIAN_POINT('Ctrl Pts',(0.18765354068678,-0.0596813730664067,
7.88871750036453));
#28477=CARTESIAN_POINT('Ctrl Pts',(0.0516311516775647,-0.190026158074923,
7.87760371130772));
#28478=CARTESIAN_POINT('Ctrl Pts',(-0.131649814209033,-0.146437852861883,
7.86648992225093));
#28479=CARTESIAN_POINT('Ctrl Pts',(-0.194430215690457,0.0311866942884203,
7.85537613319412));
#28480=CARTESIAN_POINT('Ctrl Pts',(-0.0792464287188404,0.180265677725562,
7.84426234413731));
#28481=CARTESIAN_POINT('Ctrl Pts',(0.108472499205164,0.164345499013512,
7.83314855508052));
#28482=CARTESIAN_POINT('Ctrl Pts',(0.196905346153373,-0.00200209185834237,
7.8220347660237));
#28483=CARTESIAN_POINT('Ctrl Pts',(0.105108441749456,-0.166516920998775,
7.8109209769669));
#28484=CARTESIAN_POINT('Ctrl Pts',(-0.0828953023872357,-0.17861736891036,
7.7998071879101));
#28485=CARTESIAN_POINT('Ctrl Pts',(-0.195024252374675,-0.0272264307646135,
7.78869339885329));
#28486=CARTESIAN_POINT('Ctrl Pts',(-0.128644863563789,0.149083417534189,
7.77757960979649));
#28487=CARTESIAN_POINT('Ctrl Pts',(0.0554837771323393,0.188938995522239,
7.76646582073968));
#28488=CARTESIAN_POINT('Ctrl Pts',(0.188829174678946,0.0558496805756237,
7.75535203168288));
#28489=CARTESIAN_POINT('Ctrl Pts',(0.149333740426706,-0.128345818837516,
7.74423824262607));
#28490=CARTESIAN_POINT('Ctrl Pts',(-0.0268419213711513,-0.195092032740585,
7.73312445356928));
#28491=CARTESIAN_POINT('Ctrl Pts',(-0.178462040649008,-0.0832145415948537,
7.72201066451247));
#28492=CARTESIAN_POINT('Ctrl Pts',(-0.166707642915459,0.104723462076886,
7.71089687545566));
#28493=CARTESIAN_POINT('Ctrl Pts',(-0.00241652804585203,0.197019500729453,
7.69978308639886));
#28494=CARTESIAN_POINT('Ctrl Pts',(0.164199550234369,0.108548043911206,
7.68866929734206));
#28495=CARTESIAN_POINT('Ctrl Pts',(0.174839538171075,-0.0159901738299269,
7.68126010463752));
#28496=CARTESIAN_POINT('Ctrl Pts',(0.15264423560529,-0.0667480137268267,
7.67755550828525));
#28497=CARTESIAN_POINT('Ctrl Pts',(0.136778062465877,0.116331236980981,
8.60748149723825));
#28498=CARTESIAN_POINT('Ctrl Pts',(0.17546096639785,0.0708492771249706,
8.60377690088598));
#28499=CARTESIAN_POINT('Ctrl Pts',(0.203192546971425,-0.0609793957674089,
8.59636770818145));
#28500=CARTESIAN_POINT('Ctrl Pts',(0.0587483684109172,-0.204071906496436,
8.58525391912464));
#28501=CARTESIAN_POINT('Ctrl Pts',(-0.139486845396373,-0.159892763615499,
8.57414013006784));
#28502=CARTESIAN_POINT('Ctrl Pts',(-0.210036443969145,0.0304022569359761,
8.56302634101102));
#28503=CARTESIAN_POINT('Ctrl Pts',(-0.0883434458706326,0.19298800079524,
8.55191255195424));
#28504=CARTESIAN_POINT('Ctrl Pts',(0.114214425677802,0.178870070080376,
8.54079876289742));
#28505=CARTESIAN_POINT('Ctrl Pts',(0.212228965838042,0.00106036395280743,
8.52968497384062));
#28506=CARTESIAN_POINT('Ctrl Pts',(0.115988719539852,-0.177735044117588,
8.51857118478382));
#28507=CARTESIAN_POINT('Ctrl Pts',(-0.0864177168718956,-0.193839918267514,
8.50745739572701));
#28508=CARTESIAN_POINT('Ctrl Pts',(-0.209724835463879,-0.0325247648960035,
8.49634360667021));
#28509=CARTESIAN_POINT('Ctrl Pts',(-0.141068535315007,0.15856261464015,
8.4852298176134));
#28510=CARTESIAN_POINT('Ctrl Pts',(0.0567094462569527,0.204514856698406,
8.4741160285566));
#28511=CARTESIAN_POINT('Ctrl Pts',(0.202580602716201,0.0632728241735722,
8.46300223949979));
#28512=CARTESIAN_POINT('Ctrl Pts',(0.163027449108952,-0.135883790487243,
8.45188845044298));
#28513=CARTESIAN_POINT('Ctrl Pts',(-0.0257465840889073,-0.210664305349561,
8.44077466138619));
#28514=CARTESIAN_POINT('Ctrl Pts',(-0.190954473574659,-0.092621455620727,
8.42966087232938));
#28515=CARTESIAN_POINT('Ctrl Pts',(-0.181379569494986,0.110198894695063,
8.41854708327258));
#28516=CARTESIAN_POINT('Ctrl Pts',(-0.00578588763114495,0.212152930894099,
8.40743329421577));
#28517=CARTESIAN_POINT('Ctrl Pts',(0.175103682373818,0.1199209915657,8.39631950515897));
#28518=CARTESIAN_POINT('Ctrl Pts',(0.195718866305016,-0.082075995421942,
8.38520571610216));
#28519=CARTESIAN_POINT('Ctrl Pts',(0.0371903521965286,-0.208947890936482,
8.37409192704536));
#28520=CARTESIAN_POINT('Ctrl Pts',(-0.155378912990374,-0.144567413284328,
8.36297813798855));
#28521=CARTESIAN_POINT('Ctrl Pts',(-0.205728097027866,0.0521372577761262,
8.35186434893175));
#28522=CARTESIAN_POINT('Ctrl Pts',(-0.067772020726633,0.201120105253607,
8.34075055987495));
#28523=CARTESIAN_POINT('Ctrl Pts',(0.132216554725712,0.166015439668319,
8.32963677081815));
#28524=CARTESIAN_POINT('Ctrl Pts',(0.211185818203411,-0.0210450406555653,
8.31852298176134));
#28525=CARTESIAN_POINT('Ctrl Pts',(0.0968543072676843,-0.188842756566615,
8.30740919270453));
#28526=CARTESIAN_POINT('Ctrl Pts',(-0.106129049511812,-0.183790555786764,
8.29629540364774));
#28527=CARTESIAN_POINT('Ctrl Pts',(-0.211971283688315,-0.0105127749600295,
8.28518161459092));
#28528=CARTESIAN_POINT('Ctrl Pts',(-0.123793797986818,0.172387468006265,
8.27406782553413));
#28529=CARTESIAN_POINT('Ctrl Pts',(0.0776935549290535,0.197499506501754,
8.26295403647731));
#28530=CARTESIAN_POINT('Ctrl Pts',(0.20806711591358,0.0418380068983455,
8.25184024742052));
#28531=CARTESIAN_POINT('Ctrl Pts',(0.147994486060795,-0.152118294893832,
8.24072645836371));
#28532=CARTESIAN_POINT('Ctrl Pts',(-0.0475391752550459,-0.206838996231168,
8.22961266930691));
#28533=CARTESIAN_POINT('Ctrl Pts',(-0.199559690329035,-0.0722376186042153,
8.2184988802501));
#28534=CARTESIAN_POINT('Ctrl Pts',(-0.168920957684039,0.128483670561418,
8.2073850911933));
#28535=CARTESIAN_POINT('Ctrl Pts',(0.0163330432231097,0.211602398958294,
8.19627130213649));
#28536=CARTESIAN_POINT('Ctrl Pts',(0.186637224438839,0.101039051854205,
8.1851575130797));
#28537=CARTESIAN_POINT('Ctrl Pts',(0.186110237515614,-0.102006485272812,
8.17404372402288));
#28538=CARTESIAN_POINT('Ctrl Pts',(0.0152344395607012,-0.211684329597404,
8.16292993496609));
#28539=CARTESIAN_POINT('Ctrl Pts',(-0.169585613694417,-0.127605106377914,
8.15181614590927));
#28540=CARTESIAN_POINT('Ctrl Pts',(-0.199182031503369,0.0732725178496109,
8.14070235685248));
#28541=CARTESIAN_POINT('Ctrl Pts',(-0.0464648769994157,0.20708297552252,
8.12958856779566));
#28542=CARTESIAN_POINT('Ctrl Pts',(0.148782106369649,0.151348037218991,
8.11847477873887));
#28543=CARTESIAN_POINT('Ctrl Pts',(0.207847140474726,-0.0429174759545572,
8.10736098968206));
#28544=CARTESIAN_POINT('Ctrl Pts',(0.0766673297563964,-0.197900136669627,
8.09624720062525));
#28545=CARTESIAN_POINT('Ctrl Pts',(-0.124686957354622,-0.171742557950773,
8.08513341156845));
#28546=CARTESIAN_POINT('Ctrl Pts',(-0.211913858352676,0.0116129317534655,
8.07401962251165));
#28547=CARTESIAN_POINT('Ctrl Pts',(-0.105173601533932,0.184338973324224,
8.06290583345484));
#28548=CARTESIAN_POINT('Ctrl Pts',(0.0978332455186183,0.188337462065038,
8.05179204439804));
#28549=CARTESIAN_POINT('Ctrl Pts',(0.211292213443444,0.0199485358859052,
8.04067825534123));
#28550=CARTESIAN_POINT('Ctrl Pts',(0.131353022186941,-0.166699511421921,
8.02956446628443));
#28551=CARTESIAN_POINT('Ctrl Pts',(-0.06881507992212,-0.200765605423151,
8.01845067722763));
#28552=CARTESIAN_POINT('Ctrl Pts',(-0.205995958961859,-0.0510686639458728,
8.00733688817082));
#28553=CARTESIAN_POINT('Ctrl Pts',(-0.154626400611774,0.145372004803316,
7.99622309911402));
#28554=CARTESIAN_POINT('Ctrl Pts',(0.0382744558029648,0.208752028917009,
7.98510931005722));
#28555=CARTESIAN_POINT('Ctrl Pts',(0.19614226875534,0.0810589535705133,
7.97399552100041));
#28556=CARTESIAN_POINT('Ctrl Pts',(0.174478838719386,-0.120828301283006,
7.96288173194361));
#28557=CARTESIAN_POINT('Ctrl Pts',(-0.0068870511370089,-0.212120041620846,
7.95176794288681));
#28558=CARTESIAN_POINT('Ctrl Pts',(-0.181949144951542,-0.109255902387577,
7.94065415382999));
#28559=CARTESIAN_POINT('Ctrl Pts',(-0.190471123011129,0.0936114036037888,
7.9295403647732));
#28560=CARTESIAN_POINT('Ctrl Pts',(-0.0246527219645235,0.210795129742235,
7.91842657571639));
#28561=CARTESIAN_POINT('Ctrl Pts',(0.163730594829841,0.135035684057547,
7.90731278665958));
#28562=CARTESIAN_POINT('Ctrl Pts',(0.202249441835637,-0.0643234566557557,
7.89619899760278));
#28563=CARTESIAN_POINT('Ctrl Pts',(0.055647080091861,-0.204806604043635,
7.88508520854598));
#28564=CARTESIAN_POINT('Ctrl Pts',(-0.141889683211386,-0.157827951961535,
7.87397141948916));
#28565=CARTESIAN_POINT('Ctrl Pts',(-0.209553214159777,0.033612430063655,
7.86285763043237));
#28566=CARTESIAN_POINT('Ctrl Pts',(-0.0854103041018835,0.194286942674705,
7.85174384137556));
#28567=CARTESIAN_POINT('Ctrl Pts',(0.116909610863029,0.177128474752108,
7.84063005231877));
#28568=CARTESIAN_POINT('Ctrl Pts',(0.212220863023546,-0.00215781679030121,
7.82951626326195));
#28569=CARTESIAN_POINT('Ctrl Pts',(0.113283893276087,-0.179468792354972,
7.81840247420515));
#28570=CARTESIAN_POINT('Ctrl Pts',(-0.0893429912233777,-0.192510426566203,
7.80728868514835));
#28571=CARTESIAN_POINT('Ctrl Pts',(-0.210193455678128,-0.0293441328373914,
7.79617489609154));
#28572=CARTESIAN_POINT('Ctrl Pts',(-0.138651004162113,0.160679291597098,
7.78506110703474));
#28573=CARTESIAN_POINT('Ctrl Pts',(0.0597993670403417,0.203634880778195,
7.77394731797793));
#28574=CARTESIAN_POINT('Ctrl Pts',(0.203516517947542,0.0601937308604925,
7.76283352892113));
#28575=CARTESIAN_POINT('Ctrl Pts',(0.160949084882664,-0.13832869940436,
7.75171973986433));
#28576=CARTESIAN_POINT('Ctrl Pts',(-0.02892971587556,-0.210266508076299,
7.74060595080753));
#28577=CARTESIAN_POINT('Ctrl Pts',(-0.192343016699888,-0.0896870612117004,
7.72949216175072));
#28578=CARTESIAN_POINT('Ctrl Pts',(-0.179674348834503,0.112868969456315,
7.71837837269391));
#28579=CARTESIAN_POINT('Ctrl Pts',(-0.00260448828551292,0.212343896669543,
7.7072645836371));
#28580=CARTESIAN_POINT('Ctrl Pts',(0.176971173914563,0.116991031520346,
7.69615079458031));
#28581=CARTESIAN_POINT('Ctrl Pts',(0.188438751949387,-0.0172339073386072,
7.68874160187577));
#28582=CARTESIAN_POINT('Ctrl Pts',(0.164517074058983,-0.071939748487992,
7.6850370055235));
#28583=CARTESIAN_POINT('Ctrl Pts',(0.146649036946521,0.124726608657104,
8.6149629944765));
#28584=CARTESIAN_POINT('Ctrl Pts',(0.188123601695045,0.0759623149459817,
8.61125839812423));
#28585=CARTESIAN_POINT('Ctrl Pts',(0.217856509961195,-0.0653801457752205,
8.60384920541969));
#28586=CARTESIAN_POINT('Ctrl Pts',(0.0629881100398666,-0.218799330945407,
8.59273541636289));
#28587=CARTESIAN_POINT('Ctrl Pts',(-0.149553306833759,-0.171431875669247,
8.58162162730608));
#28588=CARTESIAN_POINT('Ctrl Pts',(-0.225194316079973,0.0325963215173767,
8.57050783824928));
#28589=CARTESIAN_POINT('Ctrl Pts',(-0.0947189996984894,0.206915523941692,
8.55939404919247));
#28590=CARTESIAN_POINT('Ctrl Pts',(0.122457031698546,0.191778732955717,
8.54828026013568));
#28591=CARTESIAN_POINT('Ctrl Pts',(0.227545067470666,0.00113688810682507,
8.53716647107886));
#28592=CARTESIAN_POINT('Ctrl Pts',(0.124359372479216,-0.190561794644476,
8.52605268202208));
#28593=CARTESIAN_POINT('Ctrl Pts',(-0.0926542950375705,-0.207828922440066,
8.51493889296525));
#28594=CARTESIAN_POINT('Ctrl Pts',(-0.224860219468443,-0.0348720062480843,
8.50382510390846));
#28595=CARTESIAN_POINT('Ctrl Pts',(-0.15124914386445,0.170005732743154,
8.49271131485166));
#28596=CARTESIAN_POINT('Ctrl Pts',(0.0608020433205606,0.219274247897461,
8.48159752579484));
#28597=CARTESIAN_POINT('Ctrl Pts',(0.217200403023608,0.0678390859079159,
8.47048373673806));
#28598=CARTESIAN_POINT('Ctrl Pts',(0.174792784578596,-0.14569022730943,
8.45936994768122));
#28599=CARTESIAN_POINT('Ctrl Pts',(-0.0276046589140918,-0.225867488846965,
8.44825615862445));
#28600=CARTESIAN_POINT('Ctrl Pts',(-0.204735241496347,-0.0993057440827045,
8.43714236956762));
#28601=CARTESIAN_POINT('Ctrl Pts',(-0.194469337470328,0.118151708601909,
8.42602858051083));
#28602=CARTESIAN_POINT('Ctrl Pts',(-0.00620344252353972,0.227463545250637,
8.41491479145402));
#28603=CARTESIAN_POINT('Ctrl Pts',(0.187740533262168,0.128575428001615,
8.40380100239722));
#28604=CARTESIAN_POINT('Ctrl Pts',(0.209843470059799,-0.0879992410190609,
8.39268721334041));
#28605=CARTESIAN_POINT('Ctrl Pts',(0.0398742988093101,-0.224027204548875,
8.38157342428361));
#28606=CARTESIAN_POINT('Ctrl Pts',(-0.166592270288375,-0.155000528226414,
8.3704596352268));
#28607=CARTESIAN_POINT('Ctrl Pts',(-0.220575045135645,0.0558998899681659,
8.35934584617));
#28608=CARTESIAN_POINT('Ctrl Pts',(-0.0726629796643001,0.215634504644212,
8.3482320571132));
#28609=CARTESIAN_POINT('Ctrl Pts',(0.141758335140549,0.17799641190038,8.3371182680564));
#28610=CARTESIAN_POINT('Ctrl Pts',(0.226426638146155,-0.0225638153443574,
8.32600447899959));
#28611=CARTESIAN_POINT('Ctrl Pts',(0.10384407140196,-0.202471126477093,
8.31489068994278));
#28612=CARTESIAN_POINT('Ctrl Pts',(-0.113788151567359,-0.197054319384871,
8.30377690088599));
#28613=CARTESIAN_POINT('Ctrl Pts',(-0.22726878896215,-0.0112714590024876,
8.29266311182917));
#28614=CARTESIAN_POINT('Ctrl Pts',(-0.132727726416275,0.184828295627267,
8.28154932277238));
#28615=CARTESIAN_POINT('Ctrl Pts',(0.0833005293530883,0.21175261517629,
8.27043553371557));
#28616=CARTESIAN_POINT('Ctrl Pts',(0.223082865913377,0.0448573646152865,
8.25932174465876));
#28617=CARTESIAN_POINT('Ctrl Pts',(0.158674925371351,-0.163096340494608,
8.24820795560196));
#28618=CARTESIAN_POINT('Ctrl Pts',(-0.050969973859102,-0.221766115511785,
8.23709416654516));
#28619=CARTESIAN_POINT('Ctrl Pts',(-0.213961477977508,-0.0774508500020691,
8.22598037748835));
#28620=CARTESIAN_POINT('Ctrl Pts',(-0.181111614814901,0.137756056866844,
8.21486658843155));
#28621=CARTESIAN_POINT('Ctrl Pts',(0.0175117633331917,0.226873282625633,
8.20375279937474));
#28622=CARTESIAN_POINT('Ctrl Pts',(0.200106425905512,0.108330819879141,
8.19263901031794));
#28623=CARTESIAN_POINT('Ctrl Pts',(0.199541407485298,-0.109368070857775,
8.18152522126113));
#28624=CARTESIAN_POINT('Ctrl Pts',(0.0163338758403174,-0.226961126020292,
8.17041143220434));
#28625=CARTESIAN_POINT('Ctrl Pts',(-0.181824237600056,-0.136814088622201,
8.15929764314752));
#28626=CARTESIAN_POINT('Ctrl Pts',(-0.213556564337998,0.0785604356690821,
8.14818385409073));
#28627=CARTESIAN_POINT('Ctrl Pts',(-0.0498181458412077,0.22202770225652,
8.13707006503391));
#28628=CARTESIAN_POINT('Ctrl Pts',(0.159519386520241,0.162270495003162,
8.12595627597712));
#28629=CARTESIAN_POINT('Ctrl Pts',(0.222847015326826,-0.0460147365991637,
8.1148424869203));
#28630=CARTESIAN_POINT('Ctrl Pts',(0.0822002437477268,-0.212182157949678,
8.10372869786351));
#28631=CARTESIAN_POINT('Ctrl Pts',(-0.133685343147839,-0.1841368438195,
8.09261490880669));
#28632=CARTESIAN_POINT('Ctrl Pts',(-0.227207219365272,0.0124510117124686,
8.0815011197499));
#28633=CARTESIAN_POINT('Ctrl Pts',(-0.11276375099257,0.197642315020013,
8.07038733069309));
#28634=CARTESIAN_POINT('Ctrl Pts',(0.104893657491582,0.201929365973291,
8.05927354163629));
#28635=CARTESIAN_POINT('Ctrl Pts',(0.226540711698633,0.0213881782167439,
8.04815975257947));
#28636=CARTESIAN_POINT('Ctrl Pts',(0.140832483341659,-0.178729851620607,
8.03704596352269));
#28637=CARTESIAN_POINT('Ctrl Pts',(-0.0737813141672074,-0.21525442133409,
8.02593217446587));
#28638=CARTESIAN_POINT('Ctrl Pts',(-0.220862238081258,-0.0547541780515873,
8.01481838540908));
#28639=CARTESIAN_POINT('Ctrl Pts',(-0.165785450732502,0.155863185360662,
8.00370459635226));
#28640=CARTESIAN_POINT('Ctrl Pts',(0.0410366398087944,0.223817207594595,
7.99259080729547));
#28641=CARTESIAN_POINT('Ctrl Pts',(0.2102974285416,0.0869088014751938,7.98147701823866));
#28642=CARTESIAN_POINT('Ctrl Pts',(0.187070596003864,-0.129548216282546,
7.97036322918185));
#28643=CARTESIAN_POINT('Ctrl Pts',(-0.00738407459818899,-0.227428282430258,
7.95924944012505));
#28644=CARTESIAN_POINT('Ctrl Pts',(-0.195080017945446,-0.117140662596084,
7.94813565106825));
#28645=CARTESIAN_POINT('Ctrl Pts',(-0.204217008576744,0.100367134452811,
7.93702186201144));
#28646=CARTESIAN_POINT('Ctrl Pts',(-0.026431855145701,0.226007754550755,
7.92590807295464));
#28647=CARTESIAN_POINT('Ctrl Pts',(0.175546674792731,0.144780914888265,
7.91479428389783));
#28648=CARTESIAN_POINT('Ctrl Pts',(0.216845342984493,-0.0689655402451044,
7.90368049484103));
#28649=CARTESIAN_POINT('Ctrl Pts',(0.0596630085061574,-0.219587050012348,
7.89256670578422));
#28650=CARTESIAN_POINT('Ctrl Pts',(-0.152129552213739,-0.169218051061186,
7.88145291672742));
#28651=CARTESIAN_POINT('Ctrl Pts',(-0.224676212629098,0.0360381658388899,
7.87033912767062));
#28652=CARTESIAN_POINT('Ctrl Pts',(-0.0915741794849265,0.208308207623847,
7.8592253386138));
#28653=CARTESIAN_POINT('Ctrl Pts',(0.125346722520894,0.189911450490704,
7.84811154955702));
#28654=CARTESIAN_POINT('Ctrl Pts',(0.227536379893719,-0.0023135417222602,
7.8369977605002));
#28655=CARTESIAN_POINT('Ctrl Pts',(0.121459344802718,-0.192420663711169,
7.8258839714434));
#28656=CARTESIAN_POINT('Ctrl Pts',(-0.0957906800595197,-0.206403484222046,
7.8147701823866));
#28657=CARTESIAN_POINT('Ctrl Pts',(-0.22536265898158,-0.0314618349101691,
7.80365639332978));
#28658=CARTESIAN_POINT('Ctrl Pts',(-0.148657144760437,0.172275165660006,
7.79254260427299));
#28659=CARTESIAN_POINT('Ctrl Pts',(0.0641149569483445,0.218330766034152,
7.78142881521618));
#28660=CARTESIAN_POINT('Ctrl Pts',(0.218203861216137,0.0645377811453611,
7.77031502615938));
#28661=CARTESIAN_POINT('Ctrl Pts',(0.172564429338623,-0.148311579971203,
7.75920123710257));
#28662=CARTESIAN_POINT('Ctrl Pts',(-0.0310175103799688,-0.225440983412014,
7.74808744804577));
#28663=CARTESIAN_POINT('Ctrl Pts',(-0.206223992750769,-0.0961595808285469,
7.73697365898897));
#28664=CARTESIAN_POINT('Ctrl Pts',(-0.192641054753548,0.121014476835745,
7.72585986993216));
#28665=CARTESIAN_POINT('Ctrl Pts',(-0.00279244852517366,0.227668292609634,
7.71474608087536));
#28666=CARTESIAN_POINT('Ctrl Pts',(0.189742797594757,0.125434019129486,
7.70363229181855));
#28667=CARTESIAN_POINT('Ctrl Pts',(0.2020379657277,-0.0184776408472874,
7.69622309911402));
#28668=CARTESIAN_POINT('Ctrl Pts',(0.176389912512676,-0.0771314832491572,
7.69251850276175));
#28669=CARTESIAN_POINT('Ctrl Pts',(0.156520011427165,0.133121980333227,
8.62244449171475));
#28670=CARTESIAN_POINT('Ctrl Pts',(0.20078623699224,0.081075352766993,8.61873989536248));
#28671=CARTESIAN_POINT('Ctrl Pts',(0.232520472950965,-0.0697808957830323,
8.61133070265794));
#28672=CARTESIAN_POINT('Ctrl Pts',(0.0672278516688162,-0.233526755394377,
8.60021691360114));
#28673=CARTESIAN_POINT('Ctrl Pts',(-0.159619768271145,-0.182970987722995,
8.58910312454432));
#28674=CARTESIAN_POINT('Ctrl Pts',(-0.240352188190802,0.0347903860987775,
8.57798933548754));
#28675=CARTESIAN_POINT('Ctrl Pts',(-0.101094553526346,0.220843047088143,
8.56687554643072));
#28676=CARTESIAN_POINT('Ctrl Pts',(0.130699637719291,0.204687395831059,
8.55576175737394));
#28677=CARTESIAN_POINT('Ctrl Pts',(0.242861169103291,0.00121341226084251,
8.5446479683171));
#28678=CARTESIAN_POINT('Ctrl Pts',(0.132730025418579,-0.203388545171364,
8.53353417926033));
#28679=CARTESIAN_POINT('Ctrl Pts',(-0.0988908732032454,-0.221817926612619,
8.5224203902035));
#28680=CARTESIAN_POINT('Ctrl Pts',(-0.239995603473007,-0.0372192476001651,
8.51130660114671));
#28681=CARTESIAN_POINT('Ctrl Pts',(-0.161429752413892,0.181448850846158,
8.5001928120899));
#28682=CARTESIAN_POINT('Ctrl Pts',(0.0648946403841687,0.234033639096515,
8.48907902303309));
#28683=CARTESIAN_POINT('Ctrl Pts',(0.231820203331014,0.0724053476422597,
8.4779652339763));
#28684=CARTESIAN_POINT('Ctrl Pts',(0.18655812004824,-0.155496664131617,
8.46685144491948));
#28685=CARTESIAN_POINT('Ctrl Pts',(-0.0294627337392764,-0.241070672344369,
8.45573765586269));
#28686=CARTESIAN_POINT('Ctrl Pts',(-0.218516009418034,-0.105990032544682,
8.44462386680588));
#28687=CARTESIAN_POINT('Ctrl Pts',(-0.207559105445671,0.126104522508756,
8.43351007774908));
#28688=CARTESIAN_POINT('Ctrl Pts',(-0.00662099741593451,0.242774159607174,
8.42239628869227));
#28689=CARTESIAN_POINT('Ctrl Pts',(0.200377384150519,0.13722986443753,8.41128249963547));
#28690=CARTESIAN_POINT('Ctrl Pts',(0.223968073814581,-0.0939224866161797,
8.40016871057866));
#28691=CARTESIAN_POINT('Ctrl Pts',(0.0425582454220915,-0.239106518161268,
8.38905492152186));
#28692=CARTESIAN_POINT('Ctrl Pts',(-0.177805627586376,-0.1654336431685,
8.37794113246506));
#28693=CARTESIAN_POINT('Ctrl Pts',(-0.235421993243425,0.0596625221602054,
8.36682734340825));
#28694=CARTESIAN_POINT('Ctrl Pts',(-0.0775539386019673,0.230148904034816,
8.35571355435145));
#28695=CARTESIAN_POINT('Ctrl Pts',(0.151300115555386,0.189977384132442,
8.34459976529464));
#28696=CARTESIAN_POINT('Ctrl Pts',(0.241667458088899,-0.0240825900331494,
8.33348597623784));
#28697=CARTESIAN_POINT('Ctrl Pts',(0.110833835536237,-0.216099496387572,
8.32237218718103));
#28698=CARTESIAN_POINT('Ctrl Pts',(-0.121447253622906,-0.210318082982978,
8.31125839812424));
#28699=CARTESIAN_POINT('Ctrl Pts',(-0.242566294235986,-0.012030143044946,
8.30014460906742));
#28700=CARTESIAN_POINT('Ctrl Pts',(-0.141661654845732,0.19726912324827,
8.28903082001063));
#28701=CARTESIAN_POINT('Ctrl Pts',(0.088907503777123,0.226005723850825,
8.27791703095381));
#28702=CARTESIAN_POINT('Ctrl Pts',(0.238098615913173,0.0478767223322276,
8.26680324189701));
#28703=CARTESIAN_POINT('Ctrl Pts',(0.169355364681906,-0.174074386095383,
8.2556894528402));
#28704=CARTESIAN_POINT('Ctrl Pts',(-0.0544007724631579,-0.236693234792403,
8.24457566378341));
#28705=CARTESIAN_POINT('Ctrl Pts',(-0.228363265625981,-0.0826640813999228,
8.2334618747266));
#28706=CARTESIAN_POINT('Ctrl Pts',(-0.193302271945763,0.14702844317227,
8.2223480856698));
#28707=CARTESIAN_POINT('Ctrl Pts',(0.0186904834432735,0.242144166292971,
8.21123429661299));
#28708=CARTESIAN_POINT('Ctrl Pts',(0.213575627372185,0.115622587904077,
8.20012050755619));
#28709=CARTESIAN_POINT('Ctrl Pts',(0.212972577454982,-0.11672965644274,
8.18900671849938));
#28710=CARTESIAN_POINT('Ctrl Pts',(0.0174333121199337,-0.24223792244318,
8.17789292944259));
#28711=CARTESIAN_POINT('Ctrl Pts',(-0.194062861505696,-0.146023070866488,
8.16677914038577));
#28712=CARTESIAN_POINT('Ctrl Pts',(-0.227931097172626,0.0838483534885532,
8.15566535132898));
#28713=CARTESIAN_POINT('Ctrl Pts',(-0.0531714146829997,0.236972428990521,
8.14455156227216));
#28714=CARTESIAN_POINT('Ctrl Pts',(0.170256666670833,0.173192952787333,
8.13343777321537));
#28715=CARTESIAN_POINT('Ctrl Pts',(0.237846890178926,-0.0491119972437703,
8.12232398415856));
#28716=CARTESIAN_POINT('Ctrl Pts',(0.0877331577390571,-0.22646417922973,
8.11121019510175));
#28717=CARTESIAN_POINT('Ctrl Pts',(-0.142683728941055,-0.196531129688227,
8.10009640604495));
#28718=CARTESIAN_POINT('Ctrl Pts',(-0.242500580377868,0.0132890916714718,
8.08898261698815));
#28719=CARTESIAN_POINT('Ctrl Pts',(-0.120353900451207,0.210945656715802,
8.07786882793134));
#28720=CARTESIAN_POINT('Ctrl Pts',(0.111954069464546,0.215521269881544,
8.06675503887454));
#28721=CARTESIAN_POINT('Ctrl Pts',(0.241789209953822,0.0228278205475825,
8.05564124981773));
#28722=CARTESIAN_POINT('Ctrl Pts',(0.150311944496376,-0.190760191819292,
8.04452746076093));
#28723=CARTESIAN_POINT('Ctrl Pts',(-0.0787475484122947,-0.229743237245029,
8.03341367170412));
#28724=CARTESIAN_POINT('Ctrl Pts',(-0.235728517200657,-0.0584396921573019,
8.02229988264732));
#28725=CARTESIAN_POINT('Ctrl Pts',(-0.176944500853229,0.166354365918009,
8.01118609359052));
#28726=CARTESIAN_POINT('Ctrl Pts',(0.043798823814624,0.238882386272181,
8.00007230453372));
#28727=CARTESIAN_POINT('Ctrl Pts',(0.224452588327861,0.0927586493798742,
7.98895851547691));
#28728=CARTESIAN_POINT('Ctrl Pts',(0.199662353288342,-0.138268131282085,
7.9778447264201));
#28729=CARTESIAN_POINT('Ctrl Pts',(-0.00788109805936929,-0.242736523239671,
7.96673093736331));
#28730=CARTESIAN_POINT('Ctrl Pts',(-0.20821089093935,-0.12502542280459,
7.95561714830649));
#28731=CARTESIAN_POINT('Ctrl Pts',(-0.217962894142359,0.107122865301834,
7.9445033592497));
#28732=CARTESIAN_POINT('Ctrl Pts',(-0.0282109883268786,0.241220379359275,
7.93338957019289));
#28733=CARTESIAN_POINT('Ctrl Pts',(0.187362754755622,0.154526145718984,
7.92227578113608));
#28734=CARTESIAN_POINT('Ctrl Pts',(0.23144124413335,-0.0736076238344533,
7.91116199207928));
#28735=CARTESIAN_POINT('Ctrl Pts',(0.0636789369204538,-0.234367495981061,
7.90004820302247));
#28736=CARTESIAN_POINT('Ctrl Pts',(-0.162369421216092,-0.180608150160837,
7.88893441396567));
#28737=CARTESIAN_POINT('Ctrl Pts',(-0.239799211098419,0.0384639016141247,
7.87782062490887));
#28738=CARTESIAN_POINT('Ctrl Pts',(-0.0977380548679695,0.222329472572989,
7.86670683585206));
#28739=CARTESIAN_POINT('Ctrl Pts',(0.133783834178758,0.2026944262293,7.85559304679526));
#28740=CARTESIAN_POINT('Ctrl Pts',(0.242851896763891,-0.00246926665421919,
7.84447925773846));
#28741=CARTESIAN_POINT('Ctrl Pts',(0.129634796329349,-0.205372535067366,
7.83336546868165));
#28742=CARTESIAN_POINT('Ctrl Pts',(-0.102238368895662,-0.220296541877889,
7.82225167962484));
#28743=CARTESIAN_POINT('Ctrl Pts',(-0.240531862285032,-0.033579536982947,
7.81113789056804));
#28744=CARTESIAN_POINT('Ctrl Pts',(-0.158663285358761,0.183871039722915,
7.80002410151124));
#28745=CARTESIAN_POINT('Ctrl Pts',(0.0684305468563471,0.233026651290108,
7.78891031245443));
#28746=CARTESIAN_POINT('Ctrl Pts',(0.232891204484732,0.0688818314302299,
7.77779652339763));
#28747=CARTESIAN_POINT('Ctrl Pts',(0.184179773794582,-0.158294460538047,
7.76668273434082));
#28748=CARTESIAN_POINT('Ctrl Pts',(-0.0331053048843776,-0.240615458747729,
7.75556894528403));
#28749=CARTESIAN_POINT('Ctrl Pts',(-0.22010496880165,-0.102632100445394,
7.74445515622721));
#28750=CARTESIAN_POINT('Ctrl Pts',(-0.205607760672592,0.129159984215175,
7.73334136717041));
#28751=CARTESIAN_POINT('Ctrl Pts',(-0.00298040876483471,0.242992688549725,
7.7222275781136));
#28752=CARTESIAN_POINT('Ctrl Pts',(0.202514421274951,0.133877006738626,
7.7111137890568));
#28753=CARTESIAN_POINT('Ctrl Pts',(0.215637179506012,-0.0197213743559677,
7.70370459635227));
#28754=CARTESIAN_POINT('Ctrl Pts',(0.188262750966369,-0.0823232180103224,
7.7));
#28755=CARTESIAN_POINT('Ctrl Pts',(0.126907087985233,0.107935865304858,
8.6));
#28756=CARTESIAN_POINT('Ctrl Pts',(0.135119342222632,0.100274703694019,
8.6));
#28757=CARTESIAN_POINT('Ctrl Pts',(0.142437014324932,0.0917732077732832,
8.6));
#28758=CARTESIAN_POINT('Ctrl Pts',(0.14885561179134,0.0826255492913934,
8.6));
#28759=CARTESIAN_POINT('Ctrl Pts',(0.153626284694708,0.0758264803861984,
8.6));
#28760=CARTESIAN_POINT('Ctrl Pts',(0.157899939952193,0.0686691570742025,
8.6));
#28761=CARTESIAN_POINT('Ctrl Pts',(0.161664554366084,0.0612188846220726,
8.6));
#28762=CARTESIAN_POINT('Ctrl Pts',(0.163881899847797,0.0568306987036657,
8.6));
#28763=CARTESIAN_POINT('Ctrl Pts',(0.165924040766234,0.0523356709836805,
8.6));
#28764=CARTESIAN_POINT('Ctrl Pts',(0.167776061733539,0.0477755770655923,
8.6));
#28765=CARTESIAN_POINT('Ctrl Pts',(0.172334880242679,0.0365507362434885,
8.6));
#28766=CARTESIAN_POINT('Ctrl Pts',(0.175760680768791,0.0249077723450597,
8.6));
#28767=CARTESIAN_POINT('Ctrl Pts',(0.178025304432692,0.0130451206803074,
8.6));
#28768=CARTESIAN_POINT('Ctrl Pts',(0.179464454318053,0.00550650220893073,
8.6));
#28769=CARTESIAN_POINT('Ctrl Pts',(0.180433932781852,-0.002121718043742,
8.6));
#28770=CARTESIAN_POINT('Ctrl Pts',(0.180916947576875,-0.00979373217332476,
8.6));
#28771=CARTESIAN_POINT('Ctrl Pts',(0.181142367724244,-0.0133742157807179,
8.6));
#28772=CARTESIAN_POINT('Ctrl Pts',(0.181261291825179,-0.0169607842651116,
8.6));
#28773=CARTESIAN_POINT('Ctrl Pts',(0.181272571985224,-0.0205386416225958,
8.6));
#28774=CARTESIAN_POINT('Ctrl Pts',(0.181307739490319,-0.0316931213770327,
8.6));
#28775=CARTESIAN_POINT('Ctrl Pts',(0.18030100776568,-0.0427900713202343,
8.6));
#28776=CARTESIAN_POINT('Ctrl Pts',(0.178218613078485,-0.0536884200006557,
8.6));
#28777=CARTESIAN_POINT('Ctrl Pts',(0.177058261266385,-0.0597611970385473,
8.6));
#28778=CARTESIAN_POINT('Ctrl Pts',(0.175563380683853,-0.0657725480180776,
8.6));
#28779=CARTESIAN_POINT('Ctrl Pts',(0.173752707611816,-0.0717063254815672,
8.6));
#28780=CARTESIAN_POINT('Ctrl Pts',(0.172620016542247,-0.0754182803592885,
8.6));
#28781=CARTESIAN_POINT('Ctrl Pts',(0.171363093867741,-0.0791013962971504,
8.6));
#28782=CARTESIAN_POINT('Ctrl Pts',(0.169987642094878,-0.0827468570145976,
8.6));
#28783=CARTESIAN_POINT('Ctrl Pts',(0.165605788263354,-0.094360405615556,
8.6));
#28784=CARTESIAN_POINT('Ctrl Pts',(0.160056570352909,-0.10551119017211,
8.6));
#28785=CARTESIAN_POINT('Ctrl Pts',(0.153505449982331,-0.116076623215971,
8.6));
#28786=CARTESIAN_POINT('Ctrl Pts',(0.14916461185782,-0.123077385217648,
8.6));
#28787=CARTESIAN_POINT('Ctrl Pts',(0.144382694364319,-0.129821293390769,
8.6));
#28788=CARTESIAN_POINT('Ctrl Pts',(0.139196287888346,-0.136270468973621,
8.6));
#28789=CARTESIAN_POINT('Ctrl Pts',(0.136485946091972,-0.139640715832468,
8.6));
#28790=CARTESIAN_POINT('Ctrl Pts',(0.133663744041843,-0.142931788522251,
8.6));
#28791=CARTESIAN_POINT('Ctrl Pts',(0.130738055024136,-0.146133486419774,
8.6));
#28792=CARTESIAN_POINT('Ctrl Pts',(0.124471671826875,-0.15299103887539,
8.6));
#28793=CARTESIAN_POINT('Ctrl Pts',(0.117755782354928,-0.159412890827526,
8.6));
#28794=CARTESIAN_POINT('Ctrl Pts',(0.110644485105481,-0.165348276025604,
8.6));
#28795=CARTESIAN_POINT('Ctrl Pts',(0.106128056396711,-0.169117875743616,
8.6));
#28796=CARTESIAN_POINT('Ctrl Pts',(0.101451886306371,-0.172691180761178,
8.6));
#28797=CARTESIAN_POINT('Ctrl Pts',(0.0966276544344934,-0.176053779769394,
8.6));
#28798=CARTESIAN_POINT('Ctrl Pts',(0.0925453919559805,-0.178899209285654,
8.6));
#28799=CARTESIAN_POINT('Ctrl Pts',(0.0883640473887971,-0.181588757784238,
8.6));
#28800=CARTESIAN_POINT('Ctrl Pts',(0.0840946504162302,-0.184112638937655,
8.6));
#28801=CARTESIAN_POINT('Ctrl Pts',(0.0753694926585074,-0.189270571396691,
8.6));
#28802=CARTESIAN_POINT('Ctrl Pts',(0.0662731702050655,-0.193740352082781,
8.6));
#28803=CARTESIAN_POINT('Ctrl Pts',(0.0568645195540229,-0.197448127710951,
8.6));
#28804=CARTESIAN_POINT('Ctrl Pts',(0.0556251889131679,-0.197936525050361,
8.6));
#28805=CARTESIAN_POINT('Ctrl Pts',(0.0543804239234686,-0.19841168092438,
8.6));
#28806=CARTESIAN_POINT('Ctrl Pts',(0.0531304158592269,-0.198873653475084,
8.6));
#28807=CARTESIAN_POINT('Ctrl Pts',(-0.166732044643443,-0.000130047968060085,
8.48714803633902));
#28808=CARTESIAN_POINT('Ctrl Pts',(-0.166805196659206,-0.00865458859339771,
8.48771939403667));
#28809=CARTESIAN_POINT('Ctrl Pts',(-0.166207891524911,-0.0171688432130046,
8.48829075173431));
#28810=CARTESIAN_POINT('Ctrl Pts',(-0.164904478551508,-0.0255735852889172,
8.48886210943196));
#28811=CARTESIAN_POINT('Ctrl Pts',(-0.156453347208284,-0.0800686537276021,
8.49256670578422));
#28812=CARTESIAN_POINT('Ctrl Pts',(-0.118317242957253,-0.129959783911282,
8.49627130213649));
#28813=CARTESIAN_POINT('Ctrl Pts',(-0.0679493232806182,-0.152414912252412,
8.49997589848876));
#28814=CARTESIAN_POINT('Ctrl Pts',(-0.0175814036039843,-0.174870040593541,
8.50368049484103));
#28815=CARTESIAN_POINT('Ctrl Pts',(0.045018331498252,-0.169889167092121,
8.5073850911933));
#28816=CARTESIAN_POINT('Ctrl Pts',(0.0912006653168583,-0.139750041443162,
8.51108968754557));
#28817=CARTESIAN_POINT('Ctrl Pts',(0.137382999135465,-0.109610915794204,
8.51479428389784));
#28818=CARTESIAN_POINT('Ctrl Pts',(0.167147931670441,-0.054313537997707,
8.5184988802501));
#28819=CARTESIAN_POINT('Ctrl Pts',(0.16687355717987,0.000831412134915374,
8.52220347660237));
#28820=CARTESIAN_POINT('Ctrl Pts',(0.166599182689298,0.0559763622675381,
8.52590807295464));
#28821=CARTESIAN_POINT('Ctrl Pts',(0.136285501173178,0.110968884736286,
8.52961266930691));
#28822=CARTESIAN_POINT('Ctrl Pts',(0.0898053751318118,0.140648324377953,
8.53331726565918));
#28823=CARTESIAN_POINT('Ctrl Pts',(0.0433252490904463,0.170327764019619,
8.53702186201145));
#28824=CARTESIAN_POINT('Ctrl Pts',(-0.0193213214761645,0.174694120834203,
8.54072645836371));
#28825=CARTESIAN_POINT('Ctrl Pts',(-0.0694630533953934,0.15173525169246,
8.54443105471598));
#28826=CARTESIAN_POINT('Ctrl Pts',(-0.119604785314622,0.128776382550717,
8.54813565106824));
#28827=CARTESIAN_POINT('Ctrl Pts',(-0.157241678586469,0.078492287452646,
8.55184024742051));
#28828=CARTESIAN_POINT('Ctrl Pts',(-0.165150427239171,0.023923265917556,
8.55554484377278));
#28829=CARTESIAN_POINT('Ctrl Pts',(-0.166291284509671,0.0160515446508695,
8.55607924129486));
#28830=CARTESIAN_POINT('Ctrl Pts',(-0.166813534699148,0.00809065919753236,
8.55661363881694));
#28831=CARTESIAN_POINT('Ctrl Pts',(-0.166747144031447,0.000121296159821427,
8.55714803633902));
#28832=CARTESIAN_POINT('Ctrl Pts',(-0.0530170217188485,-0.198517432567176,
8.6));
#28833=CARTESIAN_POINT('Ctrl Pts',(-0.119028790974543,-0.180888011517996,
8.59629540364773));
#28834=CARTESIAN_POINT('Ctrl Pts',(-0.230934959138857,-0.074861353976339,
8.5888862109432));
#28835=CARTESIAN_POINT('Ctrl Pts',(-0.188121058383465,0.153833707952583,
8.57777242188639));
#28836=CARTESIAN_POINT('Ctrl Pts',(0.027212997215315,0.241280498724425,
8.56665863282958));
#28837=CARTESIAN_POINT('Ctrl Pts',(0.217474198098902,0.108094945242369,
8.5555448437728));
#28838=CARTESIAN_POINT('Ctrl Pts',(0.208761552554325,-0.124138522922833,
8.54443105471596));
#28839=CARTESIAN_POINT('Ctrl Pts',(0.00892537992430322,-0.24269250748312,
8.53331726565919));
#28840=CARTESIAN_POINT('Ctrl Pts',(-0.199059264243693,-0.139134553701345,
8.52220347660236));
#28841=CARTESIAN_POINT('Ctrl Pts',(-0.22485330991897,0.0917885826081383,
8.51108968754558));
#28842=CARTESIAN_POINT('Ctrl Pts',(-0.0448312245259985,0.238689656539759,
8.49997589848875));
#28843=CARTESIAN_POINT('Ctrl Pts',(0.176222693303572,0.167118876029215,
8.48886210943197));
#28844=CARTESIAN_POINT('Ctrl Pts',(0.235979340716847,-0.0574194692648986,
8.47774832037514));
#28845=CARTESIAN_POINT('Ctrl Pts',(0.0797407360187229,-0.229400234578822,
8.46663453131836));
#28846=CARTESIAN_POINT('Ctrl Pts',(-0.149485123105517,-0.191408811645189,
8.45552074226153));
#28847=CARTESIAN_POINT('Ctrl Pts',(-0.241885728018762,0.0217814932194586,
8.44440695320475));
#28848=CARTESIAN_POINT('Ctrl Pts',(-0.112885495048793,0.215034836414334,
8.43329316414793));
#28849=CARTESIAN_POINT('Ctrl Pts',(0.119440067448933,0.211464412612195,
8.42217937509113));
#28850=CARTESIAN_POINT('Ctrl Pts',(0.242440804004482,0.0143381848173731,
8.41106558603433));
#28851=CARTESIAN_POINT('Ctrl Pts',(0.143532711926644,-0.195911931545135,
8.39995179697752));
#28852=CARTESIAN_POINT('Ctrl Pts',(-0.0867524934706339,-0.226841642534413,
8.38883800792072));
#28853=CARTESIAN_POINT('Ctrl Pts',(-0.23763216061734,-0.0501406218404715,
8.37772421886392));
#28854=CARTESIAN_POINT('Ctrl Pts',(-0.17100441477528,0.172454676785586,
8.36661042980711));
#28855=CARTESIAN_POINT('Ctrl Pts',(0.05214561050461,0.237200254924533,8.35549664075031));
#28856=CARTESIAN_POINT('Ctrl Pts',(0.22756616748523,0.0848337492213278,
8.3443828516935));
#28857=CARTESIAN_POINT('Ctrl Pts',(0.19469283040568,-0.145182048984365,
8.3332690626367));
#28858=CARTESIAN_POINT('Ctrl Pts',(-0.016385062217743,-0.242311071399234,
8.3221552735799));
#28859=CARTESIAN_POINT('Ctrl Pts',(-0.212465521621073,-0.117650022106929,
8.31104148452309));
#28860=CARTESIAN_POINT('Ctrl Pts',(-0.214073879538015,0.114697426631087,
8.29992769546629));
#28861=CARTESIAN_POINT('Ctrl Pts',(-0.0197379877628579,0.242061020031891,
8.28881390640948));
#28862=CARTESIAN_POINT('Ctrl Pts',(0.19266430806168,0.147863416631009,8.27770011735268));
#28863=CARTESIAN_POINT('Ctrl Pts',(0.22871877775246,-0.0816752488934883,
8.26658632829587));
#28864=CARTESIAN_POINT('Ctrl Pts',(0.0554243563205898,-0.236455632847443,
8.25547253923908));
#28865=CARTESIAN_POINT('Ctrl Pts',(-0.168600607007242,-0.174805494465869,
8.24435875018226));
#28866=CARTESIAN_POINT('Ctrl Pts',(-0.238303522680024,0.0468460954289506,
8.23324496112547));
#28867=CARTESIAN_POINT('Ctrl Pts',(-0.0898845214982184,0.22561892290705,
8.22213117206865));
#28868=CARTESIAN_POINT('Ctrl Pts',(0.14080680157081,0.197880191555585,8.21101738301186));
#28869=CARTESIAN_POINT('Ctrl Pts',(0.242616062304287,-0.0109805232406446,
8.19990359395504));
#28870=CARTESIAN_POINT('Ctrl Pts',(0.122356089757392,-0.209790640587143,
8.18878980489824));
#28871=CARTESIAN_POINT('Ctrl Pts',(-0.109897799356892,-0.21657700541653,
8.17767601584145));
#28872=CARTESIAN_POINT('Ctrl Pts',(-0.241560986393994,-0.0251279810378811,
8.16656222678462));
#28873=CARTESIAN_POINT('Ctrl Pts',(-0.152120663096767,0.189320969355431,
8.15544843772784));
#28874=CARTESIAN_POINT('Ctrl Pts',(0.0765574282985869,0.230482289451893,
8.14433464867103));
#28875=CARTESIAN_POINT('Ctrl Pts',(0.235161637351955,0.0606805561660993,
8.13322085961422));
#28876=CARTESIAN_POINT('Ctrl Pts',(0.178519732822726,-0.164662778342839,
8.12210707055743));
#28877=CARTESIAN_POINT('Ctrl Pts',(-0.0415233077106159,-0.239288404431658,
8.1109932815006));
#28878=CARTESIAN_POINT('Ctrl Pts',(-0.223559593790088,-0.0948906402291072,
8.09987949244382));
#28879=CARTESIAN_POINT('Ctrl Pts',(-0.200969248335269,0.136361603108205,
8.088765703387));
#28880=CARTESIAN_POINT('Ctrl Pts',(0.00557052926712743,0.242800524674804,
8.0776519143302));
#28881=CARTESIAN_POINT('Ctrl Pts',(0.207011538257192,0.127001372461354,
8.06653812527341));
#28882=CARTESIAN_POINT('Ctrl Pts',(0.218972538609993,-0.105043576259552,
8.05542433621658));
#28883=CARTESIAN_POINT('Ctrl Pts',(0.0305054910554562,-0.240940948354804,
8.0443105471598));
#28884=CARTESIAN_POINT('Ctrl Pts',(-0.185883578417697,-0.156302337964917,
8.03319675810297));
#28885=CARTESIAN_POINT('Ctrl Pts',(-0.232131300502452,0.0714015749537549,
8.02208296904619));
#28886=CARTESIAN_POINT('Ctrl Pts',(-0.0659066106883685,0.233750816567481,
8.01096917998937));
#28887=CARTESIAN_POINT('Ctrl Pts',(0.160643147318701,0.182145284864098,
7.99985539093258));
#28888=CARTESIAN_POINT('Ctrl Pts',(0.240154410771491,-0.0361798917467206,
7.98874160187577));
#28889=CARTESIAN_POINT('Ctrl Pts',(0.0998496185014871,-0.221389203127338,
7.97762781281897));
#28890=CARTESIAN_POINT('Ctrl Pts',(-0.13184866193996,-0.203958466174165,
7.96651402376217));
#28891=CARTESIAN_POINT('Ctrl Pts',(-0.242864366871307,0.000157767940311883,
7.95540023470535));
#28892=CARTESIAN_POINT('Ctrl Pts',(-0.131583562478442,0.204129595218713,
7.94428644564855));
#28893=CARTESIAN_POINT('Ctrl Pts',(0.100137168795687,0.221259289107705,
7.93317265659175));
#28894=CARTESIAN_POINT('Ctrl Pts',(0.240201214065173,0.035867846224428,
7.92205886753494));
#28895=CARTESIAN_POINT('Ctrl Pts',(0.160406363583993,-0.182353842678505,
7.91094507847815));
#28896=CARTESIAN_POINT('Ctrl Pts',(-0.0662102497254891,-0.233664992135114,
7.89983128942133));
#28897=CARTESIAN_POINT('Ctrl Pts',(-0.232223872355038,-0.0710999227813469,
7.88871750036453));
#28898=CARTESIAN_POINT('Ctrl Pts',(-0.185680347511564,0.156543709112656,
7.87760371130772));
#28899=CARTESIAN_POINT('Ctrl Pts',(0.0308184982090563,0.240901114896414,
7.86648992225093));
#28900=CARTESIAN_POINT('Ctrl Pts',(0.21910883681408,0.104758985980235,7.85537613319412));
#28901=CARTESIAN_POINT('Ctrl Pts',(0.206846344849442,-0.12727020659438,
7.84426234413731));
#28902=CARTESIAN_POINT('Ctrl Pts',(0.00525510193017616,-0.242807583839013,
7.83314855508051));
#28903=CARTESIAN_POINT('Ctrl Pts',(-0.201146303040926,-0.136100330558978,
7.82203476602371));
#28904=CARTESIAN_POINT('Ctrl Pts',(-0.223436002168958,0.0951809095374688,
7.8109209769669));
#28905=CARTESIAN_POINT('Ctrl Pts',(-0.0412126180342513,0.239342358997698,
7.7998071879101));
#28906=CARTESIAN_POINT('Ctrl Pts',(0.178733982604362,0.164430288641772,
7.7886933988533));
#28907=CARTESIAN_POINT('Ctrl Pts',(0.23508167636479,-0.0609852135282689,
7.77757960979648));
#28908=CARTESIAN_POINT('Ctrl Pts',(0.0762597491160078,-0.230583185734543,
7.76646582073969));
#28909=CARTESIAN_POINT('Ctrl Pts',(-0.152370142836843,-0.189119946824214,
7.75535203168288));
#28910=CARTESIAN_POINT('Ctrl Pts',(-0.2415209216033,0.0254354088453453,
7.74423824262608));
#28911=CARTESIAN_POINT('Ctrl Pts',(-0.109630632113431,0.216732284629596,
7.73312445356927));
#28912=CARTESIAN_POINT('Ctrl Pts',(0.122656937311001,0.209606344739839,
7.72201066451247));
#28913=CARTESIAN_POINT('Ctrl Pts',(0.242573721631839,0.0107152160886697,
7.71089687545566));
#28914=CARTESIAN_POINT('Ctrl Pts',(0.140662758040614,-0.198162384952754,
7.69978308639886));
#28915=CARTESIAN_POINT('Ctrl Pts',(-0.0904173958729584,-0.225299516633279,
7.68866929734205));
#28916=CARTESIAN_POINT('Ctrl Pts',(-0.188575434363685,-0.106431345694509,
7.68126010463752));
#28917=CARTESIAN_POINT('Ctrl Pts',(-0.201667586144655,-0.0393720754290152,
7.67755550828525));
#28918=CARTESIAN_POINT('Ctrl Pts',(-0.0496734897087577,-0.18599788000028,
8.60748149723825));
#28919=CARTESIAN_POINT('Ctrl Pts',(-0.111522209883356,-0.169480262890407,
8.60377690088598));
#28920=CARTESIAN_POINT('Ctrl Pts',(-0.216370986982434,-0.0701402035755114,
8.59636770818144));
#28921=CARTESIAN_POINT('Ctrl Pts',(-0.176257155808688,0.144132145886385,
8.58525391912465));
#28922=CARTESIAN_POINT('Ctrl Pts',(0.025496802598378,0.226064082472793,
8.57414013006782));
#28923=CARTESIAN_POINT('Ctrl Pts',(0.203759132274033,0.101277909923722,
8.56302634101104));
#28924=CARTESIAN_POINT('Ctrl Pts',(0.195595951945087,-0.116309695281798,
8.55191255195423));
#28925=CARTESIAN_POINT('Ctrl Pts',(0.00836249856070296,-0.227387042538631,
8.54079876289741));
#28926=CARTESIAN_POINT('Ctrl Pts',(-0.186505540923786,-0.130359997550735,
8.52968497384063));
#28927=CARTESIAN_POINT('Ctrl Pts',(-0.21067287852326,0.085999912212078,
8.5185711847838));
#28928=CARTESIAN_POINT('Ctrl Pts',(-0.0420039319057314,0.223636632411953,
8.50745739572702));
#28929=CARTESIAN_POINT('Ctrl Pts',(0.165109164160243,0.156579481446523,
8.49634360667019));
#28930=CARTESIAN_POINT('Ctrl Pts',(0.221097243348363,-0.053798295776359,
8.48522981761341));
#28931=CARTESIAN_POINT('Ctrl Pts',(0.0747118661436728,-0.214933050218597,
8.4741160285566));
#28932=CARTESIAN_POINT('Ctrl Pts',(-0.140057805652904,-0.179337566071589,
8.46300223949979));
#28933=CARTESIAN_POINT('Ctrl Pts',(-0.226631142827166,0.0204078377886982,
8.45188845044299));
#28934=CARTESIAN_POINT('Ctrl Pts',(-0.105766342483563,0.201473609556878,
8.44077466138618));
#28935=CARTESIAN_POINT('Ctrl Pts',(0.111907549101888,0.19812835544336,8.42966087232938));
#28936=CARTESIAN_POINT('Ctrl Pts',(0.227151212804134,0.0134339435312874,
8.41854708327257));
#28937=CARTESIAN_POINT('Ctrl Pts',(0.134480784804694,-0.183556695565385,
8.40743329421579));
#28938=CARTESIAN_POINT('Ctrl Pts',(-0.0812814253217577,-0.212535816434684,
8.39631950515895));
#28939=CARTESIAN_POINT('Ctrl Pts',(-0.222645827739863,-0.0469784907230634,
8.38520571610218));
#28940=CARTESIAN_POINT('Ctrl Pts',(-0.160219977699579,0.16157877856595,
8.37409192704536));
#28941=CARTESIAN_POINT('Ctrl Pts',(0.0488570342652188,0.22224116028984,
8.36297813798856));
#28942=CARTESIAN_POINT('Ctrl Pts',(0.213214649034505,0.0794836871683949,
8.35186434893175));
#28943=CARTESIAN_POINT('Ctrl Pts',(0.182414477350531,-0.136026105999789,
8.34075055987495));
#28944=CARTESIAN_POINT('Ctrl Pts',(-0.0153517340858297,-0.227029661818758,
8.32963677081815));
#28945=CARTESIAN_POINT('Ctrl Pts',(-0.199066329257008,-0.110230393426381,
8.31852298176133));
#28946=CARTESIAN_POINT('Ctrl Pts',(-0.200573255671299,0.107464004138028,
8.30740919270455));
#28947=CARTESIAN_POINT('Ctrl Pts',(-0.0184932065254304,0.226795380004735,
8.29629540364772));
#28948=CARTESIAN_POINT('Ctrl Pts',(0.180513884286042,0.138538372511237,
8.28518161459093));
#28949=CARTESIAN_POINT('Ctrl Pts',(0.214294569640967,-0.0765243784701043,
8.27406782553412));
#28950=CARTESIAN_POINT('Ctrl Pts',(0.0519290051392408,-0.221543497994145,
8.26295403647732));
#28951=CARTESIAN_POINT('Ctrl Pts',(-0.157967766682131,-0.163781341329055,
8.25184024742051));
#28952=CARTESIAN_POINT('Ctrl Pts',(-0.223274850182662,0.0438917344607866,
8.24072645836371));
#28953=CARTESIAN_POINT('Ctrl Pts',(-0.0842159312021673,0.211390207932784,
8.22961266930691));
#28954=CARTESIAN_POINT('Ctrl Pts',(0.131926784681382,0.185400826755775,
8.21849888025009));
#28955=CARTESIAN_POINT('Ctrl Pts',(0.227315418394518,-0.0102880337391155,
8.20738509119331));
#28956=CARTESIAN_POINT('Ctrl Pts',(0.114639671718996,-0.196560140278386,
8.19627130213649));
#28957=CARTESIAN_POINT('Ctrl Pts',(-0.102967066583239,-0.20291852127723,
8.18515751307969));
#28958=CARTESIAN_POINT('Ctrl Pts',(-0.226326881115871,-0.0235432784984843,
8.17404372402289));
#28959=CARTESIAN_POINT('Ctrl Pts',(-0.142527134641746,0.177381394088866,
8.16292993496608));
#28960=CARTESIAN_POINT('Ctrl Pts',(0.0717293145376143,0.215946865024847,
8.15181614590928));
#28961=CARTESIAN_POINT('Ctrl Pts',(0.22033110865494,0.0568537213995711,
8.14070235685247));
#28962=CARTESIAN_POINT('Ctrl Pts',(0.167261340295681,-0.154278278187787,
8.12958856779567));
#28963=CARTESIAN_POINT('Ctrl Pts',(-0.038904629708831,-0.224197620115187,
8.11847477873885));
#28964=CARTESIAN_POINT('Ctrl Pts',(-0.209460750932336,-0.0889063377772168,
8.10736098968207));
#28965=CARTESIAN_POINT('Ctrl Pts',(-0.188295071381003,0.127761923794693,
8.09624720062525));
#28966=CARTESIAN_POINT('Ctrl Pts',(0.00521922241672461,0.227488247598545,
8.08513341156845));
#28967=CARTESIAN_POINT('Ctrl Pts',(0.193956302746387,0.118991998483278,
8.07401962251165));
#28968=CARTESIAN_POINT('Ctrl Pts',(0.205162979558262,-0.0984189763048294,
8.06290583345485));
#28969=CARTESIAN_POINT('Ctrl Pts',(0.0285816544739079,-0.225745945933921,
8.05179204439804));
#28970=CARTESIAN_POINT('Ctrl Pts',(-0.174160783088195,-0.146445091116742,
8.04067825534124));
#28971=CARTESIAN_POINT('Ctrl Pts',(-0.217491880772505,0.0668986164002777,
8.02956446628442));
#28972=CARTESIAN_POINT('Ctrl Pts',(-0.0617501934591672,0.219009261643426,
8.01845067722763));
#28973=CARTESIAN_POINT('Ctrl Pts',(0.150512146220409,0.170658245971951,
8.00733688817082));
#28974=CARTESIAN_POINT('Ctrl Pts',(0.225009011544104,-0.0338981976368876,
7.99622309911402));
#28975=CARTESIAN_POINT('Ctrl Pts',(0.0935525768188083,-0.207427236510839,
7.98510931005721));
#28976=CARTESIAN_POINT('Ctrl Pts',(-0.12353359241339,-0.191095773433733,
7.97399552100042));
#28977=CARTESIAN_POINT('Ctrl Pts',(-0.227548063570627,0.000147818264877529,
7.9628817319436));
#28978=CARTESIAN_POINT('Ctrl Pts',(-0.123285211517094,0.191256110181397,
7.95176794288681));
#28979=CARTESIAN_POINT('Ctrl Pts',(0.0938219926802922,0.207305515552022,
7.94065415382999));
#28980=CARTESIAN_POINT('Ctrl Pts',(0.225052863176122,0.0336058313451245,
7.9295403647732));
#28981=CARTESIAN_POINT('Ctrl Pts',(0.150290295312382,-0.170853651034546,
7.91842657571639));
#28982=CARTESIAN_POINT('Ctrl Pts',(-0.0620346834228921,-0.218928849750797,
7.90731278665959));
#28983=CARTESIAN_POINT('Ctrl Pts',(-0.217578614557574,-0.0666159879991351,
7.89619899760278));
#28984=CARTESIAN_POINT('Ctrl Pts',(-0.173970368991043,0.146671240131426,
7.88508520854598));
#28985=CARTESIAN_POINT('Ctrl Pts',(0.0288749217514545,0.225708624582753,
7.87397141948917));
#28986=CARTESIAN_POINT('Ctrl Pts',(0.205290682081311,0.0981523337841342,
7.86285763043236));
#28987=CARTESIAN_POINT('Ctrl Pts',(0.19380152730307,-0.119243878523071,
7.85174384137556));
#28988=CARTESIAN_POINT('Ctrl Pts',(0.00492368758530773,-0.227494861574761,
7.84063005231876));
#28989=CARTESIAN_POINT('Ctrl Pts',(-0.188460960086445,-0.127517128465487,
7.82951626326196));
#28990=CARTESIAN_POINT('Ctrl Pts',(-0.209344953648346,0.08917830117754,
7.81840247420515));
#28991=CARTESIAN_POINT('Ctrl Pts',(-0.0386135337562265,0.224248172022745,
7.80728868514835));
#28992=CARTESIAN_POINT('Ctrl Pts',(0.16746207836014,0.154060450509073,7.79617489609154));
#28993=CARTESIAN_POINT('Ctrl Pts',(0.220256190427845,-0.0571391654674155,
7.78506110703474));
#28994=CARTESIAN_POINT('Ctrl Pts',(0.071450408568683,-0.216041398257672,
7.77394731797793));
#28995=CARTESIAN_POINT('Ctrl Pts',(-0.14276088087832,-0.177193049094902,
7.76283352892113));
#28996=CARTESIAN_POINT('Ctrl Pts',(-0.226289343021431,0.0238313182927837,
7.75171973986433));
#28997=CARTESIAN_POINT('Ctrl Pts',(-0.102716748310195,0.203064007767081,
7.74060595080752));
#28998=CARTESIAN_POINT('Ctrl Pts',(0.114921546244829,0.196387467095744,
7.72949216175072));
#28999=CARTESIAN_POINT('Ctrl Pts',(0.227275747947388,0.0100394582504136,
7.71837837269392));
#29000=CARTESIAN_POINT('Ctrl Pts',(0.131791825293193,-0.185665223554306,
7.70726458363711));
#29001=CARTESIAN_POINT('Ctrl Pts',(-0.0847151997184201,-0.211090945097214,
7.69615079458031));
#29002=CARTESIAN_POINT('Ctrl Pts',(-0.176682876451711,-0.0997192257060688,
7.68874160187577));
#29003=CARTESIAN_POINT('Ctrl Pts',(-0.188949368338152,-0.0368890654402851,
7.6850370055235));
#29004=CARTESIAN_POINT('Ctrl Pts',(-0.0463299576986669,-0.173478327433383,
8.6149629944765));
#29005=CARTESIAN_POINT('Ctrl Pts',(-0.104015628792168,-0.158072514262817,
8.61125839812423));
#29006=CARTESIAN_POINT('Ctrl Pts',(-0.201807014826011,-0.0654190531746837,
8.60384920541969));
#29007=CARTESIAN_POINT('Ctrl Pts',(-0.16439325323391,0.134430583820185,
8.5927354163629));
#29008=CARTESIAN_POINT('Ctrl Pts',(0.0237806079814409,0.210847666221162,
8.58162162730608));
#29009=CARTESIAN_POINT('Ctrl Pts',(0.190044066449164,0.0944608746050748,
8.57050783824928));
#29010=CARTESIAN_POINT('Ctrl Pts',(0.182430351335849,-0.108480867640763,
8.55939404919248));
#29011=CARTESIAN_POINT('Ctrl Pts',(0.00779961719710285,-0.212081577594143,
8.54828026013567));
#29012=CARTESIAN_POINT('Ctrl Pts',(-0.173951817603879,-0.121585441400125,
8.53716647107887));
#29013=CARTESIAN_POINT('Ctrl Pts',(-0.196492447127551,0.080211241816018,
8.52605268202207));
#29014=CARTESIAN_POINT('Ctrl Pts',(-0.0391766392854642,0.208583608284146,
8.51493889296525));
#29015=CARTESIAN_POINT('Ctrl Pts',(0.153995635016914,0.146040086863831,
8.50382510390846));
#29016=CARTESIAN_POINT('Ctrl Pts',(0.20621514597988,-0.0501771222878196,
8.49271131485164));
#29017=CARTESIAN_POINT('Ctrl Pts',(0.0696829962686225,-0.200465865858373,
8.48159752579486));
#29018=CARTESIAN_POINT('Ctrl Pts',(-0.130630488200291,-0.167266320497988,
8.47048373673803));
#29019=CARTESIAN_POINT('Ctrl Pts',(-0.211376557635571,0.0190341823579378,
8.45936994768125));
#29020=CARTESIAN_POINT('Ctrl Pts',(-0.0986471899183328,0.187912382699423,
8.44825615862442));
#29021=CARTESIAN_POINT('Ctrl Pts',(0.104375030754843,0.184792298274526,
8.43714236956764));
#29022=CARTESIAN_POINT('Ctrl Pts',(0.211861621603787,0.0125297022452017,
8.42602858051082));
#29023=CARTESIAN_POINT('Ctrl Pts',(0.125428857682743,-0.171201459585636,
8.41491479145403));
#29024=CARTESIAN_POINT('Ctrl Pts',(-0.0758103571728818,-0.198229990334955,
8.40380100239721));
#29025=CARTESIAN_POINT('Ctrl Pts',(-0.207659494862385,-0.0438163596056552,
8.39268721334042));
#29026=CARTESIAN_POINT('Ctrl Pts',(-0.149435540623878,0.150702880346313,
8.38157342428361));
#29027=CARTESIAN_POINT('Ctrl Pts',(0.0455684580258277,0.207282065655146,
8.3704596352268));
#29028=CARTESIAN_POINT('Ctrl Pts',(0.19886313058378,0.0741336251154622,
8.35934584617));
#29029=CARTESIAN_POINT('Ctrl Pts',(0.170136124295381,-0.126870163015214,
8.34823205711319));
#29030=CARTESIAN_POINT('Ctrl Pts',(-0.0143184059539161,-0.211748252238281,
8.33711826805639));
#29031=CARTESIAN_POINT('Ctrl Pts',(-0.185667136892942,-0.102810764745833,
8.32600447899959));
#29032=CARTESIAN_POINT('Ctrl Pts',(-0.187072631804583,0.10023058164497,
8.31489068994278));
#29033=CARTESIAN_POINT('Ctrl Pts',(-0.0172484252880032,0.211529739977579,
8.30377690088599));
#29034=CARTESIAN_POINT('Ctrl Pts',(0.168363460510403,0.129213328391465,
8.29266311182917));
#29035=CARTESIAN_POINT('Ctrl Pts',(0.199870361529475,-0.0713735080467207,
8.28154932277237));
#29036=CARTESIAN_POINT('Ctrl Pts',(0.0484336539578921,-0.206631363140847,
8.27043553371557));
#29037=CARTESIAN_POINT('Ctrl Pts',(-0.14733492635702,-0.152757188192241,
8.25932174465876));
#29038=CARTESIAN_POINT('Ctrl Pts',(-0.208246177685301,0.0409373734926227,
8.24820795560196));
#29039=CARTESIAN_POINT('Ctrl Pts',(-0.0785473409061163,0.197161492958519,
8.23709416654515));
#29040=CARTESIAN_POINT('Ctrl Pts',(0.123046767791955,0.172921461955964,
8.22598037748835));
#29041=CARTESIAN_POINT('Ctrl Pts',(0.21201477448475,-0.00959554423758641,
8.21486658843154));
#29042=CARTESIAN_POINT('Ctrl Pts',(0.106923253680599,-0.18332963996963,
8.20375279937475));
#29043=CARTESIAN_POINT('Ctrl Pts',(-0.0960363338095857,-0.189260037137931,
8.19263901031793));
#29044=CARTESIAN_POINT('Ctrl Pts',(-0.211092775837749,-0.0219585759590876,
8.18152522126114));
#29045=CARTESIAN_POINT('Ctrl Pts',(-0.132933606186724,0.165441818822301,
8.17041143220433));
#29046=CARTESIAN_POINT('Ctrl Pts',(0.0669012007766416,0.2014114405978,8.15929764314753));
#29047=CARTESIAN_POINT('Ctrl Pts',(0.205500579957926,0.053026886633043,
8.14818385409072));
#29048=CARTESIAN_POINT('Ctrl Pts',(0.156002947768637,-0.143893778032735,
8.13707006503392));
#29049=CARTESIAN_POINT('Ctrl Pts',(-0.0362859517070463,-0.209106835798716,
8.12595627597711));
#29050=CARTESIAN_POINT('Ctrl Pts',(-0.195361908074584,-0.0829220353253264,
8.11484248692031));
#29051=CARTESIAN_POINT('Ctrl Pts',(-0.175620894426736,0.119162244481181,
8.10372869786351));
#29052=CARTESIAN_POINT('Ctrl Pts',(0.00486791556632166,0.212175970522286,
8.09261490880669));
#29053=CARTESIAN_POINT('Ctrl Pts',(0.180901067235581,0.110982624505203,
8.0815011197499));
#29054=CARTESIAN_POINT('Ctrl Pts',(0.19135342050653,-0.0917943763501063,
8.07038733069309));
#29055=CARTESIAN_POINT('Ctrl Pts',(0.0266578178923598,-0.210550943513038,
8.0592735416363));
#29056=CARTESIAN_POINT('Ctrl Pts',(-0.162437987758694,-0.136587844268567,
8.04815975257947));
#29057=CARTESIAN_POINT('Ctrl Pts',(-0.202852461042557,0.0623956578468004,
8.03704596352269));
#29058=CARTESIAN_POINT('Ctrl Pts',(-0.0575937762299663,0.204267706719371,
8.02593217446586));
#29059=CARTESIAN_POINT('Ctrl Pts',(0.140381145122117,0.159171207079804,
8.01481838540908));
#29060=CARTESIAN_POINT('Ctrl Pts',(0.209863612316717,-0.0316165035270548,
8.00370459635226));
#29061=CARTESIAN_POINT('Ctrl Pts',(0.0872555351361295,-0.193465269894341,
7.99259080729547));
#29062=CARTESIAN_POINT('Ctrl Pts',(-0.11521852288682,-0.178233080693301,
7.98147701823866));
#29063=CARTESIAN_POINT('Ctrl Pts',(-0.212231760269946,0.000137868589443255,
7.97036322918185));
#29064=CARTESIAN_POINT('Ctrl Pts',(-0.114986860555745,0.178382625144081,
7.95924944012505));
#29065=CARTESIAN_POINT('Ctrl Pts',(0.0875068165648974,0.193351741996339,
7.94813565106825));
#29066=CARTESIAN_POINT('Ctrl Pts',(0.20990451228707,0.031343816465821,7.93702186201144));
#29067=CARTESIAN_POINT('Ctrl Pts',(0.140174227040771,-0.159353459390588,
7.92590807295464));
#29068=CARTESIAN_POINT('Ctrl Pts',(-0.057859117120295,-0.20419270736648,
7.91479428389783));
#29069=CARTESIAN_POINT('Ctrl Pts',(-0.202933356760109,-0.0621320532169235,
7.90368049484103));
#29070=CARTESIAN_POINT('Ctrl Pts',(-0.162260390470522,0.136798771150197,
7.89256670578423));
#29071=CARTESIAN_POINT('Ctrl Pts',(0.0269313452938532,0.210516134269093,
7.88145291672742));
#29072=CARTESIAN_POINT('Ctrl Pts',(0.191472527348541,0.0915456815880331,
7.87033912767062));
#29073=CARTESIAN_POINT('Ctrl Pts',(0.180756709756699,-0.111217550451763,
7.85922533861381));
#29074=CARTESIAN_POINT('Ctrl Pts',(0.00459227324043899,-0.212182139310508,
7.84811154955701));
#29075=CARTESIAN_POINT('Ctrl Pts',(-0.175775617131964,-0.118933926371996,
7.83699776050021));
#29076=CARTESIAN_POINT('Ctrl Pts',(-0.195253905127734,0.0831756928176114,
7.8258839714434));
#29077=CARTESIAN_POINT('Ctrl Pts',(-0.0360144494782014,0.209153985047792,
7.8147701823866));
#29078=CARTESIAN_POINT('Ctrl Pts',(0.156190174115918,0.143690612376374,
7.80365639332979));
#29079=CARTESIAN_POINT('Ctrl Pts',(0.205430704490901,-0.0532931174065624,
7.79254260427299));
#29080=CARTESIAN_POINT('Ctrl Pts',(0.0666410680213578,-0.2014996107808,
7.78142881521619));
#29081=CARTESIAN_POINT('Ctrl Pts',(-0.133151618919797,-0.165266151365589,
7.77031502615938));
#29082=CARTESIAN_POINT('Ctrl Pts',(-0.211057764439563,0.022227227740222,
7.75920123710257));
#29083=CARTESIAN_POINT('Ctrl Pts',(-0.0958028645069595,0.189395730904567,
7.74808744804577));
#29084=CARTESIAN_POINT('Ctrl Pts',(0.107186155178657,0.183168589451649,
7.73697365898897));
#29085=CARTESIAN_POINT('Ctrl Pts',(0.211977774262937,0.00936370041215743,
7.72585986993216));
#29086=CARTESIAN_POINT('Ctrl Pts',(0.122920892545772,-0.173168062155858,
7.71474608087536));
#29087=CARTESIAN_POINT('Ctrl Pts',(-0.079013003563882,-0.196882373561149,
7.70363229181855));
#29088=CARTESIAN_POINT('Ctrl Pts',(-0.164790318539738,-0.0930071057176291,
7.69622309911402));
#29089=CARTESIAN_POINT('Ctrl Pts',(-0.17623115053165,-0.034406055451555,
7.69251850276175));
#29090=CARTESIAN_POINT('Ctrl Pts',(-0.042986425688576,-0.160958774866487,
8.62244449171475));
#29091=CARTESIAN_POINT('Ctrl Pts',(-0.0965090477009803,-0.146664765635227,
8.61873989536248));
#29092=CARTESIAN_POINT('Ctrl Pts',(-0.187243042669588,-0.0606979027738561,
8.61133070265794));
#29093=CARTESIAN_POINT('Ctrl Pts',(-0.152529350659133,0.124729021753987,
8.60021691360114));
#29094=CARTESIAN_POINT('Ctrl Pts',(0.022064413364504,0.19563124996953,8.58910312454432));
#29095=CARTESIAN_POINT('Ctrl Pts',(0.176329000624295,0.0876438392864277,
8.57798933548754));
#29096=CARTESIAN_POINT('Ctrl Pts',(0.169264750726611,-0.100652039999728,
8.56687554643072));
#29097=CARTESIAN_POINT('Ctrl Pts',(0.00723673583350253,-0.196776112649654,
8.55576175737392));
#29098=CARTESIAN_POINT('Ctrl Pts',(-0.161398094283972,-0.112810885249515,
8.54464796831711));
#29099=CARTESIAN_POINT('Ctrl Pts',(-0.182312015731842,0.0744225714199578,
8.53353417926031));
#29100=CARTESIAN_POINT('Ctrl Pts',(-0.0363493466651971,0.19353058415634,
8.52242039020351));
#29101=CARTESIAN_POINT('Ctrl Pts',(0.142882105873586,0.13550069228114,8.51130660114671));
#29102=CARTESIAN_POINT('Ctrl Pts',(0.191333048611396,-0.0465559487992802,
8.50019281208989));
#29103=CARTESIAN_POINT('Ctrl Pts',(0.0646541263935723,-0.185998681498147,
8.4890790230331));
#29104=CARTESIAN_POINT('Ctrl Pts',(-0.121203170747678,-0.155195074924388,
8.47796523397628));
#29105=CARTESIAN_POINT('Ctrl Pts',(-0.196121972443975,0.0176605269271775,
8.46685144491949));
#29106=CARTESIAN_POINT('Ctrl Pts',(-0.0915280373531031,0.174351155841967,
8.45573765586269));
#29107=CARTESIAN_POINT('Ctrl Pts',(0.0968425124077976,0.171456241105691,
8.44462386680587));
#29108=CARTESIAN_POINT('Ctrl Pts',(0.196572030403439,0.0116254609591159,
8.43351007774908));
#29109=CARTESIAN_POINT('Ctrl Pts',(0.116376930560793,-0.158846223605886,
8.42239628869226));
#29110=CARTESIAN_POINT('Ctrl Pts',(-0.0703392890240059,-0.183924164235226,
8.41128249963547));
#29111=CARTESIAN_POINT('Ctrl Pts',(-0.192673161984908,-0.040654228488247,
8.40016871057866));
#29112=CARTESIAN_POINT('Ctrl Pts',(-0.138651103548177,0.139826982126676,
8.38905492152185));
#29113=CARTESIAN_POINT('Ctrl Pts',(0.0422798817864365,0.192322971020452,
8.37794113246506));
#29114=CARTESIAN_POINT('Ctrl Pts',(0.184511612133054,0.0687835630625294,
8.36682734340824));
#29115=CARTESIAN_POINT('Ctrl Pts',(0.157857771240231,-0.117714220030638,
8.35571355435146));
#29116=CARTESIAN_POINT('Ctrl Pts',(-0.0132850778220027,-0.196466842657805,
8.34459976529463));
#29117=CARTESIAN_POINT('Ctrl Pts',(-0.172267944528876,-0.0953911360652848,
8.33348597623784));
#29118=CARTESIAN_POINT('Ctrl Pts',(-0.173572007937867,0.092997159151912,
8.32237218718103));
#29119=CARTESIAN_POINT('Ctrl Pts',(-0.016003644050576,0.196264099950422,
8.31125839812423));
#29120=CARTESIAN_POINT('Ctrl Pts',(0.156213036734765,0.119888284271693,
8.30014460906742));
#29121=CARTESIAN_POINT('Ctrl Pts',(0.185446153417982,-0.066222637623337,
8.28903082001062));
#29122=CARTESIAN_POINT('Ctrl Pts',(0.0449383027765433,-0.191719228287548,
8.27791703095383));
#29123=CARTESIAN_POINT('Ctrl Pts',(-0.136702086031909,-0.141733035055427,
8.266803241897));
#29124=CARTESIAN_POINT('Ctrl Pts',(-0.19321750518794,0.0379830125244588,
8.25568945284021));
#29125=CARTESIAN_POINT('Ctrl Pts',(-0.0728787506100653,0.182932777984253,
8.2445756637834));
#29126=CARTESIAN_POINT('Ctrl Pts',(0.114166750902528,0.160442097156153,
8.23346187472661));
#29127=CARTESIAN_POINT('Ctrl Pts',(0.196714130574981,-0.0089030547360575,
8.22234808566979));
#29128=CARTESIAN_POINT('Ctrl Pts',(0.0992068356422025,-0.170099139660873,
8.21123429661299));
#29129=CARTESIAN_POINT('Ctrl Pts',(-0.0891056010359326,-0.175601552998632,
8.20012050755619));
#29130=CARTESIAN_POINT('Ctrl Pts',(-0.195858670559627,-0.0203738734196908,
8.18900671849937));
#29131=CARTESIAN_POINT('Ctrl Pts',(-0.123340077731702,0.153502243555736,
8.17789292944259));
#29132=CARTESIAN_POINT('Ctrl Pts',(0.062073087015669,0.186876016170753,
8.16677914038577));
#29133=CARTESIAN_POINT('Ctrl Pts',(0.190670051260911,0.0492000518665148,
8.15566535132897));
#29134=CARTESIAN_POINT('Ctrl Pts',(0.144744555241592,-0.133509277877683,
8.14455156227217));
#29135=CARTESIAN_POINT('Ctrl Pts',(-0.0336672737052616,-0.194016051482245,
8.13343777321535));
#29136=CARTESIAN_POINT('Ctrl Pts',(-0.181263065216832,-0.076937732873436,
8.12232398415856));
#29137=CARTESIAN_POINT('Ctrl Pts',(-0.16294671747247,0.11056256516767,8.11121019510174));
#29138=CARTESIAN_POINT('Ctrl Pts',(0.00451660871591894,0.196863693446027,
8.10009640604495));
#29139=CARTESIAN_POINT('Ctrl Pts',(0.167845831724775,0.102973250527127,
8.08898261698814));
#29140=CARTESIAN_POINT('Ctrl Pts',(0.177543861454799,-0.0851697763953834,
8.07786882793134));
#29141=CARTESIAN_POINT('Ctrl Pts',(0.0247339813108116,-0.195355941092154,
8.06675503887455));
#29142=CARTESIAN_POINT('Ctrl Pts',(-0.150715192429192,-0.126730597420393,
8.05564124981772));
#29143=CARTESIAN_POINT('Ctrl Pts',(-0.18821304131261,0.0578926992933231,
8.04452746076093));
#29144=CARTESIAN_POINT('Ctrl Pts',(-0.0534373590007651,0.189526151795315,
8.03341367170412));
#29145=CARTESIAN_POINT('Ctrl Pts',(0.130250144023825,0.147684168187657,
8.02229988264732));
#29146=CARTESIAN_POINT('Ctrl Pts',(0.194718213089331,-0.0293348094172218,
8.01118609359052));
#29147=CARTESIAN_POINT('Ctrl Pts',(0.0809584934534505,-0.179503303277842,
8.00007230453371));
#29148=CARTESIAN_POINT('Ctrl Pts',(-0.10690345336025,-0.165370387952869,
7.98895851547691));
#29149=CARTESIAN_POINT('Ctrl Pts',(-0.196915456969266,0.000127918914008822,
7.9778447264201));
#29150=CARTESIAN_POINT('Ctrl Pts',(-0.106688509594396,0.165509140106765,
7.9667309373633));
#29151=CARTESIAN_POINT('Ctrl Pts',(0.0811916404495023,0.179397968440655,
7.95561714830649));
#29152=CARTESIAN_POINT('Ctrl Pts',(0.194756161398019,0.0290818015865176,
7.94450335924969));
#29153=CARTESIAN_POINT('Ctrl Pts',(0.13005815876916,-0.14785326774663,7.93338957019289));
#29154=CARTESIAN_POINT('Ctrl Pts',(-0.0536835508176979,-0.189456564982163,
7.92227578113608));
#29155=CARTESIAN_POINT('Ctrl Pts',(-0.188288098962645,-0.0576481184347118,
7.91116199207928));
#29156=CARTESIAN_POINT('Ctrl Pts',(-0.150550411950001,0.126926302168967,
7.90004820302248));
#29157=CARTESIAN_POINT('Ctrl Pts',(0.0249877688362514,0.195323643955433,
7.88893441396566));
#29158=CARTESIAN_POINT('Ctrl Pts',(0.177654372615772,0.0849390293919319,
7.87782062490887));
#29159=CARTESIAN_POINT('Ctrl Pts',(0.167711892210327,-0.103191222380454,
7.86670683585206));
#29160=CARTESIAN_POINT('Ctrl Pts',(0.00426085889557056,-0.196869417046256,
7.85559304679526));
#29161=CARTESIAN_POINT('Ctrl Pts',(-0.163090274177483,-0.110350724278505,
7.84447925773845));
#29162=CARTESIAN_POINT('Ctrl Pts',(-0.181162856607122,0.0771730844576825,
7.83336546868165));
#29163=CARTESIAN_POINT('Ctrl Pts',(-0.0334153652001765,0.194059798072839,
7.82225167962485));
#29164=CARTESIAN_POINT('Ctrl Pts',(0.144918269871696,0.133320774243675,
7.81113789056804));
#29165=CARTESIAN_POINT('Ctrl Pts',(0.190605218553956,-0.0494470693457091,
7.80002410151123));
#29166=CARTESIAN_POINT('Ctrl Pts',(0.0618317274740329,-0.186957823303929,
7.78891031245443));
#29167=CARTESIAN_POINT('Ctrl Pts',(-0.123542356961275,-0.153339253636277,
7.77779652339763));
#29168=CARTESIAN_POINT('Ctrl Pts',(-0.195826185857694,0.0206231371876604,
7.76668273434082));
#29169=CARTESIAN_POINT('Ctrl Pts',(-0.0888889807037237,0.175727454042052,
7.75556894528402));
#29170=CARTESIAN_POINT('Ctrl Pts',(0.0994507641124849,0.169949711807554,
7.74445515622721));
#29171=CARTESIAN_POINT('Ctrl Pts',(0.196679800578486,0.00868794257390136,
7.73334136717042));
#29172=CARTESIAN_POINT('Ctrl Pts',(0.114049959798351,-0.16067090075741,
7.72222757811361));
#29173=CARTESIAN_POINT('Ctrl Pts',(-0.0733108074093436,-0.182673802025085,
7.7111137890568));
#29174=CARTESIAN_POINT('Ctrl Pts',(-0.152897760627765,-0.0862949857291892,
7.70370459635227));
#29175=CARTESIAN_POINT('Ctrl Pts',(-0.163512932725147,-0.0319230454628249,
7.7));
#29176=CARTESIAN_POINT('Ctrl Pts',(-0.166383640089184,9.41837290711752E-5,
8.53785196366098));
#29177=CARTESIAN_POINT('Ctrl Pts',(-0.166495359952371,0.0216826172703768,
8.53641270219409));
#29178=CARTESIAN_POINT('Ctrl Pts',(-0.162596302111187,0.0432323652637361,
8.5349734407272));
#29179=CARTESIAN_POINT('Ctrl Pts',(-0.15449925064609,0.0630683307644428,
8.53353417926031));
#29180=CARTESIAN_POINT('Ctrl Pts',(-0.133657792709627,0.114125242332085,
8.52982958290805));
#29181=CARTESIAN_POINT('Ctrl Pts',(-0.0850035696874118,0.153827913244213,
8.52612498655578));
#29182=CARTESIAN_POINT('Ctrl Pts',(-0.0308045494198404,0.164007600054409,
8.52242039020351));
#29183=CARTESIAN_POINT('Ctrl Pts',(0.0233944708477309,0.174187286864606,
8.51871579385124));
#29184=CARTESIAN_POINT('Ctrl Pts',(0.0831382883606584,0.154843989572873,
8.51501119749897));
#29185=CARTESIAN_POINT('Ctrl Pts',(0.121085354240091,0.114829567413603,
8.51130660114671));
#29186=CARTESIAN_POINT('Ctrl Pts',(0.159032420119523,0.0748151452543328,
8.50760200479444));
#29187=CARTESIAN_POINT('Ctrl Pts',(0.17518273436546,0.0141295982275263,
8.50389740844216));
#29188=CARTESIAN_POINT('Ctrl Pts',(0.162144737785457,-0.0394536307356881,
8.5001928120899));
#29189=CARTESIAN_POINT('Ctrl Pts',(0.149106741205455,-0.0930368596989026,
8.49648821573763));
#29190=CARTESIAN_POINT('Ctrl Pts',(0.106880433799514,-0.139517770598525,
8.49278361938537));
#29191=CARTESIAN_POINT('Ctrl Pts',(0.0547910639063346,-0.157624291619376,
8.4890790230331));
#29192=CARTESIAN_POINT('Ctrl Pts',(0.00270169401315546,-0.175730812640227,
8.48537442668083));
#29193=CARTESIAN_POINT('Ctrl Pts',(-0.0592507383672613,-0.165462943782308,
8.48166983032856));
#29194=CARTESIAN_POINT('Ctrl Pts',(-0.102713421506852,-0.131519742378087,
8.47796523397629));
#29195=CARTESIAN_POINT('Ctrl Pts',(-0.142263377059629,-0.100632277318825,
8.47459414387118));
#29196=CARTESIAN_POINT('Ctrl Pts',(-0.166502812179775,-0.0501403461319692,
8.47122305376608));
#29197=CARTESIAN_POINT('Ctrl Pts',(-0.16681984310415,8.64016909114964E-5,
8.46785196366098));
#29198=CARTESIAN_POINT('Ctrl Pts',(-0.0530170217188485,-0.198517432567176,
8.6));
#29199=CARTESIAN_POINT('Ctrl Pts',(-0.06542081092342,-0.193924769288753,
8.6));
#29200=CARTESIAN_POINT('Ctrl Pts',(-0.0772704541431171,-0.188065565737325,
8.6));
#29201=CARTESIAN_POINT('Ctrl Pts',(-0.0884481740526511,-0.181102974015431,
8.6));
#29202=CARTESIAN_POINT('Ctrl Pts',(-0.0941164108607929,-0.1775722343836,
8.6));
#29203=CARTESIAN_POINT('Ctrl Pts',(-0.0996114240419522,-0.173757009103972,
8.6));
#29204=CARTESIAN_POINT('Ctrl Pts',(-0.104914415136506,-0.169674993381027,
8.6));
#29205=CARTESIAN_POINT('Ctrl Pts',(-0.109523380425031,-0.166127209038415,
8.6));
#29206=CARTESIAN_POINT('Ctrl Pts',(-0.113987272284976,-0.162377843722833,
8.6));
#29207=CARTESIAN_POINT('Ctrl Pts',(-0.118291910700038,-0.158437614516047,
8.6));
#29208=CARTESIAN_POINT('Ctrl Pts',(-0.121383799927864,-0.155607469201867,
8.6));
#29209=CARTESIAN_POINT('Ctrl Pts',(-0.124387199055957,-0.15268442084067,
8.6));
#29210=CARTESIAN_POINT('Ctrl Pts',(-0.127293146906171,-0.14967825940901,
8.6));
#29211=CARTESIAN_POINT('Ctrl Pts',(-0.136236980136076,-0.140425992027493,
8.6));
#29212=CARTESIAN_POINT('Ctrl Pts',(-0.144276520214277,-0.130374017836739,
8.6));
#29213=CARTESIAN_POINT('Ctrl Pts',(-0.151272696882763,-0.119653258631744,
8.6));
#29214=CARTESIAN_POINT('Ctrl Pts',(-0.155802688817768,-0.112711616784059,
8.6));
#29215=CARTESIAN_POINT('Ctrl Pts',(-0.159894413372832,-0.10548900882637,
8.6));
#29216=CARTESIAN_POINT('Ctrl Pts',(-0.163498383914012,-0.0980183248117674,
8.6));
#29217=CARTESIAN_POINT('Ctrl Pts',(-0.165162652591317,-0.0945684560457829,
8.6));
#29218=CARTESIAN_POINT('Ctrl Pts',(-0.166718761668699,-0.0910738139207644,
8.6));
#29219=CARTESIAN_POINT('Ctrl Pts',(-0.168161639193221,-0.0875412396582513,
8.6));
#29220=CARTESIAN_POINT('Ctrl Pts',(-0.172163015187704,-0.0777447339864133,
8.6));
#29221=CARTESIAN_POINT('Ctrl Pts',(-0.175299623694641,-0.0676487151368408,
8.6));
#29222=CARTESIAN_POINT('Ctrl Pts',(-0.177477376050015,-0.057326480317048,
8.6));
#29223=CARTESIAN_POINT('Ctrl Pts',(-0.179331110212822,-0.0485400454064169,
8.6));
#29224=CARTESIAN_POINT('Ctrl Pts',(-0.18048935110848,-0.0395892198362765,
8.6));
#29225=CARTESIAN_POINT('Ctrl Pts',(-0.180964733448231,-0.0305523301186972,
8.6));
#29226=CARTESIAN_POINT('Ctrl Pts',(-0.181133859445773,-0.0273372906433986,
8.6));
#29227=CARTESIAN_POINT('Ctrl Pts',(-0.181216193772417,-0.0241127956726884,
8.6));
#29228=CARTESIAN_POINT('Ctrl Pts',(-0.181212666773714,-0.0208920829129295,
8.6));
#29229=CARTESIAN_POINT('Ctrl Pts',(-0.18119984414273,-0.00918297420461843,
8.6));
#29230=CARTESIAN_POINT('Ctrl Pts',(-0.180057695209983,0.00251249492629139,
8.6));
#29231=CARTESIAN_POINT('Ctrl Pts',(-0.177831621291215,0.0140219353702633,
8.6));
#29232=CARTESIAN_POINT('Ctrl Pts',(-0.176688035248831,0.0199346031107226,
8.6));
#29233=CARTESIAN_POINT('Ctrl Pts',(-0.17525769513229,0.0257979924523235,
8.6));
#29234=CARTESIAN_POINT('Ctrl Pts',(-0.173542822423344,0.0315864625403328,
8.6));
#29235=CARTESIAN_POINT('Ctrl Pts',(-0.171856156212592,0.0372797229546229,
8.6));
#29236=CARTESIAN_POINT('Ctrl Pts',(-0.169891488737815,0.0429059368612729,
8.6));
#29237=CARTESIAN_POINT('Ctrl Pts',(-0.167662780533083,0.048407845623496,
8.6));
#29238=CARTESIAN_POINT('Ctrl Pts',(-0.164206394717703,0.0569404652651757,
8.6));
#29239=CARTESIAN_POINT('Ctrl Pts',(-0.160113292534287,0.0651877483840102,
8.6));
#29240=CARTESIAN_POINT('Ctrl Pts',(-0.155392822172953,0.0730538252569167,
8.6));
#29241=CARTESIAN_POINT('Ctrl Pts',(-0.152978226140765,0.0770774492927307,
8.6));
#29242=CARTESIAN_POINT('Ctrl Pts',(-0.150398552838242,0.0810014273591959,
8.6));
#29243=CARTESIAN_POINT('Ctrl Pts',(-0.147663850341513,0.0847992235167022,
8.6));
#29244=CARTESIAN_POINT('Ctrl Pts',(-0.142229060792935,0.0923467439102818,
8.6));
#29245=CARTESIAN_POINT('Ctrl Pts',(-0.136175359211409,0.0994106650199937,
8.6));
#29246=CARTESIAN_POINT('Ctrl Pts',(-0.129507404772142,0.105879808304267,
8.6));
#29247=CARTESIAN_POINT('Ctrl Pts',(-0.128728930874604,0.106635071291155,
8.6));
#29248=CARTESIAN_POINT('Ctrl Pts',(-0.127942070273424,0.107382201802382,
8.6));
#29249=CARTESIAN_POINT('Ctrl Pts',(-0.127146980098767,0.108121134152663,
8.6));
#29250=CARTESIAN_POINT('Origin',(0.,0.,8.1));
#29251=CARTESIAN_POINT('Origin',(0.,0.,7.6));
#29252=CARTESIAN_POINT('Origin',(0.,0.,7.1));
#29253=CARTESIAN_POINT('',(-0.6,-7.34788079488412E-17,7.36457513110646));
#29254=CARTESIAN_POINT('Origin',(0.,0.,7.36457513110646));
#29255=CARTESIAN_POINT('',(-0.6,-7.34788079488412E-17,6.83542486889354));
#29256=CARTESIAN_POINT('Origin',(-0.899999999999998,-1.10218211923262E-16,
7.1));
#29257=CARTESIAN_POINT('Origin',(0.,0.,6.83542486889354));
#29258=CARTESIAN_POINT('Origin',(0.,0.,2.4));
#29259=CARTESIAN_POINT('',(-0.6,-7.34788079488412E-17,6.56457513110646));
#29260=CARTESIAN_POINT('',(-0.6,-7.34788079488412E-17,2.4));
#29261=CARTESIAN_POINT('Origin',(0.,0.,6.56457513110646));
#29262=CARTESIAN_POINT('Origin',(0.,0.,6.3));
#29263=CARTESIAN_POINT('',(-0.6,-7.34788079488412E-17,6.03542486889354));
#29264=CARTESIAN_POINT('Origin',(-0.900000000000001,-1.10218211923262E-16,
6.3));
#29265=CARTESIAN_POINT('Origin',(0.,0.,6.03542486889354));
#29266=CARTESIAN_POINT('Origin',(0.,0.,2.4));
#29267=CARTESIAN_POINT('',(-0.6,-7.34788079488412E-17,2.4));
#29268=CARTESIAN_POINT('',(-0.6,-7.34788079488412E-17,2.4));
#29269=CARTESIAN_POINT('Origin',(0.,0.,2.4));
#29270=CARTESIAN_POINT('Origin',(0.,0.,7.8));
#29271=CARTESIAN_POINT('',(-1.,-1.22464679914735E-16,7.8));
#29272=CARTESIAN_POINT('Origin',(0.,0.,7.8));
#29273=CARTESIAN_POINT('',(-0.6,-7.34788079488412E-17,7.8));
#29274=CARTESIAN_POINT('Origin',(0.,0.,7.8));
#29275=CARTESIAN_POINT('Origin',(0.,0.,7.6));
#29276=CARTESIAN_POINT('',(-1.,-1.22464679914735E-16,7.6));
#29277=CARTESIAN_POINT('Origin',(0.,0.,7.6));
#29278=CARTESIAN_POINT('',(-0.6,7.34788079488412E-17,7.6));
#29279=CARTESIAN_POINT('Origin',(0.,0.,7.6));
#29280=CARTESIAN_POINT('Origin',(0.,0.,7.6));
#29281=CARTESIAN_POINT('',(-1.,-1.22464679914735E-16,7.6));
#29282=CARTESIAN_POINT('Origin',(0.,0.,2.4));
#29283=CARTESIAN_POINT('',(-0.6,-7.34788079488412E-17,2.4));
#29284=CARTESIAN_POINT('Origin',(-1.8,0.6,2.));
#29285=CARTESIAN_POINT('',(0.8,0.6,2.4));
#29286=CARTESIAN_POINT('',(0.8,0.6,2.));
#29287=CARTESIAN_POINT('',(1.8,0.6,2.4));
#29288=CARTESIAN_POINT('',(1.8,0.6,2.));
#29289=CARTESIAN_POINT('',(-1.8,0.6,2.4));
#29290=CARTESIAN_POINT('Origin',(1.8,1.4,2.));
#29291=CARTESIAN_POINT('',(-1.8,1.4,2.4));
#29292=CARTESIAN_POINT('',(-1.8,1.4,2.));
#29293=CARTESIAN_POINT('',(1.8,1.4,2.4));
#29294=CARTESIAN_POINT('',(1.8,1.4,2.4));
#29295=CARTESIAN_POINT('',(1.8,1.4,2.));
#29296=CARTESIAN_POINT('Origin',(1.8,0.6,2.));
#29297=CARTESIAN_POINT('',(1.8,0.6,2.4));
#29298=CARTESIAN_POINT('Origin',(-1.8,0.6,2.));
#29299=CARTESIAN_POINT('',(-0.8,0.6,2.4));
#29300=CARTESIAN_POINT('',(-0.8,0.6,2.));
#29301=CARTESIAN_POINT('',(-1.8,0.6,2.4));
#29302=CARTESIAN_POINT('',(-1.8,0.6,2.4));
#29303=CARTESIAN_POINT('',(-1.8,0.6,2.));
#29304=CARTESIAN_POINT('Origin',(-1.8,1.4,2.));
#29305=CARTESIAN_POINT('',(-1.8,1.4,2.4));
#29306=CARTESIAN_POINT('Origin',(0.,0.,2.));
#29307=CARTESIAN_POINT('Origin',(0.,0.,2.4));
#29308=CARTESIAN_POINT('Origin',(0.,0.,2.4));
#29309=CARTESIAN_POINT('',(-0.6,-7.34788079488412E-17,8.6));
#29310=CARTESIAN_POINT('Origin',(0.,0.,8.6));
#29311=CARTESIAN_POINT('',(-0.6,-7.34788079488412E-17,2.4));
#29312=CARTESIAN_POINT('Origin',(0.,0.,8.6));
#29313=CARTESIAN_POINT('Origin',(0.,0.,2.4));
#29314=CARTESIAN_POINT('',(0.,0.,0.));
#29315=CARTESIAN_POINT('Origin',(0.,0.,9.2));
#29316=CARTESIAN_POINT('',(-2.,2.44929359829471E-16,9.4));
#29317=CARTESIAN_POINT('Origin',(0.,0.,9.4));
#29318=CARTESIAN_POINT('',(-2.2,-2.69422295812418E-16,9.2));
#29319=CARTESIAN_POINT('Origin',(-2.,-2.44929359829471E-16,9.2));
#29320=CARTESIAN_POINT('Origin',(0.,0.,9.2));
#29321=CARTESIAN_POINT('Origin',(0.,0.,8.6));
#29322=CARTESIAN_POINT('',(-2.2,2.69422295812418E-16,8.8));
#29323=CARTESIAN_POINT('',(-2.2,-2.69422295812418E-16,8.6));
#29324=CARTESIAN_POINT('Origin',(0.,0.,8.8));
#29325=CARTESIAN_POINT('Origin',(0.,0.,9.4));
#29326=CARTESIAN_POINT('',(-0.4,4.89858719658941E-17,9.4));
#29327=CARTESIAN_POINT('Origin',(0.,0.,9.4));
#29328=CARTESIAN_POINT('Origin',(0.,0.,8.8));
#29329=CARTESIAN_POINT('',(-2.,-2.44929359829471E-16,8.6));
#29330=CARTESIAN_POINT('Origin',(-2.,-2.44929359829471E-16,8.8));
#29331=CARTESIAN_POINT('Origin',(0.,0.,8.6));
#29332=CARTESIAN_POINT('Origin',(0.,0.,8.6));
#29333=CARTESIAN_POINT('',(-1.,-1.22464679914735E-16,8.6));
#29334=CARTESIAN_POINT('Origin',(0.,0.,8.6));
#29335=CARTESIAN_POINT('Origin',(0.,0.,9.));
#29336=CARTESIAN_POINT('',(-0.4,4.89858719658941E-17,9.));
#29337=CARTESIAN_POINT('Origin',(0.,0.,9.));
#29338=CARTESIAN_POINT('',(-0.25,3.06161699786838E-17,9.));
#29339=CARTESIAN_POINT('Origin',(0.,0.,9.));
#29340=CARTESIAN_POINT('Origin',(0.,0.,9.2));
#29341=CARTESIAN_POINT('',(-0.4,4.89858719658941E-17,9.2));
#29342=CARTESIAN_POINT('Origin',(0.,0.,8.6));
#29343=CARTESIAN_POINT('',(-0.6,-7.34788079488412E-17,8.6));
#29344=CARTESIAN_POINT('Origin',(0.,0.,8.6));
#29345=CARTESIAN_POINT('',(-0.25,-3.06161699786838E-17,8.6));
#29346=CARTESIAN_POINT('Origin',(0.,0.,8.6));
#29347=CARTESIAN_POINT('Origin',(0.,0.,8.6));
#29348=CARTESIAN_POINT('',(-0.25,-3.06161699786838E-17,8.6));
#29349=CARTESIAN_POINT('Origin',(0.,0.,7.8));
#29350=CARTESIAN_POINT('',(-0.6,-7.34788079488412E-17,7.8));
#29351=CARTESIAN_POINT('',(-0.6,-7.34788079488412E-17,7.8));
#29352=CARTESIAN_POINT('Origin',(0.,0.,7.8));
#29353=CARTESIAN_POINT('Origin',(0.,0.,7.8));
#29354=CARTESIAN_POINT('',(-1.,-1.22464679914735E-16,7.8));
#29355=CARTESIAN_POINT('',(-1.,-1.22464679914735E-16,7.8));
#29356=CARTESIAN_POINT('Origin',(0.,0.,7.8));
#29357=CARTESIAN_POINT('Origin',(0.,0.,7.8));
#29358=CARTESIAN_POINT('',(0.,0.,0.));
#29359=CARTESIAN_POINT('Origin',(-0.6,1.,2.5));
#29360=CARTESIAN_POINT('',(-0.8,1.,2.6));
#29361=CARTESIAN_POINT('Origin',(-0.6,1.,2.6));
#29362=CARTESIAN_POINT('',(-0.8,1.,2.4));
#29363=CARTESIAN_POINT('',(-0.8,1.,2.5));
#29364=CARTESIAN_POINT('Origin',(-0.6,1.,2.4));
#29365=CARTESIAN_POINT('Origin',(0.6,1.,2.5));
#29366=CARTESIAN_POINT('',(0.4,1.,2.6));
#29367=CARTESIAN_POINT('Origin',(0.6,1.,2.6));
#29368=CARTESIAN_POINT('',(0.4,1.,2.4));
#29369=CARTESIAN_POINT('',(0.4,1.,2.5));
#29370=CARTESIAN_POINT('Origin',(0.6,1.,2.4));
#29371=CARTESIAN_POINT('Origin',(1.8,1.4,2.4));
#29372=CARTESIAN_POINT('',(1.8,1.4,2.4));
#29373=CARTESIAN_POINT('',(-1.8,1.4,2.4));
#29374=CARTESIAN_POINT('',(1.8,1.4,2.4));
#29375=CARTESIAN_POINT('',(-1.8,1.4,2.6));
#29376=CARTESIAN_POINT('',(-1.8,1.4,2.4));
#29377=CARTESIAN_POINT('',(1.8,1.4,2.6));
#29378=CARTESIAN_POINT('',(1.8,1.4,2.6));
#29379=CARTESIAN_POINT('',(1.8,1.4,2.4));
#29380=CARTESIAN_POINT('Origin',(1.8,0.6,2.4));
#29381=CARTESIAN_POINT('',(1.8,0.6,2.4));
#29382=CARTESIAN_POINT('',(1.8,0.6,2.4));
#29383=CARTESIAN_POINT('',(1.8,0.6,2.6));
#29384=CARTESIAN_POINT('',(1.8,0.6,2.6));
#29385=CARTESIAN_POINT('',(1.8,0.6,2.4));
#29386=CARTESIAN_POINT('Origin',(-1.8,0.6,2.4));
#29387=CARTESIAN_POINT('',(-1.8,0.6,2.4));
#29388=CARTESIAN_POINT('',(-1.8,0.6,2.4));
#29389=CARTESIAN_POINT('',(-1.8,0.6,2.6));
#29390=CARTESIAN_POINT('',(-1.8,0.6,2.6));
#29391=CARTESIAN_POINT('',(-1.8,0.6,2.4));
#29392=CARTESIAN_POINT('Origin',(-1.8,1.4,2.4));
#29393=CARTESIAN_POINT('',(-1.8,1.4,2.4));
#29394=CARTESIAN_POINT('',(-1.8,1.4,2.6));
#29395=CARTESIAN_POINT('Origin',(0.,1.,2.6));
#29396=CARTESIAN_POINT('Origin',(0.,1.,2.4));
#29397=CARTESIAN_POINT('',(0.,0.,0.));
#29398=CARTESIAN_POINT('Ctrl Pts',(0.55,-6.12323399573676E-18,0.));
#29399=CARTESIAN_POINT('Ctrl Pts',(0.55,0.00964912280701754,-0.0909408399723361));
#29400=CARTESIAN_POINT('Ctrl Pts',(0.504021197632585,0.0289473684210526,
-0.272733075266705));
#29401=CARTESIAN_POINT('Ctrl Pts',(0.313429112214632,0.0578947368421053,
-0.4797633508545));
#29402=CARTESIAN_POINT('Ctrl Pts',(0.0473287281417178,0.0868421052631579,
-0.571108104224167));
#29403=CARTESIAN_POINT('Ctrl Pts',(-0.230201927212741,0.115789473684211,
-0.52480399893423));
#29404=CARTESIAN_POINT('Ctrl Pts',(-0.452231273974558,0.144736842105263,
-0.351985646771294));
#29405=CARTESIAN_POINT('Ctrl Pts',(-0.565254339124195,0.173684210526316,
-0.0943246722345097));
#29406=CARTESIAN_POINT('Ctrl Pts',(-0.542018875701069,0.202631578947368,
0.186075664943732));
#29407=CARTESIAN_POINT('Ctrl Pts',(-0.388129668188505,0.231578947368421,
0.421620932468086));
#29408=CARTESIAN_POINT('Ctrl Pts',(-0.140680214568305,0.260526315789474,
0.555533945989301));
#29409=CARTESIAN_POINT('Ctrl Pts',(0.140680250766997,0.289473684210526,
0.555533855939788));
#29410=CARTESIAN_POINT('Ctrl Pts',(0.388129540647023,0.318421052631579,
0.421621069647034));
#29411=CARTESIAN_POINT('Ctrl Pts',(0.542019161337126,0.347368421052632,
0.186075408839635));
#29412=CARTESIAN_POINT('Ctrl Pts',(0.565253745898005,0.376315789473684,
-0.0943241631669167));
#29413=CARTESIAN_POINT('Ctrl Pts',(0.452232485289668,0.405263157894737,
-0.351986675242114));
#29414=CARTESIAN_POINT('Ctrl Pts',(0.230199463455902,0.43421052631579,-0.524801912662064));
#29415=CARTESIAN_POINT('Ctrl Pts',(-0.0473237183527974,0.463157894736842,
-0.571112341965111));
#29416=CARTESIAN_POINT('Ctrl Pts',(-0.313439397484805,0.492105263157895,
-0.479754713047896));
#29417=CARTESIAN_POINT('Ctrl Pts',(-0.503999728127626,0.521052631578947,
-0.272751013161366));
#29418=CARTESIAN_POINT('Ctrl Pts',(-0.573069664876904,0.55,-2.39751545989516E-16));
#29419=CARTESIAN_POINT('Ctrl Pts',(-0.503999728127627,0.578947368421053,
0.272751013161366));
#29420=CARTESIAN_POINT('Ctrl Pts',(-0.313439397484805,0.607894736842105,
0.479754713047896));
#29421=CARTESIAN_POINT('Ctrl Pts',(-0.0473237183527982,0.636842105263158,
0.571112341965112));
#29422=CARTESIAN_POINT('Ctrl Pts',(0.230199463455903,0.665789473684211,
0.524801912662064));
#29423=CARTESIAN_POINT('Ctrl Pts',(0.452232485289667,0.694736842105263,
0.351986675242114));
#29424=CARTESIAN_POINT('Ctrl Pts',(0.565253745898007,0.723684210526316,
0.0943241631669169));
#29425=CARTESIAN_POINT('Ctrl Pts',(0.542019161337125,0.752631578947369,
-0.186075408839635));
#29426=CARTESIAN_POINT('Ctrl Pts',(0.388129540647024,0.781578947368421,
-0.421621069647034));
#29427=CARTESIAN_POINT('Ctrl Pts',(0.140680250766998,0.810526315789474,
-0.555533855939788));
#29428=CARTESIAN_POINT('Ctrl Pts',(-0.140680214568305,0.839473684210527,
-0.555533945989301));
#29429=CARTESIAN_POINT('Ctrl Pts',(-0.388129668188505,0.868421052631579,
-0.421620932468086));
#29430=CARTESIAN_POINT('Ctrl Pts',(-0.542018875701069,0.897368421052632,
-0.186075664943732));
#29431=CARTESIAN_POINT('Ctrl Pts',(-0.565254339124195,0.926315789473684,
0.0943246722345097));
#29432=CARTESIAN_POINT('Ctrl Pts',(-0.452231273974558,0.955263157894737,
0.351985646771295));
#29433=CARTESIAN_POINT('Ctrl Pts',(-0.23020192721274,0.984210526315789,
0.52480399893423));
#29434=CARTESIAN_POINT('Ctrl Pts',(0.047328728141718,1.01315789473684,0.571108104224167));
#29435=CARTESIAN_POINT('Ctrl Pts',(0.313429112214631,1.04210526315789,0.4797633508545));
#29436=CARTESIAN_POINT('Ctrl Pts',(0.504021197632586,1.07105263157895,0.272733075266706));
#29437=CARTESIAN_POINT('Ctrl Pts',(0.55,1.09035087719298,0.0909408399723365));
#29438=CARTESIAN_POINT('Ctrl Pts',(0.55,1.1,4.04133443718627E-16));
#29439=CARTESIAN_POINT('Ctrl Pts',(0.55,-0.0149599650170943,0.));
#29440=CARTESIAN_POINT('Ctrl Pts',(0.55,-0.0053108422100767,-0.090963337566431));
#29441=CARTESIAN_POINT('Ctrl Pts',(0.504025597995316,0.0139874034039583,
-0.272722100402085));
#29442=CARTESIAN_POINT('Ctrl Pts',(0.313430222123197,0.0429347718250111,
-0.479772059039409));
#29443=CARTESIAN_POINT('Ctrl Pts',(0.0473293473867347,0.0718821402460636,
-0.57110852263267));
#29444=CARTESIAN_POINT('Ctrl Pts',(-0.230203431837132,0.100829508667116,
-0.524808465895466));
#29445=CARTESIAN_POINT('Ctrl Pts',(-0.452233813118511,0.129776877088169,
-0.351986987289247));
#29446=CARTESIAN_POINT('Ctrl Pts',(-0.565257658331638,0.158724245509222,
-0.0943255642817947));
#29447=CARTESIAN_POINT('Ctrl Pts',(-0.54202199880764,0.187671613930274,
0.186076913937926));
#29448=CARTESIAN_POINT('Ctrl Pts',(-0.388131929047426,0.216618982351327,
0.421623293944921));
#29449=CARTESIAN_POINT('Ctrl Pts',(-0.140681025512686,0.245566350772379,
0.555537208898314));
#29450=CARTESIAN_POINT('Ctrl Pts',(0.140681064202504,0.274513719193432,
0.555537057388092));
#29451=CARTESIAN_POINT('Ctrl Pts',(0.388131792728783,0.303461087614485,
0.421623524751422));
#29452=CARTESIAN_POINT('Ctrl Pts',(0.542022304100625,0.332408456035537,
0.186076483037303));
#29453=CARTESIAN_POINT('Ctrl Pts',(0.565257024280752,0.36135582445659,-0.0943247077642448));
#29454=CARTESIAN_POINT('Ctrl Pts',(0.452235107794019,0.390303192877642,
-0.351988717720502));
#29455=CARTESIAN_POINT('Ctrl Pts',(0.230200798529239,0.419250561298696,
-0.524804955578026));
#29456=CARTESIAN_POINT('Ctrl Pts',(-0.0473239928336781,0.448197929719748,
-0.571115654320144));
#29457=CARTESIAN_POINT('Ctrl Pts',(-0.313441215206083,0.477145298140801,
-0.479757495171017));
#29458=CARTESIAN_POINT('Ctrl Pts',(-0.504002650999897,0.506092666561853,
-0.272752594988184));
#29459=CARTESIAN_POINT('Ctrl Pts',(-0.573072988290107,0.535040034982906,
-2.69720489238206E-16));
#29460=CARTESIAN_POINT('Ctrl Pts',(-0.504002650999898,0.563987403403958,
0.272752594988184));
#29461=CARTESIAN_POINT('Ctrl Pts',(-0.313441215206083,0.59293477182501,
0.479757495171017));
#29462=CARTESIAN_POINT('Ctrl Pts',(-0.0473239928336784,0.621882140246064,
0.571115654320144));
#29463=CARTESIAN_POINT('Ctrl Pts',(0.230200798529239,0.650829508667116,
0.524804955578026));
#29464=CARTESIAN_POINT('Ctrl Pts',(0.452235107794019,0.67977687708817,0.351988717720502));
#29465=CARTESIAN_POINT('Ctrl Pts',(0.565257024280752,0.708724245509221,
0.0943247077642448));
#29466=CARTESIAN_POINT('Ctrl Pts',(0.542022304100626,0.737671613930275,
-0.186076483037303));
#29467=CARTESIAN_POINT('Ctrl Pts',(0.388131792728783,0.766618982351327,
-0.421623524751422));
#29468=CARTESIAN_POINT('Ctrl Pts',(0.140681064202504,0.79556635077238,-0.555537057388092));
#29469=CARTESIAN_POINT('Ctrl Pts',(-0.140681025512686,0.824513719193432,
-0.555537208898314));
#29470=CARTESIAN_POINT('Ctrl Pts',(-0.388131929047426,0.853461087614485,
-0.421623293944921));
#29471=CARTESIAN_POINT('Ctrl Pts',(-0.54202199880764,0.882408456035538,
-0.186076913937926));
#29472=CARTESIAN_POINT('Ctrl Pts',(-0.565257658331638,0.911355824456589,
0.094325564281795));
#29473=CARTESIAN_POINT('Ctrl Pts',(-0.452233813118511,0.940303192877643,
0.351986987289247));
#29474=CARTESIAN_POINT('Ctrl Pts',(-0.230203431837132,0.969250561298695,
0.524808465895466));
#29475=CARTESIAN_POINT('Ctrl Pts',(0.0473293473867349,0.998197929719749,
0.57110852263267));
#29476=CARTESIAN_POINT('Ctrl Pts',(0.313430222123197,1.0271452981408,0.47977205903941));
#29477=CARTESIAN_POINT('Ctrl Pts',(0.504025597995316,1.05609266656185,0.272722100402085));
#29478=CARTESIAN_POINT('Ctrl Pts',(0.55,1.07539091217589,0.0909633375664313));
#29479=CARTESIAN_POINT('Ctrl Pts',(0.55,1.08504003498291,4.04133443718627E-16));
#29480=CARTESIAN_POINT('Ctrl Pts',(0.53570113931992,-0.0447553195607142,
0.));
#29481=CARTESIAN_POINT('Ctrl Pts',(0.53570113931992,-0.0351061967536967,
-0.0885671891766316));
#29482=CARTESIAN_POINT('Ctrl Pts',(0.490915856431254,-0.0158079511396616,
-0.265647154764381));
#29483=CARTESIAN_POINT('Ctrl Pts',(0.305280141935785,0.013139417281391,
-0.467286867853663));
#29484=CARTESIAN_POINT('Ctrl Pts',(0.0460980211403113,0.0420867857024435,
-0.556260302160471));
#29485=CARTESIAN_POINT('Ctrl Pts',(-0.224216526816036,0.0710341541234964,
-0.511158320191165));
#29486=CARTESIAN_POINT('Ctrl Pts',(-0.440473139290293,0.0999815225445487,
-0.342834190341978));
#29487=CARTESIAN_POINT('Ctrl Pts',(-0.550557513729943,0.128928890965602,
-0.0918720543302183));
#29488=CARTESIAN_POINT('Ctrl Pts',(-0.527926205961598,0.157876259386654,
0.181237562509432));
#29489=CARTESIAN_POINT('Ctrl Pts',(-0.378038158462228,0.186823627807707,
0.410658677308307));
#29490=CARTESIAN_POINT('Ctrl Pts',(-0.137022482393337,0.215770996228759,
0.541089854146894));
#29491=CARTESIAN_POINT('Ctrl Pts',(0.1370225166126,0.244718364649812,0.54108979205624));
#29492=CARTESIAN_POINT('Ctrl Pts',(0.378038037895015,0.273665733070865,
0.410658771895499));
#29493=CARTESIAN_POINT('Ctrl Pts',(0.527926475978401,0.302613101491917,
0.181237385921362));
#29494=CARTESIAN_POINT('Ctrl Pts',(0.550556952942761,0.331560469912971,
-0.0918717033197569));
#29495=CARTESIAN_POINT('Ctrl Pts',(0.440474284367836,0.360507838334022,
-0.342834899486897));
#29496=CARTESIAN_POINT('Ctrl Pts',(0.224214197783231,0.389455206755076,
-0.511156881721493));
#29497=CARTESIAN_POINT('Ctrl Pts',(-0.0460932852984628,0.418402575176128,
-0.556263223487983));
#29498=CARTESIAN_POINT('Ctrl Pts',(-0.30528986478313,0.44734994359718,-0.46728092468486));
#29499=CARTESIAN_POINT('Ctrl Pts',(-0.490895560929454,0.476297312018233,
-0.265659392490889));
#29500=CARTESIAN_POINT('Ctrl Pts',(-0.558169655449433,0.505244680439286,
-2.99689432486895E-17));
#29501=CARTESIAN_POINT('Ctrl Pts',(-0.490895560929455,0.534192048860338,
0.265659392490888));
#29502=CARTESIAN_POINT('Ctrl Pts',(-0.305289864783131,0.563139417281392,
0.467280924684859));
#29503=CARTESIAN_POINT('Ctrl Pts',(-0.0460932852984632,0.592086785702444,
0.556263223487983));
#29504=CARTESIAN_POINT('Ctrl Pts',(0.224214197783231,0.621034154123497,
0.511156881721493));
#29505=CARTESIAN_POINT('Ctrl Pts',(0.440474284367836,0.649981522544549,
0.342834899486896));
#29506=CARTESIAN_POINT('Ctrl Pts',(0.550556952942761,0.678928890965602,
0.091871703319757));
#29507=CARTESIAN_POINT('Ctrl Pts',(0.527926475978402,0.707876259386654,
-0.181237385921362));
#29508=CARTESIAN_POINT('Ctrl Pts',(0.378038037895015,0.736823627807706,
-0.410658771895499));
#29509=CARTESIAN_POINT('Ctrl Pts',(0.1370225166126,0.76577099622876,-0.54108979205624));
#29510=CARTESIAN_POINT('Ctrl Pts',(-0.137022482393337,0.794718364649812,
-0.541089854146894));
#29511=CARTESIAN_POINT('Ctrl Pts',(-0.378038158462228,0.823665733070864,
-0.410658677308307));
#29512=CARTESIAN_POINT('Ctrl Pts',(-0.527926205961598,0.852613101491918,
-0.181237562509432));
#29513=CARTESIAN_POINT('Ctrl Pts',(-0.550557513729943,0.88156046991297,
0.0918720543302184));
#29514=CARTESIAN_POINT('Ctrl Pts',(-0.440473139290294,0.910507838334022,
0.342834190341979));
#29515=CARTESIAN_POINT('Ctrl Pts',(-0.224216526816034,0.939455206755075,
0.511158320191165));
#29516=CARTESIAN_POINT('Ctrl Pts',(0.0460980211403112,0.968402575176127,
0.556260302160472));
#29517=CARTESIAN_POINT('Ctrl Pts',(0.305280141935785,0.99734994359718,0.467286867853663));
#29518=CARTESIAN_POINT('Ctrl Pts',(0.490915856431254,1.02629731201823,0.265647154764381));
#29519=CARTESIAN_POINT('Ctrl Pts',(0.53570113931992,1.04559555763227,0.088567189176632));
#29520=CARTESIAN_POINT('Ctrl Pts',(0.53570113931992,1.05524468043929,3.93626811340638E-16));
#29521=CARTESIAN_POINT('Ctrl Pts',(0.487277162951485,-0.055780572102217,
0.));
#29522=CARTESIAN_POINT('Ctrl Pts',(0.487277162951485,-0.0461314492951994,
-0.0805709915657102));
#29523=CARTESIAN_POINT('Ctrl Pts',(0.446542084643265,-0.0268332036811644,
-0.241629603004461));
#29524=CARTESIAN_POINT('Ctrl Pts',(0.277685237629778,0.00211416473988834,
-0.425050866224017));
#29525=CARTESIAN_POINT('Ctrl Pts',(0.0419313205272104,0.0310615331609409,
-0.505978088853912));
#29526=CARTESIAN_POINT('Ctrl Pts',(-0.203949428231782,0.0600089015819936,
-0.464954787158114));
#29527=CARTESIAN_POINT('Ctrl Pts',(-0.400658264797364,0.0889562700030461,
-0.311844738436358));
#29528=CARTESIAN_POINT('Ctrl Pts',(-0.50079204861863,0.117903638424099,
-0.0835677899817997));
#29529=CARTESIAN_POINT('Ctrl Pts',(-0.480206382491451,0.146851006845151,
0.164855378621667));
#29530=CARTESIAN_POINT('Ctrl Pts',(-0.343866889053833,0.175798375266204,
0.373538763876965));
#29531=CARTESIAN_POINT('Ctrl Pts',(-0.12463687145299,0.204745743687256,
0.492180180949036));
#29532=CARTESIAN_POINT('Ctrl Pts',(0.124636903654563,0.23369311210831,0.492180097936035));
#29533=CARTESIAN_POINT('Ctrl Pts',(0.343866775595692,0.262640480529362,
0.373538890336684));
#29534=CARTESIAN_POINT('Ctrl Pts',(0.480206636587103,0.291587848950415,
0.164855142529666));
#29535=CARTESIAN_POINT('Ctrl Pts',(0.500791520897454,0.320535217371467,
-0.0835673206929687));
#29536=CARTESIAN_POINT('Ctrl Pts',(0.400659342357064,0.34948258579252,-0.31184568654235));
#29537=CARTESIAN_POINT('Ctrl Pts',(0.203947236527034,0.378429954213572,
-0.464952863901945));
#29538=CARTESIAN_POINT('Ctrl Pts',(-0.0419268639274376,0.407377322634625,
-0.505981995539795));
#29539=CARTESIAN_POINT('Ctrl Pts',(-0.277694387183471,0.436324691055678,
-0.425042901771534));
#29540=CARTESIAN_POINT('Ctrl Pts',(-0.44652298583642,0.465272059476731,
-0.241646155723996));
#29541=CARTESIAN_POINT('Ctrl Pts',(-0.507716102949532,0.494219427897782,
-1.34860244619103E-16));
#29542=CARTESIAN_POINT('Ctrl Pts',(-0.44652298583642,0.523166796318836,
0.241646155723995));
#29543=CARTESIAN_POINT('Ctrl Pts',(-0.277694387183471,0.552114164739888,
0.425042901771534));
#29544=CARTESIAN_POINT('Ctrl Pts',(-0.0419268639274382,0.581061533160941,
0.505981995539795));
#29545=CARTESIAN_POINT('Ctrl Pts',(0.203947236527034,0.610008901581994,
0.464952863901946));
#29546=CARTESIAN_POINT('Ctrl Pts',(0.400659342357062,0.638956270003045,
0.31184568654235));
#29547=CARTESIAN_POINT('Ctrl Pts',(0.500791520897455,0.667903638424099,
0.083567320692969));
#29548=CARTESIAN_POINT('Ctrl Pts',(0.480206636587102,0.696851006845151,
-0.164855142529666));
#29549=CARTESIAN_POINT('Ctrl Pts',(0.343866775595692,0.725798375266205,
-0.373538890336684));
#29550=CARTESIAN_POINT('Ctrl Pts',(0.124636903654563,0.754745743687256,
-0.492180097936035));
#29551=CARTESIAN_POINT('Ctrl Pts',(-0.12463687145299,0.783693112108309,
-0.492180180949036));
#29552=CARTESIAN_POINT('Ctrl Pts',(-0.343866889053832,0.812640480529363,
-0.373538763876965));
#29553=CARTESIAN_POINT('Ctrl Pts',(-0.480206382491451,0.841587848950416,
-0.164855378621666));
#29554=CARTESIAN_POINT('Ctrl Pts',(-0.50079204861863,0.870535217371465,
0.0835677899817997));
#29555=CARTESIAN_POINT('Ctrl Pts',(-0.400658264797365,0.899482585792521,
0.311844738436358));
#29556=CARTESIAN_POINT('Ctrl Pts',(-0.203949428231782,0.928429954213573,
0.464954787158114));
#29557=CARTESIAN_POINT('Ctrl Pts',(0.0419313205272106,0.957377322634626,
0.505978088853912));
#29558=CARTESIAN_POINT('Ctrl Pts',(0.277685237629778,0.986324691055679,
0.425050866224016));
#29559=CARTESIAN_POINT('Ctrl Pts',(0.446542084643265,1.01527205947673,0.241629603004461));
#29560=CARTESIAN_POINT('Ctrl Pts',(0.487277162951485,1.03457030509077,0.0805709915657105));
#29561=CARTESIAN_POINT('Ctrl Pts',(0.487277162951485,1.04421942789778,3.58045450743683E-16));
#29562=CARTESIAN_POINT('Ctrl Pts',(0.448387246880286,-0.0248419023856354,
0.));
#29563=CARTESIAN_POINT('Ctrl Pts',(0.448387246880286,-0.0151927795786178,
-0.07414422645298));
#29564=CARTESIAN_POINT('Ctrl Pts',(0.410903978185472,0.0041054660354173,
-0.222343197653867));
#29565=CARTESIAN_POINT('Ctrl Pts',(0.255523173753345,0.0330528344564699,
-0.391128689006159));
#29566=CARTESIAN_POINT('Ctrl Pts',(0.038584854538714,0.0620002028775224,
-0.465595707447286));
#29567=CARTESIAN_POINT('Ctrl Pts',(-0.187672332794983,0.0909475712985754,
-0.427847161438827));
#29568=CARTESIAN_POINT('Ctrl Pts',(-0.368681873914515,0.119894939719628,
-0.286956419480487));
#29569=CARTESIAN_POINT('Ctrl Pts',(-0.460824040408845,0.14884230814068,
-0.0768983339117788));
#29570=CARTESIAN_POINT('Ctrl Pts',(-0.44188129815593,0.177789676561733,
0.15169836383255));
#29571=CARTESIAN_POINT('Ctrl Pts',(-0.316423010561111,0.206737044982786,
0.343726769588972));
#29572=CARTESIAN_POINT('Ctrl Pts',(-0.114689651347553,0.235684413403838,
0.452899482496333));
#29573=CARTESIAN_POINT('Ctrl Pts',(0.114689681384317,0.264631781824891,
0.45289939611113));
#29574=CARTESIAN_POINT('Ctrl Pts',(0.316422904730401,0.293579150245943,
0.343726901185811));
#29575=CARTESIAN_POINT('Ctrl Pts',(0.441881535169538,0.322526518666996,
0.151698118149882));
#29576=CARTESIAN_POINT('Ctrl Pts',(0.460823548164688,0.351473887088049,
-0.0768978455591534));
#29577=CARTESIAN_POINT('Ctrl Pts',(0.368682879033298,0.380421255509101,
-0.286957406102108));
#29578=CARTESIAN_POINT('Ctrl Pts',(0.187670288431583,0.409368623930155,
-0.427845160036274));
#29579=CARTESIAN_POINT('Ctrl Pts',(-0.0385806975419882,0.438315992351207,
-0.465599773082623));
#29580=CARTESIAN_POINT('Ctrl Pts',(-0.255531708211606,0.467263360772259,
-0.391120396237365));
#29581=CARTESIAN_POINT('Ctrl Pts',(-0.410886163330746,0.496210729193312,
-0.222360471827706));
#29582=CARTESIAN_POINT('Ctrl Pts',(-0.467195482019691,0.525158097614364,
-2.24767074365171E-16));
#29583=CARTESIAN_POINT('Ctrl Pts',(-0.410886163330746,0.554105466035418,
0.222360471827706));
#29584=CARTESIAN_POINT('Ctrl Pts',(-0.255531708211606,0.583052834456469,
0.391120396237364));
#29585=CARTESIAN_POINT('Ctrl Pts',(-0.0385806975419882,0.612000202877523,
0.465599773082623));
#29586=CARTESIAN_POINT('Ctrl Pts',(0.187670288431583,0.640947571298575,
0.427845160036274));
#29587=CARTESIAN_POINT('Ctrl Pts',(0.368682879033298,0.669894939719628,
0.286957406102107));
#29588=CARTESIAN_POINT('Ctrl Pts',(0.460823548164688,0.69884230814068,0.0768978455591535));
#29589=CARTESIAN_POINT('Ctrl Pts',(0.441881535169539,0.727789676561734,
-0.151698118149882));
#29590=CARTESIAN_POINT('Ctrl Pts',(0.316422904730401,0.756737044982785,
-0.34372690118581));
#29591=CARTESIAN_POINT('Ctrl Pts',(0.114689681384317,0.785684413403839,
-0.452899396111131));
#29592=CARTESIAN_POINT('Ctrl Pts',(-0.114689651347553,0.814631781824892,
-0.452899482496332));
#29593=CARTESIAN_POINT('Ctrl Pts',(-0.316423010561111,0.843579150245942,
-0.343726769588972));
#29594=CARTESIAN_POINT('Ctrl Pts',(-0.44188129815593,0.872526518666998,
-0.15169836383255));
#29595=CARTESIAN_POINT('Ctrl Pts',(-0.460824040408845,0.901473887088049,
0.0768983339117786));
#29596=CARTESIAN_POINT('Ctrl Pts',(-0.368681873914516,0.930421255509102,
0.286956419480488));
#29597=CARTESIAN_POINT('Ctrl Pts',(-0.187672332794982,0.959368623930154,
0.427847161438827));
#29598=CARTESIAN_POINT('Ctrl Pts',(0.038584854538714,0.988315992351207,
0.465595707447287));
#29599=CARTESIAN_POINT('Ctrl Pts',(0.255523173753346,1.01726336077226,0.391128689006158));
#29600=CARTESIAN_POINT('Ctrl Pts',(0.410903978185472,1.04621072919331,0.222343197653867));
#29601=CARTESIAN_POINT('Ctrl Pts',(0.448387246880286,1.06550897480735,0.0741442264529802));
#29602=CARTESIAN_POINT('Ctrl Pts',(0.448387246880286,1.07515809761436,3.29469604002262E-16));
#29603=CARTESIAN_POINT('Ctrl Pts',(0.44846989161077,0.0248083822941807,
0.));
#29604=CARTESIAN_POINT('Ctrl Pts',(0.44846989161077,0.0344575051011982,
-0.0741467389671334));
#29605=CARTESIAN_POINT('Ctrl Pts',(0.410977532641741,0.0537557507152332,
-0.22238961986095));
#29606=CARTESIAN_POINT('Ctrl Pts',(0.255569720392287,0.082703119136286,
-0.391196462921687));
#29607=CARTESIAN_POINT('Ctrl Pts',(0.0385916593292064,0.111650487557339,
-0.465681316533805));
#29608=CARTESIAN_POINT('Ctrl Pts',(-0.187706177786097,0.140597855978391,
-0.427923805769893));
#29609=CARTESIAN_POINT('Ctrl Pts',(-0.368748568900195,0.169545224399444,
-0.287008645427576));
#29610=CARTESIAN_POINT('Ctrl Pts',(-0.460907331901607,0.198492592820497,
-0.0769120652267277));
#29611=CARTESIAN_POINT('Ctrl Pts',(-0.441961195426282,0.227439961241549,
0.151725704994062));
#29612=CARTESIAN_POINT('Ctrl Pts',(-0.316480211389712,0.256387329662602,
0.343788953041849));
#29613=CARTESIAN_POINT('Ctrl Pts',(-0.114710388396602,0.285334698083654,
0.452981341280585));
#29614=CARTESIAN_POINT('Ctrl Pts',(0.1147104172039,0.314282066504708,0.45298128534925));
#29615=CARTESIAN_POINT('Ctrl Pts',(0.316480109890866,0.343229434925759,
0.343789038246103));
#29616=CARTESIAN_POINT('Ctrl Pts',(0.441961422738447,0.372176803346812,
0.151725545923318));
#29617=CARTESIAN_POINT('Ctrl Pts',(0.460906859805993,0.401124171767864,
-0.0769117490360455));
#29618=CARTESIAN_POINT('Ctrl Pts',(0.368749532877446,0.430071540188918,
-0.287009284226811));
#29619=CARTESIAN_POINT('Ctrl Pts',(0.1877042171026,0.45901890860997,-0.427922509983804));
#29620=CARTESIAN_POINT('Ctrl Pts',(-0.0385876724867117,0.487966277031022,
-0.46568394821421));
#29621=CARTESIAN_POINT('Ctrl Pts',(-0.255577905518018,0.516913645452076,
-0.391191106531583));
#29622=CARTESIAN_POINT('Ctrl Pts',(-0.410960446984824,0.545861013873128,
-0.222400672107441));
#29623=CARTESIAN_POINT('Ctrl Pts',(-0.467279945783006,0.57480838229418,
-2.99689432486895E-16));
#29624=CARTESIAN_POINT('Ctrl Pts',(-0.410960446984824,0.603755750715233,
0.222400672107441));
#29625=CARTESIAN_POINT('Ctrl Pts',(-0.255577905518018,0.632703119136285,
0.391191106531583));
#29626=CARTESIAN_POINT('Ctrl Pts',(-0.0385876724867119,0.661650487557339,
0.46568394821421));
#29627=CARTESIAN_POINT('Ctrl Pts',(0.1877042171026,0.690597855978391,0.427922509983805));
#29628=CARTESIAN_POINT('Ctrl Pts',(0.368749532877446,0.719545224399444,
0.287009284226811));
#29629=CARTESIAN_POINT('Ctrl Pts',(0.460906859805992,0.748492592820496,
0.0769117490360456));
#29630=CARTESIAN_POINT('Ctrl Pts',(0.441961422738447,0.777439961241549,
-0.151725545923318));
#29631=CARTESIAN_POINT('Ctrl Pts',(0.316480109890866,0.806387329662602,
-0.343789038246102));
#29632=CARTESIAN_POINT('Ctrl Pts',(0.114710417203901,0.835334698083655,
-0.45298128534925));
#29633=CARTESIAN_POINT('Ctrl Pts',(-0.114710388396602,0.864282066504706,
-0.452981341280585));
#29634=CARTESIAN_POINT('Ctrl Pts',(-0.316480211389712,0.89322943492576,
-0.343788953041849));
#29635=CARTESIAN_POINT('Ctrl Pts',(-0.441961195426283,0.922176803346812,
-0.151725704994062));
#29636=CARTESIAN_POINT('Ctrl Pts',(-0.460907331901607,0.951124171767863,
0.0769120652267278));
#29637=CARTESIAN_POINT('Ctrl Pts',(-0.368748568900195,0.980071540188918,
0.287008645427576));
#29638=CARTESIAN_POINT('Ctrl Pts',(-0.187706177786096,1.00901890860997,
0.427923805769892));
#29639=CARTESIAN_POINT('Ctrl Pts',(0.0385916593292065,1.03796627703102,
0.465681316533805));
#29640=CARTESIAN_POINT('Ctrl Pts',(0.255569720392286,1.06691364545207,0.391196462921687));
#29641=CARTESIAN_POINT('Ctrl Pts',(0.410977532641741,1.09586101387313,0.222389619860949));
#29642=CARTESIAN_POINT('Ctrl Pts',(0.44846989161077,1.11515925948716,0.0741467389671337));
#29643=CARTESIAN_POINT('Ctrl Pts',(0.44846989161077,1.12480838229418,3.29530330365054E-16));
#29644=CARTESIAN_POINT('Ctrl Pts',(0.487239979171329,0.0558629369918963,
0.));
#29645=CARTESIAN_POINT('Ctrl Pts',(0.487239979171329,0.0655120597989138,
-0.0805720968838106));
#29646=CARTESIAN_POINT('Ctrl Pts',(0.446509428085615,0.084810305412949,
-0.241607625921821));
#29647=CARTESIAN_POINT('Ctrl Pts',(0.277664405517879,0.113757673834002,
-0.425021238566598));
#29648=CARTESIAN_POINT('Ctrl Pts',(0.0419283204332873,0.142705042255054,
-0.50593961292168));
#29649=CARTESIAN_POINT('Ctrl Pts',(-0.2039343501116,0.171652410676107,-0.46492074701256));
#29650=CARTESIAN_POINT('Ctrl Pts',(-0.400628509511133,0.200599779097159,
-0.311821373989466));
#29651=CARTESIAN_POINT('Ctrl Pts',(-0.500754903699936,0.229547147518212,
-0.0835617005943787));
#29652=CARTESIAN_POINT('Ctrl Pts',(-0.480170745224076,0.258494515939265,
0.164843201321287));
#29653=CARTESIAN_POINT('Ctrl Pts',(-0.343841377753676,0.287441884360317,
0.373511020777802));
#29654=CARTESIAN_POINT('Ctrl Pts',(-0.124627621963577,0.31638925278137,
0.492143675044313));
#29655=CARTESIAN_POINT('Ctrl Pts',(0.124627654965877,0.345336621202422,
0.492143572221594));
#29656=CARTESIAN_POINT('Ctrl Pts',(0.343841261474276,0.374283989623475,
0.373511177415101));
#29657=CARTESIAN_POINT('Ctrl Pts',(0.480171005638091,0.403231358044527,
0.164842908889717));
#29658=CARTESIAN_POINT('Ctrl Pts',(0.500754362856404,0.432178726465581,
-0.0835611193171623));
#29659=CARTESIAN_POINT('Ctrl Pts',(0.400629613865516,0.461126094886633,
-0.311822548347942));
#29660=CARTESIAN_POINT('Ctrl Pts',(0.203932103907749,0.490073463307686,
-0.464918364765013));
#29661=CARTESIAN_POINT('Ctrl Pts',(-0.0419237530153557,0.519020831728739,
-0.505944452370532));
#29662=CARTESIAN_POINT('Ctrl Pts',(-0.27767378258509,0.54796820014979,-0.425011364051589));
#29663=CARTESIAN_POINT('Ctrl Pts',(-0.446489854366344,0.576915568570844,
-0.241628225884321));
#29664=CARTESIAN_POINT('Ctrl Pts',(-0.507678431017099,0.605862936991897,
-2.99689432486895E-16));
#29665=CARTESIAN_POINT('Ctrl Pts',(-0.446489854366344,0.634810305412948,
0.241628225884321));
#29666=CARTESIAN_POINT('Ctrl Pts',(-0.27767378258509,0.663757673834001,
0.425011364051589));
#29667=CARTESIAN_POINT('Ctrl Pts',(-0.041923753015356,0.692705042255054,
0.505944452370533));
#29668=CARTESIAN_POINT('Ctrl Pts',(0.203932103907749,0.721652410676107,
0.464918364765012));
#29669=CARTESIAN_POINT('Ctrl Pts',(0.400629613865516,0.750599779097159,
0.311822548347942));
#29670=CARTESIAN_POINT('Ctrl Pts',(0.500754362856405,0.779547147518212,
0.0835611193171624));
#29671=CARTESIAN_POINT('Ctrl Pts',(0.48017100563809,0.808494515939265,-0.164842908889718));
#29672=CARTESIAN_POINT('Ctrl Pts',(0.343841261474277,0.837441884360317,
-0.3735111774151));
#29673=CARTESIAN_POINT('Ctrl Pts',(0.124627654965877,0.86638925278137,-0.492143572221595));
#29674=CARTESIAN_POINT('Ctrl Pts',(-0.124627621963577,0.895336621202423,
-0.492143675044312));
#29675=CARTESIAN_POINT('Ctrl Pts',(-0.343841377753676,0.924283989623475,
-0.373511020777802));
#29676=CARTESIAN_POINT('Ctrl Pts',(-0.480170745224076,0.953231358044529,
-0.164843201321287));
#29677=CARTESIAN_POINT('Ctrl Pts',(-0.500754903699936,0.98217872646558,
0.0835617005943788));
#29678=CARTESIAN_POINT('Ctrl Pts',(-0.400628509511134,1.01112609488663,
0.311821373989466));
#29679=CARTESIAN_POINT('Ctrl Pts',(-0.203934350111599,1.04007346330769,
0.46492074701256));
#29680=CARTESIAN_POINT('Ctrl Pts',(0.0419283204332873,1.06902083172874,
0.50593961292168));
#29681=CARTESIAN_POINT('Ctrl Pts',(0.277664405517879,1.09796820014979,0.425021238566598));
#29682=CARTESIAN_POINT('Ctrl Pts',(0.446509428085615,1.12691556857084,0.241607625921822));
#29683=CARTESIAN_POINT('Ctrl Pts',(0.487239979171329,1.14621381418488,0.080572096883811));
#29684=CARTESIAN_POINT('Ctrl Pts',(0.487239979171329,1.1558629369919,3.58018128545275E-16));
#29685=CARTESIAN_POINT('Ctrl Pts',(0.535698098014683,0.0446967718358284,
0.));
#29686=CARTESIAN_POINT('Ctrl Pts',(0.535698098014683,0.054345894642846,
-0.0885628977313501));
#29687=CARTESIAN_POINT('Ctrl Pts',(0.49091232835538,0.0736441402568811,
-0.265647494804398));
#29688=CARTESIAN_POINT('Ctrl Pts',(0.305278221876178,0.102591508677934,
-0.467282748481705));
#29689=CARTESIAN_POINT('Ctrl Pts',(0.0460976551488997,0.131538877098987,
-0.556257073675275));
#29690=CARTESIAN_POINT('Ctrl Pts',(-0.224215000503499,0.160486245520039,
-0.511154665978631));
#29691=CARTESIAN_POINT('Ctrl Pts',(-0.440470211021928,0.189433613941092,
-0.342832018243975));
#29692=CARTESIAN_POINT('Ctrl Pts',(-0.550553829122059,0.218380982362144,
-0.0918713825282206));
#29693=CARTESIAN_POINT('Ctrl Pts',(-0.52792268286081,0.247328350783197,
0.181236323247396));
#29694=CARTESIAN_POINT('Ctrl Pts',(-0.378035631515992,0.27627571920425,
0.410655948223274));
#29695=CARTESIAN_POINT('Ctrl Pts',(-0.137021567919262,0.305223087625302,
0.541086232769947));
#29696=CARTESIAN_POINT('Ctrl Pts',(0.137021601718821,0.334170456046355,
0.54108618102972));
#29697=CARTESIAN_POINT('Ctrl Pts',(0.378035512427552,0.363117824467407,
0.410656027042911));
#29698=CARTESIAN_POINT('Ctrl Pts',(0.527922949565824,0.39206519288846,0.181236176096321));
#29699=CARTESIAN_POINT('Ctrl Pts',(0.550553275213,0.421012561309513,-0.0918710900308351));
#29700=CARTESIAN_POINT('Ctrl Pts',(0.440471342054956,0.449959929730565,
-0.3428326091737));
#29701=CARTESIAN_POINT('Ctrl Pts',(0.224212700036564,0.478907298151618,
-0.511153467328439));
#29702=CARTESIAN_POINT('Ctrl Pts',(-0.0460929773927245,0.50785466657267,
-0.556259507641357));
#29703=CARTESIAN_POINT('Ctrl Pts',(-0.305287825471625,0.536802034993724,
-0.467277803304149));
#29704=CARTESIAN_POINT('Ctrl Pts',(-0.490892281780365,0.565749403414775,
-0.265657617896155));
#29705=CARTESIAN_POINT('Ctrl Pts',(-0.55816592691732,0.594696771835828,
-5.39440978476411E-16));
#29706=CARTESIAN_POINT('Ctrl Pts',(-0.490892281780366,0.623644140256882,
0.265657617896155));
#29707=CARTESIAN_POINT('Ctrl Pts',(-0.305287825471625,0.652591508677933,
0.467277803304148));
#29708=CARTESIAN_POINT('Ctrl Pts',(-0.0460929773927249,0.681538877098987,
0.556259507641358));
#29709=CARTESIAN_POINT('Ctrl Pts',(0.224212700036564,0.710486245520039,
0.51115346732844));
#29710=CARTESIAN_POINT('Ctrl Pts',(0.440471342054955,0.739433613941091,
0.342832609173699));
#29711=CARTESIAN_POINT('Ctrl Pts',(0.550553275213,0.768380982362144,0.0918710900308353));
#29712=CARTESIAN_POINT('Ctrl Pts',(0.527922949565824,0.797328350783197,
-0.181236176096321));
#29713=CARTESIAN_POINT('Ctrl Pts',(0.378035512427552,0.82627571920425,-0.410656027042911));
#29714=CARTESIAN_POINT('Ctrl Pts',(0.137021601718821,0.855223087625302,
-0.541086181029719));
#29715=CARTESIAN_POINT('Ctrl Pts',(-0.137021567919262,0.884170456046355,
-0.541086232769948));
#29716=CARTESIAN_POINT('Ctrl Pts',(-0.378035631515992,0.913117824467408,
-0.410655948223274));
#29717=CARTESIAN_POINT('Ctrl Pts',(-0.52792268286081,0.942065192888461,
-0.181236323247396));
#29718=CARTESIAN_POINT('Ctrl Pts',(-0.550553829122059,0.971012561309512,
0.091871382528221));
#29719=CARTESIAN_POINT('Ctrl Pts',(-0.440470211021928,0.999959929730566,
0.342832018243975));
#29720=CARTESIAN_POINT('Ctrl Pts',(-0.224215000503498,1.02890729815162,
0.511154665978631));
#29721=CARTESIAN_POINT('Ctrl Pts',(0.0460976551488998,1.05785466657267,
0.556257073675275));
#29722=CARTESIAN_POINT('Ctrl Pts',(0.305278221876177,1.08680203499372,0.467282748481705));
#29723=CARTESIAN_POINT('Ctrl Pts',(0.49091232835538,1.11574940341478,0.265647494804399));
#29724=CARTESIAN_POINT('Ctrl Pts',(0.535698098014682,1.13504764902881,0.0885628977313504));
#29725=CARTESIAN_POINT('Ctrl Pts',(0.535698098014683,1.14469677183583,3.93624576625804E-16));
#29726=CARTESIAN_POINT('Ctrl Pts',(0.55,0.0149599650170943,0.));
#29727=CARTESIAN_POINT('Ctrl Pts',(0.55,0.0246090878241118,-0.0909662710727813));
#29728=CARTESIAN_POINT('Ctrl Pts',(0.504026171767425,0.0439073334381469,
-0.272720669367508));
#29729=CARTESIAN_POINT('Ctrl Pts',(0.313430366846398,0.0728547018591995,
-0.47977319451708));
#29730=CARTESIAN_POINT('Ctrl Pts',(0.0473294281313326,0.101802070280252,
-0.571108577189793));
#29731=CARTESIAN_POINT('Ctrl Pts',(-0.23020362802812,0.130749438701305,
-0.524809048351488));
#29732=CARTESIAN_POINT('Ctrl Pts',(-0.452234144202576,0.159696807122357,
-0.351987162082067));
#29733=CARTESIAN_POINT('Ctrl Pts',(-0.565258091129744,0.18864417554341,
-0.094325680597627));
#29734=CARTESIAN_POINT('Ctrl Pts',(-0.54202240603576,0.217591543964463,
0.18607707679678));
#29735=CARTESIAN_POINT('Ctrl Pts',(-0.388132223845349,0.246538912385515,
0.421623601862615));
#29736=CARTESIAN_POINT('Ctrl Pts',(-0.140681131253348,0.275486280806568,
0.555537634355555));
#29737=CARTESIAN_POINT('Ctrl Pts',(0.140681170267988,0.304433649227621,
0.555537474831348));
#29738=CARTESIAN_POINT('Ctrl Pts',(0.388132086382233,0.333381017648673,
0.4216238448774));
#29739=CARTESIAN_POINT('Ctrl Pts',(0.542022713891853,0.362328386069726,
0.186076623104089));
#29740=CARTESIAN_POINT('Ctrl Pts',(0.565257451755643,0.391275754490779,
-0.0943247787753811));
#29741=CARTESIAN_POINT('Ctrl Pts',(0.452235449747614,0.420223122911831,
-0.35198898404335));
#29742=CARTESIAN_POINT('Ctrl Pts',(0.230200972612125,0.449170491332884,
-0.524805352349932));
#29743=CARTESIAN_POINT('Ctrl Pts',(-0.0473240286237898,0.478117859753936,
-0.57111608622475));
#29744=CARTESIAN_POINT('Ctrl Pts',(-0.313441452222401,0.507065228174989,
-0.479757857937623));
#29745=CARTESIAN_POINT('Ctrl Pts',(-0.504003032119066,0.536012596596042,
-0.272752801245751));
#29746=CARTESIAN_POINT('Ctrl Pts',(-0.573073421636609,0.564959965017094,
-2.99689432486895E-16));
#29747=CARTESIAN_POINT('Ctrl Pts',(-0.504003032119067,0.593907333438147,
0.27275280124575));
#29748=CARTESIAN_POINT('Ctrl Pts',(-0.313441452222401,0.6228547018592,0.479757857937623));
#29749=CARTESIAN_POINT('Ctrl Pts',(-0.0473240286237902,0.651802070280252,
0.57111608622475));
#29750=CARTESIAN_POINT('Ctrl Pts',(0.230200972612125,0.680749438701306,
0.524805352349932));
#29751=CARTESIAN_POINT('Ctrl Pts',(0.452235449747613,0.709696807122357,
0.35198898404335));
#29752=CARTESIAN_POINT('Ctrl Pts',(0.565257451755644,0.73864417554341,0.0943247787753813));
#29753=CARTESIAN_POINT('Ctrl Pts',(0.542022713891852,0.767591543964463,
-0.186076623104089));
#29754=CARTESIAN_POINT('Ctrl Pts',(0.388132086382234,0.796538912385515,
-0.4216238448774));
#29755=CARTESIAN_POINT('Ctrl Pts',(0.140681170267989,0.825486280806568,
-0.555537474831348));
#29756=CARTESIAN_POINT('Ctrl Pts',(-0.140681131253348,0.854433649227621,
-0.555537634355555));
#29757=CARTESIAN_POINT('Ctrl Pts',(-0.388132223845348,0.883381017648673,
-0.421623601862615));
#29758=CARTESIAN_POINT('Ctrl Pts',(-0.542022406035761,0.912328386069727,
-0.18607707679678));
#29759=CARTESIAN_POINT('Ctrl Pts',(-0.565258091129743,0.941275754490777,
0.0943256805976271));
#29760=CARTESIAN_POINT('Ctrl Pts',(-0.452234144202576,0.970223122911832,
0.351987162082068));
#29761=CARTESIAN_POINT('Ctrl Pts',(-0.230203628028119,0.999170491332883,
0.524809048351488));
#29762=CARTESIAN_POINT('Ctrl Pts',(0.0473294281313327,1.02811785975394,
0.571108577189792));
#29763=CARTESIAN_POINT('Ctrl Pts',(0.313430366846398,1.05706522817499,0.47977319451708));
#29764=CARTESIAN_POINT('Ctrl Pts',(0.504026171767425,1.08601259659604,0.272720669367508));
#29765=CARTESIAN_POINT('Ctrl Pts',(0.55,1.10531084221008,0.0909662710727816));
#29766=CARTESIAN_POINT('Ctrl Pts',(0.55,1.11495996501709,4.04133443718627E-16));
#29767=CARTESIAN_POINT('Ctrl Pts',(0.55,6.12323399573676E-18,0.));
#29768=CARTESIAN_POINT('Ctrl Pts',(0.55,0.00964912280701755,-0.0909408399723361));
#29769=CARTESIAN_POINT('Ctrl Pts',(0.504021197632585,0.0289473684210526,
-0.272733075266705));
#29770=CARTESIAN_POINT('Ctrl Pts',(0.313429112214632,0.0578947368421053,
-0.4797633508545));
#29771=CARTESIAN_POINT('Ctrl Pts',(0.0473287281417178,0.0868421052631579,
-0.571108104224167));
#29772=CARTESIAN_POINT('Ctrl Pts',(-0.230201927212741,0.115789473684211,
-0.52480399893423));
#29773=CARTESIAN_POINT('Ctrl Pts',(-0.452231273974558,0.144736842105263,
-0.351985646771294));
#29774=CARTESIAN_POINT('Ctrl Pts',(-0.565254339124195,0.173684210526316,
-0.0943246722345097));
#29775=CARTESIAN_POINT('Ctrl Pts',(-0.542018875701069,0.202631578947368,
0.186075664943732));
#29776=CARTESIAN_POINT('Ctrl Pts',(-0.388129668188505,0.231578947368421,
0.421620932468086));
#29777=CARTESIAN_POINT('Ctrl Pts',(-0.140680214568305,0.260526315789474,
0.555533945989301));
#29778=CARTESIAN_POINT('Ctrl Pts',(0.140680250766997,0.289473684210526,
0.555533855939788));
#29779=CARTESIAN_POINT('Ctrl Pts',(0.388129540647023,0.318421052631579,
0.421621069647034));
#29780=CARTESIAN_POINT('Ctrl Pts',(0.542019161337126,0.347368421052632,
0.186075408839635));
#29781=CARTESIAN_POINT('Ctrl Pts',(0.565253745898005,0.376315789473684,
-0.0943241631669167));
#29782=CARTESIAN_POINT('Ctrl Pts',(0.452232485289668,0.405263157894737,
-0.351986675242114));
#29783=CARTESIAN_POINT('Ctrl Pts',(0.230199463455902,0.43421052631579,-0.524801912662064));
#29784=CARTESIAN_POINT('Ctrl Pts',(-0.0473237183527974,0.463157894736842,
-0.571112341965111));
#29785=CARTESIAN_POINT('Ctrl Pts',(-0.313439397484805,0.492105263157895,
-0.479754713047896));
#29786=CARTESIAN_POINT('Ctrl Pts',(-0.503999728127626,0.521052631578947,
-0.272751013161366));
#29787=CARTESIAN_POINT('Ctrl Pts',(-0.573069664876904,0.55,-2.39751545989516E-16));
#29788=CARTESIAN_POINT('Ctrl Pts',(-0.503999728127627,0.578947368421053,
0.272751013161366));
#29789=CARTESIAN_POINT('Ctrl Pts',(-0.313439397484805,0.607894736842105,
0.479754713047896));
#29790=CARTESIAN_POINT('Ctrl Pts',(-0.0473237183527982,0.636842105263158,
0.571112341965112));
#29791=CARTESIAN_POINT('Ctrl Pts',(0.230199463455903,0.665789473684211,
0.524801912662064));
#29792=CARTESIAN_POINT('Ctrl Pts',(0.452232485289667,0.694736842105263,
0.351986675242114));
#29793=CARTESIAN_POINT('Ctrl Pts',(0.565253745898007,0.723684210526316,
0.0943241631669169));
#29794=CARTESIAN_POINT('Ctrl Pts',(0.542019161337125,0.752631578947369,
-0.186075408839635));
#29795=CARTESIAN_POINT('Ctrl Pts',(0.388129540647024,0.781578947368421,
-0.421621069647034));
#29796=CARTESIAN_POINT('Ctrl Pts',(0.140680250766998,0.810526315789474,
-0.555533855939788));
#29797=CARTESIAN_POINT('Ctrl Pts',(-0.140680214568305,0.839473684210527,
-0.555533945989301));
#29798=CARTESIAN_POINT('Ctrl Pts',(-0.388129668188505,0.868421052631579,
-0.421620932468086));
#29799=CARTESIAN_POINT('Ctrl Pts',(-0.542018875701069,0.897368421052632,
-0.186075664943732));
#29800=CARTESIAN_POINT('Ctrl Pts',(-0.565254339124195,0.926315789473684,
0.0943246722345097));
#29801=CARTESIAN_POINT('Ctrl Pts',(-0.452231273974558,0.955263157894737,
0.351985646771295));
#29802=CARTESIAN_POINT('Ctrl Pts',(-0.23020192721274,0.984210526315789,
0.52480399893423));
#29803=CARTESIAN_POINT('Ctrl Pts',(0.047328728141718,1.01315789473684,0.571108104224167));
#29804=CARTESIAN_POINT('Ctrl Pts',(0.313429112214631,1.04210526315789,0.4797633508545));
#29805=CARTESIAN_POINT('Ctrl Pts',(0.504021197632586,1.07105263157895,0.272733075266706));
#29806=CARTESIAN_POINT('Ctrl Pts',(0.55,1.09035087719298,0.0909408399723365));
#29807=CARTESIAN_POINT('Ctrl Pts',(0.55,1.1,4.04133443718627E-16));
#29808=CARTESIAN_POINT('',(0.55,-6.12323399573676E-18,0.));
#29809=CARTESIAN_POINT('Origin',(0.5,0.,0.));
#29810=CARTESIAN_POINT('',(0.55,1.1,4.04133443718627E-16));
#29811=CARTESIAN_POINT('Ctrl Pts',(0.55,6.12323399573676E-18,0.));
#29812=CARTESIAN_POINT('Ctrl Pts',(0.55,0.00964912280701755,-0.0909408399723361));
#29813=CARTESIAN_POINT('Ctrl Pts',(0.504021197632585,0.0289473684210526,
-0.272733075266705));
#29814=CARTESIAN_POINT('Ctrl Pts',(0.313429112214632,0.0578947368421053,
-0.4797633508545));
#29815=CARTESIAN_POINT('Ctrl Pts',(0.0473287281417178,0.0868421052631579,
-0.571108104224167));
#29816=CARTESIAN_POINT('Ctrl Pts',(-0.230201927212741,0.115789473684211,
-0.52480399893423));
#29817=CARTESIAN_POINT('Ctrl Pts',(-0.452231273974558,0.144736842105263,
-0.351985646771294));
#29818=CARTESIAN_POINT('Ctrl Pts',(-0.565254339124195,0.173684210526316,
-0.0943246722345097));
#29819=CARTESIAN_POINT('Ctrl Pts',(-0.542018875701069,0.202631578947368,
0.186075664943732));
#29820=CARTESIAN_POINT('Ctrl Pts',(-0.388129668188505,0.231578947368421,
0.421620932468086));
#29821=CARTESIAN_POINT('Ctrl Pts',(-0.140680214568305,0.260526315789474,
0.555533945989301));
#29822=CARTESIAN_POINT('Ctrl Pts',(0.140680250766997,0.289473684210526,
0.555533855939788));
#29823=CARTESIAN_POINT('Ctrl Pts',(0.388129540647023,0.318421052631579,
0.421621069647034));
#29824=CARTESIAN_POINT('Ctrl Pts',(0.542019161337126,0.347368421052632,
0.186075408839635));
#29825=CARTESIAN_POINT('Ctrl Pts',(0.565253745898005,0.376315789473684,
-0.0943241631669167));
#29826=CARTESIAN_POINT('Ctrl Pts',(0.452232485289668,0.405263157894737,
-0.351986675242114));
#29827=CARTESIAN_POINT('Ctrl Pts',(0.230199463455902,0.43421052631579,-0.524801912662064));
#29828=CARTESIAN_POINT('Ctrl Pts',(-0.0473237183527974,0.463157894736842,
-0.571112341965111));
#29829=CARTESIAN_POINT('Ctrl Pts',(-0.313439397484805,0.492105263157895,
-0.479754713047896));
#29830=CARTESIAN_POINT('Ctrl Pts',(-0.503999728127626,0.521052631578947,
-0.272751013161366));
#29831=CARTESIAN_POINT('Ctrl Pts',(-0.573069664876904,0.55,-2.39751545989516E-16));
#29832=CARTESIAN_POINT('Ctrl Pts',(-0.503999728127627,0.578947368421053,
0.272751013161366));
#29833=CARTESIAN_POINT('Ctrl Pts',(-0.313439397484805,0.607894736842105,
0.479754713047896));
#29834=CARTESIAN_POINT('Ctrl Pts',(-0.0473237183527982,0.636842105263158,
0.571112341965112));
#29835=CARTESIAN_POINT('Ctrl Pts',(0.230199463455903,0.665789473684211,
0.524801912662064));
#29836=CARTESIAN_POINT('Ctrl Pts',(0.452232485289667,0.694736842105263,
0.351986675242114));
#29837=CARTESIAN_POINT('Ctrl Pts',(0.565253745898007,0.723684210526316,
0.0943241631669169));
#29838=CARTESIAN_POINT('Ctrl Pts',(0.542019161337125,0.752631578947369,
-0.186075408839635));
#29839=CARTESIAN_POINT('Ctrl Pts',(0.388129540647024,0.781578947368421,
-0.421621069647034));
#29840=CARTESIAN_POINT('Ctrl Pts',(0.140680250766998,0.810526315789474,
-0.555533855939788));
#29841=CARTESIAN_POINT('Ctrl Pts',(-0.140680214568305,0.839473684210527,
-0.555533945989301));
#29842=CARTESIAN_POINT('Ctrl Pts',(-0.388129668188505,0.868421052631579,
-0.421620932468086));
#29843=CARTESIAN_POINT('Ctrl Pts',(-0.542018875701069,0.897368421052632,
-0.186075664943732));
#29844=CARTESIAN_POINT('Ctrl Pts',(-0.565254339124195,0.926315789473684,
0.0943246722345097));
#29845=CARTESIAN_POINT('Ctrl Pts',(-0.452231273974558,0.955263157894737,
0.351985646771295));
#29846=CARTESIAN_POINT('Ctrl Pts',(-0.23020192721274,0.984210526315789,
0.52480399893423));
#29847=CARTESIAN_POINT('Ctrl Pts',(0.047328728141718,1.01315789473684,0.571108104224167));
#29848=CARTESIAN_POINT('Ctrl Pts',(0.313429112214631,1.04210526315789,0.4797633508545));
#29849=CARTESIAN_POINT('Ctrl Pts',(0.504021197632586,1.07105263157895,0.272733075266706));
#29850=CARTESIAN_POINT('Ctrl Pts',(0.55,1.09035087719298,0.0909408399723365));
#29851=CARTESIAN_POINT('Ctrl Pts',(0.55,1.1,4.04133443718627E-16));
#29852=CARTESIAN_POINT('Origin',(0.5,1.1,3.67394039744206E-16));
#29853=CARTESIAN_POINT('Origin',(0.5,1.1,3.67394039744206E-16));
#29854=CARTESIAN_POINT('Origin',(0.5,7.2280144832367E-19,0.));
#29855=CARTESIAN_POINT('',(0.,0.,0.));
#29856=CARTESIAN_POINT('Origin',(0.,0.,1.3));
#29857=CARTESIAN_POINT('',(0.166752921449725,-0.000121400228749406,1.61285196366098));
#29858=CARTESIAN_POINT('',(0.166796959880497,9.66735530056473E-5,1.63214803633902));
#29859=CARTESIAN_POINT('',(0.1666,2.04026156737949E-17,1.3));
#29860=CARTESIAN_POINT('',(0.163512932725146,-0.0319230454628286,1.7));
#29861=CARTESIAN_POINT('Ctrl Pts',(0.166796959880497,9.66735530056473E-5,
1.63214803633902));
#29862=CARTESIAN_POINT('Ctrl Pts',(0.166837734552074,0.00590520031683778,
1.63253777944574));
#29863=CARTESIAN_POINT('Ctrl Pts',(0.166560755157907,0.0117098399368759,
1.63292752255246));
#29864=CARTESIAN_POINT('Ctrl Pts',(0.165953190799148,0.0174796970799782,
1.63331726565918));
#29865=CARTESIAN_POINT('Ctrl Pts',(0.160178154195734,0.0723234938194388,
1.63702186201144));
#29866=CARTESIAN_POINT('Ctrl Pts',(0.124534989745148,0.12402471730472,1.64072645836371));
#29867=CARTESIAN_POINT('Ctrl Pts',(0.0753220427557469,0.148912116862319,
1.64443105471598));
#29868=CARTESIAN_POINT('Ctrl Pts',(0.0261090957663466,0.173799516419917,
1.64813565106825));
#29869=CARTESIAN_POINT('Ctrl Pts',(-0.0366736337618685,0.171873092049834,
1.65184024742052));
#29870=CARTESIAN_POINT('Ctrl Pts',(-0.0842665124811252,0.144033445936741,
1.65554484377278));
#29871=CARTESIAN_POINT('Ctrl Pts',(-0.131859391200383,0.116193799823647,
1.65924944012505));
#29872=CARTESIAN_POINT('Ctrl Pts',(-0.164262419110682,0.0624409319675427,
1.66295403647732));
#29873=CARTESIAN_POINT('Ctrl Pts',(-0.16669782361829,0.00733866012848643,
1.66665863282959));
#29874=CARTESIAN_POINT('Ctrl Pts',(-0.169133228125899,-0.0477636117105698,
1.67036322918185));
#29875=CARTESIAN_POINT('Ctrl Pts',(-0.141601009230818,-0.104215287532578,
1.67406782553412));
#29876=CARTESIAN_POINT('Ctrl Pts',(-0.0965988342506402,-0.136109501609562,
1.67777242188639));
#29877=CARTESIAN_POINT('Ctrl Pts',(-0.0515966592704642,-0.168003715686544,
1.68147701823866));
#29878=CARTESIAN_POINT('Ctrl Pts',(0.0108754717948065,-0.175340468018505,
1.68518161459093));
#29879=CARTESIAN_POINT('Ctrl Pts',(0.0619990767693629,-0.154913285529167,
1.6888862109432));
#29880=CARTESIAN_POINT('Ctrl Pts',(0.11312268174392,-0.134486103039829,
1.69259080729546));
#29881=CARTESIAN_POINT('Ctrl Pts',(0.152897760627763,-0.0862949857291919,
1.69629540364773));
#29882=CARTESIAN_POINT('Ctrl Pts',(0.163512932725146,-0.0319230454628286,
1.7));
#29883=CARTESIAN_POINT('',(0.0052623718904234,0.166820541544646,1.7));
#29884=CARTESIAN_POINT('Origin',(0.,0.,1.7));
#29885=CARTESIAN_POINT('',(0.166340825374871,-6.57396331519428E-5,1.68285196366098));
#29886=CARTESIAN_POINT('Ctrl Pts',(0.00526237188778958,0.16682061735739,
1.7));
#29887=CARTESIAN_POINT('Ctrl Pts',(0.059315846276127,0.165049198896683,
1.69636770818144));
#29888=CARTESIAN_POINT('Ctrl Pts',(0.112514618214038,0.134574177622605,
1.69273541636289));
#29889=CARTESIAN_POINT('Ctrl Pts',(0.141280425894631,0.0887797885328044,
1.68910312454433));
#29890=CARTESIAN_POINT('Ctrl Pts',(0.157782375695069,0.0625091300380853,
1.68701940424988));
#29891=CARTESIAN_POINT('Ctrl Pts',(0.166243631438541,0.0311969895334432,
1.68493568395543));
#29892=CARTESIAN_POINT('Ctrl Pts',(0.166340825374871,-6.57396331519428E-5,
1.68285196366098));
#29893=CARTESIAN_POINT('',(0.1666,-2.04026156737949E-17,1.8));
#29894=CARTESIAN_POINT('',(0.1666,2.04026156737949E-17,1.3));
#29895=CARTESIAN_POINT('Origin',(0.,0.,1.8));
#29896=CARTESIAN_POINT('Ctrl Pts',(0.166340825374871,-6.57396331519428E-5,
1.68285196366098));
#29897=CARTESIAN_POINT('Ctrl Pts',(0.166416430207622,-0.024384267097259,
1.68123108760316));
#29898=CARTESIAN_POINT('Ctrl Pts',(0.161431015607884,-0.0486728962000426,
1.67961021154535));
#29899=CARTESIAN_POINT('Ctrl Pts',(0.151232376946182,-0.070535415398117,
1.67798933548753));
#29900=CARTESIAN_POINT('Ctrl Pts',(0.12792285898394,-0.120503337672002,
1.67428473913526));
#29901=CARTESIAN_POINT('Ctrl Pts',(0.0773807749454364,-0.157797874435697,
1.67058014278299));
#29902=CARTESIAN_POINT('Ctrl Pts',(0.0227482513872868,-0.165320125260105,
1.66687554643073));
#29903=CARTESIAN_POINT('Ctrl Pts',(-0.0318842721708627,-0.172842376084512,
1.66317095007846));
#29904=CARTESIAN_POINT('Ctrl Pts',(-0.0906072352486578,-0.150592340969633,
1.65946635372619));
#29905=CARTESIAN_POINT('Ctrl Pts',(-0.126551605667113,-0.108768963100728,
1.65576175737392));
#29906=CARTESIAN_POINT('Ctrl Pts',(-0.162495976085569,-0.0669455852318239,
1.65205716102165));
#29907=CARTESIAN_POINT('Ctrl Pts',(-0.175661753844685,-0.00554886460889432,
1.64835256466938));
#29908=CARTESIAN_POINT('Ctrl Pts',(-0.160020484350268,0.0473310422055452,
1.64464796831712));
#29909=CARTESIAN_POINT('Ctrl Pts',(-0.144379214855851,0.100210949019985,
1.64094337196485));
#29910=CARTESIAN_POINT('Ctrl Pts',(-0.0999308981078997,0.144574042025934,
1.63723877561258));
#29911=CARTESIAN_POINT('Ctrl Pts',(-0.0470191573240233,0.160112912591645,
1.63353417926031));
#29912=CARTESIAN_POINT('Ctrl Pts',(0.00589258345985309,0.175651783157355,
1.62982958290805));
#29913=CARTESIAN_POINT('Ctrl Pts',(0.067267748279655,0.162366431282826,
1.62612498655578));
#29914=CARTESIAN_POINT('Ctrl Pts',(0.109018480103692,0.126339265236092,
1.62242039020351));
#29915=CARTESIAN_POINT('Ctrl Pts',(0.144963809686008,0.0953216446845623,
1.61923091468933));
#29916=CARTESIAN_POINT('Ctrl Pts',(0.166362794628908,0.0474469630018487,
1.61604143917516));
#29917=CARTESIAN_POINT('Ctrl Pts',(0.166752921449725,-0.000121400228749406,
1.61285196366098));
#29918=CARTESIAN_POINT('Origin',(0.,0.,1.3));
#29919=CARTESIAN_POINT('',(0.166721717270512,0.00013247748987999,1.54285196366098));
#29920=CARTESIAN_POINT('',(0.166368100504911,8.32215516180224E-5,1.56214803633902));
#29921=CARTESIAN_POINT('',(0.1666,2.04026156737949E-17,1.3));
#29922=CARTESIAN_POINT('Ctrl Pts',(0.166368100504911,8.32215516180223E-5,
1.56214803633902));
#29923=CARTESIAN_POINT('Ctrl Pts',(0.166469575983711,0.0225191704554514,
1.56364353466546));
#29924=CARTESIAN_POINT('Ctrl Pts',(0.162248711501603,0.0449185271683059,
1.56513903299191));
#29925=CARTESIAN_POINT('Ctrl Pts',(0.153524147106197,0.0653993692500711,
1.56663453131835));
#29926=CARTESIAN_POINT('Ctrl Pts',(0.131911960142923,0.116133797718439,
1.57033912767062));
#29927=CARTESIAN_POINT('Ctrl Pts',(0.0826635066749161,0.155095554237362,
1.57404372402289));
#29928=CARTESIAN_POINT('Ctrl Pts',(0.028317337914343,0.164453369456362,
1.57774832037515));
#29929=CARTESIAN_POINT('Ctrl Pts',(-0.026028830846231,0.173811184675361,
1.58145291672742));
#29930=CARTESIAN_POINT('Ctrl Pts',(-0.0854727148993724,0.153565058594437,
1.58515751307969));
#29931=CARTESIAN_POINT('Ctrl Pts',(-0.122808942133701,0.11298112966685,
1.58886210943196));
#29932=CARTESIAN_POINT('Ctrl Pts',(-0.160145169368031,0.0723972007392629,
1.59256670578423));
#29933=CARTESIAN_POINT('Ctrl Pts',(-0.175373739783547,0.0114754689650147,
1.59627130213649));
#29934=CARTESIAN_POINT('Ctrl Pts',(-0.161526248741115,-0.041903625100424,
1.59997589848876));
#29935=CARTESIAN_POINT('Ctrl Pts',(-0.147678757698683,-0.0952827191658612,
1.60368049484103));
#29936=CARTESIAN_POINT('Ctrl Pts',(-0.1047552051983,-0.14111917552249,1.6073850911933));
#29937=CARTESIAN_POINT('Ctrl Pts',(-0.0523978126792817,-0.158434271662077,
1.61108968754557));
#29938=CARTESIAN_POINT('Ctrl Pts',(-4.04201602626775E-5,-0.175749367801665,
1.61479428389783));
#29939=CARTESIAN_POINT('Ctrl Pts',(0.0617508123773913,-0.164543103724215,
1.6184988802501));
#29940=CARTESIAN_POINT('Ctrl Pts',(0.104692974268098,-0.12994678668867,
1.62220347660237));
#29941=CARTESIAN_POINT('Ctrl Pts',(0.143117393875163,-0.0989901849689851,
1.62551832984792));
#29942=CARTESIAN_POINT('Ctrl Pts',(0.166450162079376,-0.0493061599110598,
1.62883318309347));
#29943=CARTESIAN_POINT('Ctrl Pts',(0.166796959880497,9.66735530056473E-5,
1.63214803633902));
#29944=CARTESIAN_POINT('Ctrl Pts',(0.166752921449725,-0.000121400228749406,
1.61285196366098));
#29945=CARTESIAN_POINT('Ctrl Pts',(0.166815929443988,-0.00780399726549495,
1.61233684282289));
#29946=CARTESIAN_POINT('Ctrl Pts',(0.166330935441723,-0.0154786041905287,
1.6118217219848));
#29947=CARTESIAN_POINT('Ctrl Pts',(0.165270714247807,-0.0230729153352646,
1.61130660114671));
#29948=CARTESIAN_POINT('Ctrl Pts',(0.157645917739612,-0.0776889496409508,
1.60760200479444));
#29949=CARTESIAN_POINT('Ctrl Pts',(0.120270025894947,-0.128152038033383,
1.60389740844217));
#29950=CARTESIAN_POINT('Ctrl Pts',(0.0702485553938763,-0.151366836780329,
1.6001928120899));
#29951=CARTESIAN_POINT('Ctrl Pts',(0.0202270848928061,-0.174581635527273,
1.59648821573763));
#29952=CARTESIAN_POINT('Ctrl Pts',(-0.0424399642646696,-0.170548144628732,
1.59278361938537));
#29953=CARTESIAN_POINT('Ctrl Pts',(-0.0890727806898626,-0.141112640607554,
1.5890790230331));
#29954=CARTESIAN_POINT('Ctrl Pts',(-0.135705597115056,-0.111677136586376,
1.58537442668083));
#29955=CARTESIAN_POINT('Ctrl Pts',(-0.166304180807966,-0.0568396194425618,
1.58166983032856));
#29956=CARTESIAN_POINT('Ctrl Pts',(-0.16686485427816,-0.00169661928996206,
1.57796523397629));
#29957=CARTESIAN_POINT('Ctrl Pts',(-0.167425527748354,0.0534463808626376,
1.57426063762402));
#29958=CARTESIAN_POINT('Ctrl Pts',(-0.137948290995833,0.108894864024023,
1.57055604127176));
#29959=CARTESIAN_POINT('Ctrl Pts',(-0.0919236010333964,0.139272428377062,
1.56685144491949));
#29960=CARTESIAN_POINT('Ctrl Pts',(-0.0458989110709602,0.169649992730101,
1.56314684856722));
#29961=CARTESIAN_POINT('Ctrl Pts',(0.0166732321013904,0.174956638274794,
1.55944225221495));
#29962=CARTESIAN_POINT('Ctrl Pts',(0.0671563493099001,0.152763795116617,
1.55573765586268));
#29963=CARTESIAN_POINT('Ctrl Pts',(0.117639466518409,0.13057095195844,1.55203305951042));
#29964=CARTESIAN_POINT('Ctrl Pts',(0.156033557763077,0.0808786200973942,
1.54832846315815));
#29965=CARTESIAN_POINT('Ctrl Pts',(0.164767340619488,0.0264287526812992,
1.54462386680588));
#29966=CARTESIAN_POINT('Ctrl Pts',(0.166159792575437,0.0177476547388351,
1.54403323242425));
#29967=CARTESIAN_POINT('Ctrl Pts',(0.166798314017023,0.0089456257803759,
1.54344259804261));
#29968=CARTESIAN_POINT('Ctrl Pts',(0.166721717270512,0.00013247748987999,
1.54285196366098));
#29969=CARTESIAN_POINT('Origin',(0.,0.,1.3));
#29970=CARTESIAN_POINT('',(0.166334949033457,3.80241454671915E-5,1.47285196366098));
#29971=CARTESIAN_POINT('',(0.166495616539739,-0.000143126867227327,1.49214803633902));
#29972=CARTESIAN_POINT('',(0.1666,2.04026156737949E-17,1.3));
#29973=CARTESIAN_POINT('Ctrl Pts',(0.166495616539739,-0.000143126867227327,
1.49214803633902));
#29974=CARTESIAN_POINT('Ctrl Pts',(0.166176505544999,0.0388065957770001,
1.49474928988519));
#29975=CARTESIAN_POINT('Ctrl Pts',(0.15254095518154,0.0779576027494656,
1.49735054343136));
#29976=CARTESIAN_POINT('Ctrl Pts',(0.127581990737563,0.107562045989894,
1.49995179697752));
#29977=CARTESIAN_POINT('Ctrl Pts',(0.0920364789316288,0.149723454131357,
1.50365639332979));
#29978=CARTESIAN_POINT('Ctrl Pts',(0.0335245204022979,0.172522270232617,
1.50736098968206));
#29979=CARTESIAN_POINT('Ctrl Pts',(-0.0211755609783529,0.165524482759979,
1.51106558603433));
#29980=CARTESIAN_POINT('Ctrl Pts',(-0.0758756423590036,0.158526695287341,
1.5147701823866));
#29981=CARTESIAN_POINT('Ctrl Pts',(-0.126763846590974,0.121732304240806,
1.51847477873887));
#29982=CARTESIAN_POINT('Ctrl Pts',(-0.150550887470885,0.0719804791091254,
1.52217937509113));
#29983=CARTESIAN_POINT('Ctrl Pts',(-0.174337928350795,0.0222286539774451,
1.5258839714434));
#29984=CARTESIAN_POINT('Ctrl Pts',(-0.171023805878645,-0.0404806052393804,
1.52958856779567));
#29985=CARTESIAN_POINT('Ctrl Pts',(-0.142125268024159,-0.0874480653886775,
1.53329316414794));
#29986=CARTESIAN_POINT('Ctrl Pts',(-0.113226730169674,-0.134415525537975,
1.5369977605002));
#29987=CARTESIAN_POINT('Ctrl Pts',(-0.058743776932853,-0.165641186619743,
1.54070235685247));
#29988=CARTESIAN_POINT('Ctrl Pts',(-0.00361080053401195,-0.166834419219364,
1.54440695320474));
#29989=CARTESIAN_POINT('Ctrl Pts',(0.0515221758648292,-0.168027651818985,
1.54811154955701));
#29990=CARTESIAN_POINT('Ctrl Pts',(0.10730517542569,-0.139188455936458,
1.55181614590928));
#29991=CARTESIAN_POINT('Ctrl Pts',(0.138208714976851,-0.0935153077862871,
1.55552074226154));
#29992=CARTESIAN_POINT('Ctrl Pts',(0.15663688952593,-0.0662798273674848,
1.55772984028737));
#29993=CARTESIAN_POINT('Ctrl Pts',(0.166218204462953,-0.0330583805181475,
1.5599389383132));
#29994=CARTESIAN_POINT('Ctrl Pts',(0.166368100504911,8.32215516180223E-5,
1.56214803633902));
#29995=CARTESIAN_POINT('Ctrl Pts',(0.166721717270512,0.00013247748987999,
1.54285196366098));
#29996=CARTESIAN_POINT('Ctrl Pts',(0.16631788138976,-0.0463324921623522,
1.53973800169035));
#29997=CARTESIAN_POINT('Ctrl Pts',(0.146036306492028,-0.0931065396480778,
1.53662403971971));
#29998=CARTESIAN_POINT('Ctrl Pts',(0.111564911721182,-0.124096839839778,
1.53351007774908));
#29999=CARTESIAN_POINT('Ctrl Pts',(0.0705552254983152,-0.160965161973612,
1.52980548139681));
#30000=CARTESIAN_POINT('Ctrl Pts',(0.00946237858443097,-0.175494403270137,
1.52610088504454));
#30001=CARTESIAN_POINT('Ctrl Pts',(-0.043754143626611,-0.161035180693733,
1.52239628869227));
#30002=CARTESIAN_POINT('Ctrl Pts',(-0.0969706658376549,-0.146575958117328,
1.51869169234));
#30003=CARTESIAN_POINT('Ctrl Pts',(-0.142310863345855,-0.103128271667992,
1.51498709598774));
#30004=CARTESIAN_POINT('Ctrl Pts',(-0.159024536403123,-0.0505761979513979,
1.51128249963547));
#30005=CARTESIAN_POINT('Ctrl Pts',(-0.175738209460389,0.00197587576519482,
1.5075779032832));
#30006=CARTESIAN_POINT('Ctrl Pts',(-0.163825358066725,0.0636323367490458,
1.50387330693093));
#30007=CARTESIAN_POINT('Ctrl Pts',(-0.128737966872089,0.106175754206211,
1.50016871057866));
#30008=CARTESIAN_POINT('Ctrl Pts',(-0.0936505756774527,0.148719171663375,
1.4964641142264));
#30009=CARTESIAN_POINT('Ctrl Pts',(-0.035388644681846,0.172149545593854,
1.49275951787413));
#30010=CARTESIAN_POINT('Ctrl Pts',(0.0193839233712769,0.165743833453852,
1.48905492152186));
#30011=CARTESIAN_POINT('Ctrl Pts',(0.0741564914244009,0.159338121313851,
1.48535032516959));
#30012=CARTESIAN_POINT('Ctrl Pts',(0.125439696535041,0.123096323103367,
1.48164572881732));
#30013=CARTESIAN_POINT('Ctrl Pts',(0.149763488908927,0.07360470278495,1.47794113246505));
#30014=CARTESIAN_POINT('Ctrl Pts',(0.160901714109468,0.0509417559807338,
1.4762447428637));
#30015=CARTESIAN_POINT('Ctrl Pts',(0.166386928169176,0.0255005071147636,
1.47454835326234));
#30016=CARTESIAN_POINT('Ctrl Pts',(0.166334949033457,3.80241454671915E-5,
1.47285196366098));
#30017=CARTESIAN_POINT('Origin',(0.,0.,1.3));
#30018=CARTESIAN_POINT('',(0.166582270817784,-0.000152340582006284,1.40285196366098));
#30019=CARTESIAN_POINT('',(0.166873478424592,6.71112968702338E-7,1.42214803633902));
#30020=CARTESIAN_POINT('',(0.1666,2.04026156737949E-17,1.3));
#30021=CARTESIAN_POINT('Ctrl Pts',(0.166873476951752,6.71109354370205E-7,
1.42214803633902));
#30022=CARTESIAN_POINT('Ctrl Pts',(0.166876772816304,0.0551824619258391,
1.42585504510491));
#30023=CARTESIAN_POINT('Ctrl Pts',(0.136792549878611,0.110361163623334,
1.42956205387081));
#30024=CARTESIAN_POINT('Ctrl Pts',(0.0904117910907898,0.140258570073462,
1.4332690626367));
#30025=CARTESIAN_POINT('Ctrl Pts',(0.0440612155535343,0.170136520159922,
1.43697365898897));
#30026=CARTESIAN_POINT('Ctrl Pts',(-0.0185646804667758,0.174766068965047,
1.44067825534124));
#30027=CARTESIAN_POINT('Ctrl Pts',(-0.0688048006597445,0.152028477144375,
1.4443828516935));
#30028=CARTESIAN_POINT('Ctrl Pts',(-0.119044920852713,0.129290885323702,
1.44808744804577));
#30029=CARTESIAN_POINT('Ctrl Pts',(-0.15689926521834,0.0791861528772324,
1.45179204439804));
#30030=CARTESIAN_POINT('Ctrl Pts',(-0.165043578186289,0.0246449948801753,
1.45549664075031));
#30031=CARTESIAN_POINT('Ctrl Pts',(-0.173187891154238,-0.0298961631168814,
1.45920123710258));
#30032=CARTESIAN_POINT('Ctrl Pts',(-0.15162217272451,-0.088873746664526,
1.46290583345484));
#30033=CARTESIAN_POINT('Ctrl Pts',(-0.110216096648825,-0.125296330528958,
1.46661042980711));
#30034=CARTESIAN_POINT('Ctrl Pts',(-0.0688100205731403,-0.16171891439339,
1.47031502615938));
#30035=CARTESIAN_POINT('Ctrl Pts',(-0.00756358685149875,-0.17558649857461,
1.47401962251165));
#30036=CARTESIAN_POINT('Ctrl Pts',(0.0454934276490607,-0.160552503958399,
1.47772421886392));
#30037=CARTESIAN_POINT('Ctrl Pts',(0.0985504421496201,-0.145518509342189,
1.48142881521618));
#30038=CARTESIAN_POINT('Ctrl Pts',(0.143418037429097,-0.101582935928549,
1.48513341156845));
#30039=CARTESIAN_POINT('Ctrl Pts',(0.159562302527567,-0.0488531491308943,
1.48883800792072));
#30040=CARTESIAN_POINT('Ctrl Pts',(0.164370561528649,-0.0331485958143723,
1.48994135072682));
#30041=CARTESIAN_POINT('Ctrl Pts',(0.166630970058396,-0.0166639678834416,
1.49104469353292));
#30042=CARTESIAN_POINT('Ctrl Pts',(0.166495616539739,-0.000143126867227327,
1.49214803633902));
#30043=CARTESIAN_POINT('Ctrl Pts',(0.166334949033457,3.80241454671915E-5,
1.47285196366098));
#30044=CARTESIAN_POINT('Ctrl Pts',(0.166273415497072,-0.0301047745093415,
1.47084375691007));
#30045=CARTESIAN_POINT('Ctrl Pts',(0.158451996361882,-0.0602773308783548,
1.46883555015916));
#30046=CARTESIAN_POINT('Ctrl Pts',(0.143062834518306,-0.085905647341766,
1.46682734340825));
#30047=CARTESIAN_POINT('Ctrl Pts',(0.114674008116665,-0.133182934723717,
1.46312274705598));
#30048=CARTESIAN_POINT('Ctrl Pts',(0.060531975676251,-0.16499606706127,
1.45941815070371));
#30049=CARTESIAN_POINT('Ctrl Pts',(0.00541514530056254,-0.166785584082033,
1.45571355435145));
#30050=CARTESIAN_POINT('Ctrl Pts',(-0.0497016850751255,-0.168575101102797,
1.45200895799918));
#30051=CARTESIAN_POINT('Ctrl Pts',(-0.105793313386088,-0.14034100280677,
1.44830436164691));
#30052=CARTESIAN_POINT('Ctrl Pts',(-0.137189087849022,-0.0950047843070436,
1.44459976529464));
#30053=CARTESIAN_POINT('Ctrl Pts',(-0.168584862311956,-0.0496685658073169,
1.44089516894238));
#30054=CARTESIAN_POINT('Ctrl Pts',(-0.175284782926862,0.0127697728961095,
1.43719057259011));
#30055=CARTESIAN_POINT('Ctrl Pts',(-0.154222593046579,0.0637349720094271,
1.43348597623784));
#30056=CARTESIAN_POINT('Ctrl Pts',(-0.133160403166296,0.114700171122744,
1.42978137988557));
#30057=CARTESIAN_POINT('Ctrl Pts',(-0.0843361027908238,0.154192230645953,
1.4260767835333));
#30058=CARTESIAN_POINT('Ctrl Pts',(-0.0300944098326194,0.16413738562223,
1.42237218718103));
#30059=CARTESIAN_POINT('Ctrl Pts',(0.0241472831255854,0.174082540598506,
1.41866759082877));
#30060=CARTESIAN_POINT('Ctrl Pts',(0.0838063686665219,0.154480791027852,
1.4149629944765));
#30061=CARTESIAN_POINT('Ctrl Pts',(0.121579527998707,0.114302988740736,
1.41125839812423));
#30062=CARTESIAN_POINT('Ctrl Pts',(0.150151024791829,0.0839126277146479,
1.40845625330315));
#30063=CARTESIAN_POINT('Ctrl Pts',(0.166200792747313,0.0417499637845381,
1.40565410848206));
#30064=CARTESIAN_POINT('Ctrl Pts',(0.166582270817784,-0.000152340582006284,
1.40285196366098));
#30065=CARTESIAN_POINT('Origin',(0.,0.,1.3));
#30066=CARTESIAN_POINT('',(0.16685129292948,5.5034311338048E-5,1.33285196366098));
#30067=CARTESIAN_POINT('',(0.166493658714001,0.000142704933107348,1.35214803633902));
#30068=CARTESIAN_POINT('',(0.1666,2.04026156737949E-17,1.3));
#30069=CARTESIAN_POINT('Ctrl Pts',(0.166493658714001,0.000142704933107348,
1.35214803633902));
#30070=CARTESIAN_POINT('Ctrl Pts',(0.166629086818581,0.0167362841743647,
1.35325620397237));
#30071=CARTESIAN_POINT('Ctrl Pts',(0.164348470273229,0.0332934752509887,
1.35436437160572));
#30072=CARTESIAN_POINT('Ctrl Pts',(0.159498696116421,0.0490604157264683,
1.35547253923907));
#30073=CARTESIAN_POINT('Ctrl Pts',(0.143285936322738,0.101769183257714,
1.35917713559134));
#30074=CARTESIAN_POINT('Ctrl Pts',(0.0983612975566499,0.145646425810988,
1.36288173194361));
#30075=CARTESIAN_POINT('Ctrl Pts',(0.0452847954907157,0.16061147453177,
1.36658632829587));
#30076=CARTESIAN_POINT('Ctrl Pts',(-0.00779170657521921,0.175576523252552,
1.37029092464814));
#30077=CARTESIAN_POINT('Ctrl Pts',(-0.0690200719410003,0.161629378140841,
1.37399552100041));
#30078=CARTESIAN_POINT('Ctrl Pts',(-0.11037879201089,0.125153029241032,
1.37770011735268));
#30079=CARTESIAN_POINT('Ctrl Pts',(-0.151737512080778,0.0886766803412233,
1.38140471370495));
#30080=CARTESIAN_POINT('Ctrl Pts',(-0.173226586854776,0.0296711276533176,
1.38510931005721));
#30081=CARTESIAN_POINT('Ctrl Pts',(-0.165011419406707,-0.0248594030476235,
1.38881390640948));
#30082=CARTESIAN_POINT('Ctrl Pts',(-0.156796251958638,-0.0793899337485655,
1.39251850276175));
#30083=CARTESIAN_POINT('Ctrl Pts',(-0.1188768422885,-0.129445442462543,
1.39622309911402));
#30084=CARTESIAN_POINT('Ctrl Pts',(-0.0686072232581569,-0.152117741798697,
1.39992769546629));
#30085=CARTESIAN_POINT('Ctrl Pts',(-0.0183376042278136,-0.174790041134852,
1.40363229181856));
#30086=CARTESIAN_POINT('Ctrl Pts',(0.0442822241627354,-0.170079131093183,
1.40733688817082));
#30087=CARTESIAN_POINT('Ctrl Pts',(0.0905939423885369,-0.140140986355195,
1.41104148452309));
#30088=CARTESIAN_POINT('Ctrl Pts',(0.136875502667449,-0.110222337179314,
1.41474366846173));
#30089=CARTESIAN_POINT('Ctrl Pts',(0.166870185376906,-0.0551092982940088,
1.41844585240038));
#30090=CARTESIAN_POINT('Ctrl Pts',(0.166873476951752,6.71109354370205E-7,
1.42214803633902));
#30091=CARTESIAN_POINT('Ctrl Pts',(0.166582270817784,-0.000152340582006284,
1.40285196366098));
#30092=CARTESIAN_POINT('Ctrl Pts',(0.166705128660898,-0.0136472886129686,
1.4019495121298));
#30093=CARTESIAN_POINT('Ctrl Pts',(0.165202856095667,-0.0271152318944043,
1.40104706059861));
#30094=CARTESIAN_POINT('Ctrl Pts',(0.161970345045233,-0.0401542300245841,
1.40014460906743));
#30095=CARTESIAN_POINT('Ctrl Pts',(0.148700769636142,-0.0936797914992128,
1.39644001271516));
#30096=CARTESIAN_POINT('Ctrl Pts',(0.106274385694529,-0.139977059444894,
1.39273541636289));
#30097=CARTESIAN_POINT('Ctrl Pts',(0.054107868404235,-0.157857826665655,
1.38903082001062));
#30098=CARTESIAN_POINT('Ctrl Pts',(0.00194135111394122,-0.175738593886417,
1.38532622365835));
#30099=CARTESIAN_POINT('Ctrl Pts',(-0.0599652995250327,-0.165202860382259,
1.38162162730609));
#30100=CARTESIAN_POINT('Ctrl Pts',(-0.103280153812656,-0.131072364331603,
1.37791703095382));
#30101=CARTESIAN_POINT('Ctrl Pts',(-0.146595008100279,-0.0969418682809483,
1.37421243460155));
#30102=CARTESIAN_POINT('Ctrl Pts',(-0.171318066036552,-0.0392166096837955,
1.37050783824928));
#30103=CARTESIAN_POINT('Ctrl Pts',(-0.166134679967937,0.0156851195376423,
1.36680324189701));
#30104=CARTESIAN_POINT('Ctrl Pts',(-0.160951293899322,0.0705868487590808,
1.36309864554474));
#30105=CARTESIAN_POINT('Ctrl Pts',(-0.12586146382582,0.122665048604804,
1.35939404919248));
#30106=CARTESIAN_POINT('Ctrl Pts',(-0.0769242494532953,0.14808583561233,
1.35568945284021));
#30107=CARTESIAN_POINT('Ctrl Pts',(-0.0279870350807717,0.173506622619856,
1.35198485648794));
#30108=CARTESIAN_POINT('Ctrl Pts',(0.0347975635907744,0.172269996789183,
1.34828026013567));
#30109=CARTESIAN_POINT('Ctrl Pts',(0.0826958189663461,0.144941906943662,
1.3445756637834));
#30110=CARTESIAN_POINT('Ctrl Pts',(0.130594074341918,0.117613817098141,
1.34087106743114));
#30111=CARTESIAN_POINT('Ctrl Pts',(0.163605986421516,0.0641942632377707,
1.33716647107887));
#30112=CARTESIAN_POINT('Ctrl Pts',(0.166623466451679,0.00913100709632859,
1.3334618747266));
#30113=CARTESIAN_POINT('Ctrl Pts',(0.166789062042101,0.00610920336601207,
1.33325857103806));
#30114=CARTESIAN_POINT('Ctrl Pts',(0.16686432402183,0.00308244933152886,
1.33305526734952));
#30115=CARTESIAN_POINT('Ctrl Pts',(0.16685129292948,5.5034311338048E-5,
1.33285196366098));
#30116=CARTESIAN_POINT('Origin',(0.,0.,1.3));
#30117=CARTESIAN_POINT('',(0.166419792426106,0.000117644517947116,1.26285196366098));
#30118=CARTESIAN_POINT('',(0.166369239667266,-8.42498788368234E-5,1.28214803633902));
#30119=CARTESIAN_POINT('',(0.1666,2.04026156737949E-17,1.3));
#30120=CARTESIAN_POINT('Ctrl Pts',(0.166369239667266,-8.42498788368234E-5,
1.28214803633902));
#30121=CARTESIAN_POINT('Ctrl Pts',(0.166217137033255,0.0331292003521081,
1.2843619591921));
#30122=CARTESIAN_POINT('Ctrl Pts',(0.156590960021794,0.0664238537129591,
1.28657588204517));
#30123=CARTESIAN_POINT('Ctrl Pts',(0.138087078302622,0.093694809140457,
1.28878980489824));
#30124=CARTESIAN_POINT('Ctrl Pts',(0.107124205036991,0.139327782240334,
1.29249440125051));
#30125=CARTESIAN_POINT('Ctrl Pts',(0.051303827751912,0.168094448054701,
1.29619899760278));
#30126=CARTESIAN_POINT('Ctrl Pts',(-0.00382754136500674,0.166829578855541,
1.29990359395505));
#30127=CARTESIAN_POINT('Ctrl Pts',(-0.0589589104819255,0.16556470965638,
1.30360819030732));
#30128=CARTESIAN_POINT('Ctrl Pts',(-0.113401271430684,0.134268305443692,
1.30731278665959));
#30129=CARTESIAN_POINT('Ctrl Pts',(-0.142238769013948,0.0872633430680612,
1.31101738301185));
#30130=CARTESIAN_POINT('Ctrl Pts',(-0.171076266597211,0.0402583806924305,
1.31472197936412));
#30131=CARTESIAN_POINT('Ctrl Pts',(-0.17430890081498,-0.0224551398461431,
1.31842657571639));
#30132=CARTESIAN_POINT('Ctrl Pts',(-0.150457238287118,-0.0721760202632685,
1.32213117206866));
#30133=CARTESIAN_POINT('Ctrl Pts',(-0.126605575759256,-0.121896900680394,
1.32583576842093));
#30134=CARTESIAN_POINT('Ctrl Pts',(-0.0756696164857624,-0.158625140976071,
1.32954036477319));
#30135=CARTESIAN_POINT('Ctrl Pts',(-0.0209604910548609,-0.165551853715821,
1.33324496112546));
#30136=CARTESIAN_POINT('Ctrl Pts',(0.0337486343760406,-0.17247856645557,
1.33694955747773));
#30137=CARTESIAN_POINT('Ctrl Pts',(0.0922309259643503,-0.149603751639392,
1.34065415383));
#30138=CARTESIAN_POINT('Ctrl Pts',(0.127721631347866,-0.107396197976694,
1.34435875018227));
#30139=CARTESIAN_POINT('Ctrl Pts',(0.152595889688052,-0.0778143234445287,
1.34695517890118));
#30140=CARTESIAN_POINT('Ctrl Pts',(0.166176351648266,-0.038735930748939,
1.3495516076201));
#30141=CARTESIAN_POINT('Ctrl Pts',(0.166493658714001,0.000142704933107348,
1.35214803633902));
#30142=CARTESIAN_POINT('Ctrl Pts',(0.16685129292948,5.5034311338048E-5,
1.33285196366098));
#30143=CARTESIAN_POINT('Ctrl Pts',(0.16662687167882,-0.0520830556384961,
1.32935067099725));
#30144=CARTESIAN_POINT('Ctrl Pts',(0.140215016815216,-0.104417191766459,
1.32584937833352));
#30145=CARTESIAN_POINT('Ctrl Pts',(0.0980387654551791,-0.135037607098881,
1.3223480856698));
#30146=CARTESIAN_POINT('Ctrl Pts',(0.0534135364477915,-0.167436006730135,
1.31864348931753));
#30147=CARTESIAN_POINT('Ctrl Pts',(-0.00885996954770948,-0.175525847570128,
1.31493889296526));
#30148=CARTESIAN_POINT('Ctrl Pts',(-0.0602819293976768,-0.155604768085892,
1.31123429661299));
#30149=CARTESIAN_POINT('Ctrl Pts',(-0.111703889247644,-0.135683688601655,
1.30752970026073));
#30150=CARTESIAN_POINT('Ctrl Pts',(-0.152274302952078,-0.0877516887931891,
1.30382510390846));
#30151=CARTESIAN_POINT('Ctrl Pts',(-0.163425890629257,-0.0337451201657775,
1.30012050755619));
#30152=CARTESIAN_POINT('Ctrl Pts',(-0.174577478306436,0.0202614484616345,
1.29641591120392));
#30153=CARTESIAN_POINT('Ctrl Pts',(-0.15631023995636,0.0803425859079921,
1.29271131485165));
#30154=CARTESIAN_POINT('Ctrl Pts',(-0.116984280792225,0.119001818937757,
1.28900671849938));
#30155=CARTESIAN_POINT('Ctrl Pts',(-0.077658321628091,0.157661051967521,
1.28530212214712));
#30156=CARTESIAN_POINT('Ctrl Pts',(-0.0172736416498982,0.174898380580693,
1.28159752579485));
#30157=CARTESIAN_POINT('Ctrl Pts',(0.0365343679459083,0.162825043595149,
1.27789292944258));
#30158=CARTESIAN_POINT('Ctrl Pts',(0.090342377541716,0.150751706609605,
1.27418833309031));
#30159=CARTESIAN_POINT('Ctrl Pts',(0.137573716755137,0.109367704025345,
1.27048373673804));
#30160=CARTESIAN_POINT('Ctrl Pts',(0.15661269537524,0.0576126592883118,
1.26677914038578));
#30161=CARTESIAN_POINT('Ctrl Pts',(0.163340322948393,0.0393244583837232,
1.26547008147751));
#30162=CARTESIAN_POINT('Ctrl Pts',(0.166547744893355,0.0197412896159237,
1.26416102256925));
#30163=CARTESIAN_POINT('Ctrl Pts',(0.166419792426106,0.000117644517947116,
1.26285196366098));
#30164=CARTESIAN_POINT('Origin',(0.,0.,1.3));
#30165=CARTESIAN_POINT('',(0.166426142970557,-0.000120642765556289,1.19285196366098));
#30166=CARTESIAN_POINT('',(0.16680112293357,-9.74720745467285E-5,1.21214803633902));
#30167=CARTESIAN_POINT('',(0.1666,2.04026156737949E-17,1.3));
#30168=CARTESIAN_POINT('Ctrl Pts',(0.16680112293357,-9.74720745467285E-5,
1.21214803633902));
#30169=CARTESIAN_POINT('Ctrl Pts',(0.166457232615762,0.0493755335317627,
1.21546771441182));
#30170=CARTESIAN_POINT('Ctrl Pts',(0.143044424972525,0.0991312161213854,
1.21878739248462));
#30171=CARTESIAN_POINT('Ctrl Pts',(0.104522946124804,0.130083481608585,
1.22210707055742));
#30172=CARTESIAN_POINT('Ctrl Pts',(0.0615348831579396,0.164624677261814,
1.22581166690969));
#30173=CARTESIAN_POINT('Ctrl Pts',(-0.000268695245690821,0.175749122363903,
1.22951626326196));
#30174=CARTESIAN_POINT('Ctrl Pts',(-0.0526030309795398,0.15836565153399,
1.23322085961422));
#30175=CARTESIAN_POINT('Ctrl Pts',(-0.104937366713389,0.140982180704076,
1.23692545596649));
#30176=CARTESIAN_POINT('Ctrl Pts',(-0.147802459777456,0.0950907939421611,
1.24063005231876));
#30177=CARTESIAN_POINT('Ctrl Pts',(-0.161580857269364,0.0416939446216941,
1.24433464867103));
#30178=CARTESIAN_POINT('Ctrl Pts',(-0.175359254761272,-0.0117029046987729,
1.2480392450233));
#30179=CARTESIAN_POINT('Ctrl Pts',(-0.16005095668102,-0.0726052165777916,
1.25174384137556));
#30180=CARTESIAN_POINT('Ctrl Pts',(-0.122661892448987,-0.113140702644331,
1.25544843772783));
#30181=CARTESIAN_POINT('Ctrl Pts',(-0.0852728282169544,-0.15367618871087,
1.2591530340801));
#30182=CARTESIAN_POINT('Ctrl Pts',(-0.0258029978331414,-0.17384484896493,
1.26285763043237));
#30183=CARTESIAN_POINT('Ctrl Pts',(0.0285308936104228,-0.164416381677161,
1.26656222678464));
#30184=CARTESIAN_POINT('Ctrl Pts',(0.0828647850539866,-0.154987914389393,
1.2702668231369));
#30185=CARTESIAN_POINT('Ctrl Pts',(0.132062737557302,-0.115962319559795,
1.27397141948917));
#30186=CARTESIAN_POINT('Ctrl Pts',(0.153609029185868,-0.0651998819523026,
1.27767601584144));
#30187=CARTESIAN_POINT('Ctrl Pts',(0.162278930811433,-0.044773845401895,
1.27916668934063));
#30188=CARTESIAN_POINT('Ctrl Pts',(0.166471653066795,-0.022447454634266,
1.28065736283983));
#30189=CARTESIAN_POINT('Ctrl Pts',(0.166369239667266,-8.42498788368234E-5,
1.28214803633902));
#30190=CARTESIAN_POINT('Ctrl Pts',(0.166419792426106,0.000117644517947116,
1.26285196366098));
#30191=CARTESIAN_POINT('Ctrl Pts',(0.166185643355799,-0.0357930210168177,
1.26045642621698));
#30192=CARTESIAN_POINT('Ctrl Pts',(0.154782035268061,-0.0718392331665093,
1.25806088877297));
#30193=CARTESIAN_POINT('Ctrl Pts',(0.133341646618848,-0.100333245437109,
1.25566535132897));
#30194=CARTESIAN_POINT('Ctrl Pts',(0.100185001215565,-0.144398018535696,
1.2519607549767));
#30195=CARTESIAN_POINT('Ctrl Pts',(0.0430250923822119,-0.170401477843065,
1.24825615862443));
#30196=CARTESIAN_POINT('Ctrl Pts',(-0.0119785234848996,-0.166442992757554,
1.24455156227217));
#30197=CARTESIAN_POINT('Ctrl Pts',(-0.0669821393520106,-0.162484507672042,
1.2408469659199));
#30198=CARTESIAN_POINT('Ctrl Pts',(-0.11982946225288,-0.12856407819365,
1.23714236956763));
#30199=CARTESIAN_POINT('Ctrl Pts',(-0.146334615197223,-0.0802055812150856,
1.23343777321536));
#30200=CARTESIAN_POINT('Ctrl Pts',(-0.172839768141565,-0.0318470842365214,
1.22973317686309));
#30201=CARTESIAN_POINT('Ctrl Pts',(-0.17300275112938,0.0309494802422141,
1.22602858051083));
#30202=CARTESIAN_POINT('Ctrl Pts',(-0.14674897407212,0.0794449084066994,
1.22232398415856));
#30203=CARTESIAN_POINT('Ctrl Pts',(-0.12049519701486,0.127940336571185,
1.21861938780629));
#30204=CARTESIAN_POINT('Ctrl Pts',(-0.0678246599125219,0.162134628421419,
1.21491479145402));
#30205=CARTESIAN_POINT('Ctrl Pts',(-0.01284233273225,0.166378572397304,
1.21121019510176));
#30206=CARTESIAN_POINT('Ctrl Pts',(0.0421399944480223,0.170622516373188,
1.20750559874949));
#30207=CARTESIAN_POINT('Ctrl Pts',(0.0994341117062293,0.144916112474723,
1.20380100239722));
#30208=CARTESIAN_POINT('Ctrl Pts',(0.132819041399409,0.101024042211295,
1.20009640604495));
#30209=CARTESIAN_POINT('Ctrl Pts',(0.154580764464244,0.0724133161563545,
1.19768159191696));
#30210=CARTESIAN_POINT('Ctrl Pts',(0.166183499569454,0.0360755201147432,
1.19526677778897));
#30211=CARTESIAN_POINT('Ctrl Pts',(0.166426142970557,-0.000120642765556289,
1.19285196366098));
#30212=CARTESIAN_POINT('Origin',(0.,0.,1.3));
#30213=CARTESIAN_POINT('',(0.166855124306607,-5.00565220619177E-5,1.12285196366098));
#30214=CARTESIAN_POINT('',(0.166664543572935,0.000145872469707454,1.14214803633902));
#30215=CARTESIAN_POINT('',(0.1666,2.04026156737949E-17,1.3));
#30216=CARTESIAN_POINT('Ctrl Pts',(0.166664543572935,0.000145872469707454,
1.14214803633902));
#30217=CARTESIAN_POINT('Ctrl Pts',(0.166763206461382,0.0109113832732099,
1.14286887327928));
#30218=CARTESIAN_POINT('Ctrl Pts',(0.165809417829237,0.0216594859626649,
1.14358971021953));
#30219=CARTESIAN_POINT('Ctrl Pts',(0.163739663996808,0.0321882103916611,
1.14431054715979));
#30220=CARTESIAN_POINT('Ctrl Pts',(0.153102580809897,0.0862984701957669,
1.14801514351206));
#30221=CARTESIAN_POINT('Ctrl Pts',(0.112990188231545,0.134614425572516,
1.15171973986433));
#30222=CARTESIAN_POINT('Ctrl Pts',(0.0617601501778567,0.155024005573456,
1.1554243362166));
#30223=CARTESIAN_POINT('Ctrl Pts',(0.010530112124168,0.175433585574396,
1.15912893256886));
#30224=CARTESIAN_POINT('Ctrl Pts',(-0.0518175714048562,0.167936790199525,
1.16283352892113));
#30225=CARTESIAN_POINT('Ctrl Pts',(-0.0967491295066884,0.135964570361971,
1.1665381252734));
#30226=CARTESIAN_POINT('Ctrl Pts',(-0.14168068760852,0.103992350524416,
1.17024272162567));
#30227=CARTESIAN_POINT('Ctrl Pts',(-0.16919612028316,0.0475447062241783,
1.17394731797794));
#30228=CARTESIAN_POINT('Ctrl Pts',(-0.166702833743975,-0.00754477804487655,
1.1776519143302));
#30229=CARTESIAN_POINT('Ctrl Pts',(-0.16420954720479,-0.0626342623139314,
1.18135651068247));
#30230=CARTESIAN_POINT('Ctrl Pts',(-0.131707541451779,-0.116365586551803,
1.18506110703474));
#30231=CARTESIAN_POINT('Ctrl Pts',(-0.0840715437167003,-0.144148305543673,
1.18876570338701));
#30232=CARTESIAN_POINT('Ctrl Pts',(-0.0364355459816213,-0.171931024535542,
1.19247029973928));
#30233=CARTESIAN_POINT('Ctrl Pts',(0.0263344437355261,-0.17376513828141,
1.19617489609154));
#30234=CARTESIAN_POINT('Ctrl Pts',(0.0755113837106313,-0.148811254225361,
1.19987949244381));
#30235=CARTESIAN_POINT('Ctrl Pts',(0.124688323685737,-0.123857370169311,
1.20358408879608));
#30236=CARTESIAN_POINT('Ctrl Pts',(0.1602722139188,-0.0721154883113449,
1.20728868514835));
#30237=CARTESIAN_POINT('Ctrl Pts',(0.165977885270282,-0.0172655742801778,
1.21099328150062));
#30238=CARTESIAN_POINT('Ctrl Pts',(0.166570721031857,-0.011566509515692,
1.21137819978008));
#30239=CARTESIAN_POINT('Ctrl Pts',(0.166840997182384,-0.00583389102255577,
1.21176311805955));
#30240=CARTESIAN_POINT('Ctrl Pts',(0.16680112293357,-9.74720745467285E-5,
1.21214803633902));
#30241=CARTESIAN_POINT('Ctrl Pts',(0.166426142970557,-0.000120642765556289,
1.19285196366098));
#30242=CARTESIAN_POINT('Ctrl Pts',(0.166555741825373,-0.0194534630140944,
1.1915621814367));
#30243=CARTESIAN_POINT('Ctrl Pts',(0.163444578249431,-0.0387458787095636,
1.19027239921243));
#30244=CARTESIAN_POINT('Ctrl Pts',(0.156909640667809,-0.0567989395012422,
1.18898261698815));
#30245=CARTESIAN_POINT('Ctrl Pts',(0.138139568114877,-0.108652114321963,
1.18527802063588));
#30246=CARTESIAN_POINT('Ctrl Pts',(0.0911236808808596,-0.150280727335013,
1.18157342428361));
#30247=CARTESIAN_POINT('Ctrl Pts',(0.0373790663566119,-0.162633207744568,
1.17786882793134));
#30248=CARTESIAN_POINT('Ctrl Pts',(-0.0163655481676351,-0.174985688154123,
1.17416423157907));
#30249=CARTESIAN_POINT('Ctrl Pts',(-0.0768388899821125,-0.158062035960183,
1.17045963522681));
#30250=CARTESIAN_POINT('Ctrl Pts',(-0.116364991298242,-0.119607456553155,
1.16675503887454));
#30251=CARTESIAN_POINT('Ctrl Pts',(-0.155891092614372,-0.0811528771461272,
1.16305044252227));
#30252=CARTESIAN_POINT('Ctrl Pts',(-0.174469953432153,-0.0211673705260111,
1.15934584617));
#30253=CARTESIAN_POINT('Ctrl Pts',(-0.163598852749046,0.0328963560619538,
1.15564124981773));
#30254=CARTESIAN_POINT('Ctrl Pts',(-0.152727752065939,0.0869600826499182,
1.15193665346547));
#30255=CARTESIAN_POINT('Ctrl Pts',(-0.112406689881943,0.135102029205731,
1.1482320571132));
#30256=CARTESIAN_POINT('Ctrl Pts',(-0.061088828941493,0.155289760903929,
1.14452746076093));
#30257=CARTESIAN_POINT('Ctrl Pts',(-0.00977096800104246,0.175477492602127,
1.14082286440866));
#30258=CARTESIAN_POINT('Ctrl Pts',(0.0525436916958626,0.16771100944271,
1.13711826805639));
#30259=CARTESIAN_POINT('Ctrl Pts',(0.0973364927906947,0.135544686484056,
1.13341367170413));
#30260=CARTESIAN_POINT('Ctrl Pts',(0.139904197214479,0.10497623587064,1.12989310235641));
#30261=CARTESIAN_POINT('Ctrl Pts',(0.166647613265987,0.0523718751412305,
1.12637253300869));
#30262=CARTESIAN_POINT('Ctrl Pts',(0.166855124306607,-5.00565220619177E-5,
1.12285196366098));
#30263=CARTESIAN_POINT('Origin',(0.,0.,1.3));
#30264=CARTESIAN_POINT('',(0.166573628657937,0.000152187718365226,1.05285196366098));
#30265=CARTESIAN_POINT('',(0.166327182499917,6.33242585386815E-6,1.07214803633902));
#30266=CARTESIAN_POINT('',(0.1666,2.04026156737949E-17,1.3));
#30267=CARTESIAN_POINT('Ctrl Pts',(0.166327182499917,6.33242585386815E-6,
1.07214803633902));
#30268=CARTESIAN_POINT('Ctrl Pts',(0.166336479007403,0.0274263312352492,
1.073974628499));
#30269=CARTESIAN_POINT('Ctrl Pts',(0.159932481000657,0.0548422420648042,
1.07580122065898));
#30270=CARTESIAN_POINT('Ctrl Pts',(0.147091342637332,0.0788092340673142,
1.07762781281897));
#30271=CARTESIAN_POINT('Ctrl Pts',(0.121047633821556,0.127417803124253,
1.08133240917123));
#30272=CARTESIAN_POINT('Ctrl Pts',(0.0685255340861956,0.161839665678967,
1.0850370055235));
#30273=CARTESIAN_POINT('Ctrl Pts',(0.0135620801901698,0.166321461139012,
1.08874160187577));
#30274=CARTESIAN_POINT('Ctrl Pts',(-0.0414013737058552,0.170803256599056,
1.09244619822804));
#30275=CARTESIAN_POINT('Ctrl Pts',(-0.0988061817625453,0.145344984964431,
1.09615079458031));
#30276=CARTESIAN_POINT('Ctrl Pts',(-0.132380708062468,0.101597768611665,
1.09985539093257));
#30277=CARTESIAN_POINT('Ctrl Pts',(-0.165955234362392,0.0578505522588977,
1.10355998728484));
#30278=CARTESIAN_POINT('Ctrl Pts',(-0.175699478905547,-0.00418560881201081,
1.10726458363711));
#30279=CARTESIAN_POINT('Ctrl Pts',(-0.157153932924644,-0.0561195137204682,
1.11096917998938));
#30280=CARTESIAN_POINT('Ctrl Pts',(-0.13860838694374,-0.108053418628926,
1.11467377634165));
#30281=CARTESIAN_POINT('Ctrl Pts',(-0.0917730504387764,-0.149885067374932,
1.11837837269391));
#30282=CARTESIAN_POINT('Ctrl Pts',(-0.0380823807348833,-0.162469968707007,
1.12208296904618));
#30283=CARTESIAN_POINT('Ctrl Pts',(0.0156082889690095,-0.175054870039082,
1.12578756539845));
#30284=CARTESIAN_POINT('Ctrl Pts',(0.076154291871832,-0.158393023957226,
1.12949216175072));
#30285=CARTESIAN_POINT('Ctrl Pts',(0.115846406425509,-0.120109818800568,
1.13319675810299));
#30286=CARTESIAN_POINT('Ctrl Pts',(0.147815265950422,-0.0892757243821015,
1.136180517515));
#30287=CARTESIAN_POINT('Ctrl Pts',(0.16625614840673,-0.044415792438328,
1.13916427692701));
#30288=CARTESIAN_POINT('Ctrl Pts',(0.166664543572935,0.000145872469707454,
1.14214803633902));
#30289=CARTESIAN_POINT('Ctrl Pts',(0.166855124306607,-5.00565220619177E-5,
1.12285196366098));
#30290=CARTESIAN_POINT('Ctrl Pts',(0.166865971312146,-0.00279025280966625,
1.12266793665643));
#30291=CARTESIAN_POINT('Ctrl Pts',(0.166804312774377,-0.00552995063608946,
1.12248390965187));
#30292=CARTESIAN_POINT('Ctrl Pts',(0.166668618800564,-0.00826597665440976,
1.12229988264732));
#30293=CARTESIAN_POINT('Ctrl Pts',(0.163937001222843,-0.0633441540763332,
1.11859528629505));
#30294=CARTESIAN_POINT('Ctrl Pts',(0.131202823574641,-0.116934346162291,
1.11489068994278));
#30295=CARTESIAN_POINT('Ctrl Pts',(0.0834470678717536,-0.144510697621526,
1.11118609359052));
#30296=CARTESIAN_POINT('Ctrl Pts',(0.035691312168866,-0.172087049080761,
1.10748149723825));
#30297=CARTESIAN_POINT('Ctrl Pts',(-0.0270860215887074,-0.173649559913274,
1.10377690088598));
#30298=CARTESIAN_POINT('Ctrl Pts',(-0.0761545306345133,-0.148483138187173,
1.10007230453371));
#30299=CARTESIAN_POINT('Ctrl Pts',(-0.125223039680319,-0.123316716461072,
1.09636770818145));
#30300=CARTESIAN_POINT('Ctrl Pts',(-0.160582724014357,-0.0714213621763564,
1.09266311182918));
#30301=CARTESIAN_POINT('Ctrl Pts',(-0.166051023599269,-0.0165472784677163,
1.08895851547691));
#30302=CARTESIAN_POINT('Ctrl Pts',(-0.171519323184182,0.0383268052409238,
1.08525391912464));
#30303=CARTESIAN_POINT('Ctrl Pts',(-0.147096238019968,0.0961796183734885,
1.08154932277237));
#30304=CARTESIAN_POINT('Ctrl Pts',(-0.103959131518119,0.130534492913072,
1.0778447264201));
#30305=CARTESIAN_POINT('Ctrl Pts',(-0.0608220250162706,0.164889367452656,
1.07414013006784));
#30306=CARTESIAN_POINT('Ctrl Pts',(0.0010291028232132,0.175746303399259,
1.07043553371557));
#30307=CARTESIAN_POINT('Ctrl Pts',(0.0532877326205867,0.15813656252862,
1.0667309373633));
#30308=CARTESIAN_POINT('Ctrl Pts',(0.10554636241796,0.140526821657981,1.06302634101103));
#30309=CARTESIAN_POINT('Ctrl Pts',(0.148212494173223,0.0944504039700999,
1.05932174465876));
#30310=CARTESIAN_POINT('Ctrl Pts',(0.161759730763308,0.0409944431478461,
1.0556171483065));
#30311=CARTESIAN_POINT('Ctrl Pts',(0.165130373342236,0.0276942445097812,
1.05469542009132));
#30312=CARTESIAN_POINT('Ctrl Pts',(0.16669841799434,0.0139372170985273,
1.05377369187615));
#30313=CARTESIAN_POINT('Ctrl Pts',(0.166573628657937,0.000152187718365227,
1.05285196366098));
#30314=CARTESIAN_POINT('Origin',(0.,0.,1.3));
#30315=CARTESIAN_POINT('',(0.16633703813182,-4.26131537097363E-5,0.982851963660979));
#30316=CARTESIAN_POINT('',(0.166641299058679,-0.000149160109009599,1.00214803633902));
#30317=CARTESIAN_POINT('',(0.1666,2.04026156737949E-17,1.3));
#30318=CARTESIAN_POINT('Ctrl Pts',(0.166641299058679,-0.000149160109009599,
1.00214803633902));
#30319=CARTESIAN_POINT('Ctrl Pts',(0.166236990763482,0.0436603970157784,
1.00508038371873));
#30320=CARTESIAN_POINT('Ctrl Pts',(0.148493576846311,0.0877597158867868,
1.00801273109843));
#30321=CARTESIAN_POINT('Ctrl Pts',(0.117498076053599,0.118494559065924,
1.01094507847814));
#30322=CARTESIAN_POINT('Ctrl Pts',(0.0783397485075339,0.157323583456734,
1.01464967483041));
#30323=CARTESIAN_POINT('Ctrl Pts',(0.0180302104029479,0.174822017275825,
1.01835427118268));
#30324=CARTESIAN_POINT('Ctrl Pts',(-0.0358295364409326,0.162981602616999,
1.02205886753494));
#30325=CARTESIAN_POINT('Ctrl Pts',(-0.089689283284813,0.151141187958173,
1.02576346388721));
#30326=CARTESIAN_POINT('Ctrl Pts',(-0.137099238867988,0.10996192482143,
1.02946806023948));
#30327=CARTESIAN_POINT('Ctrl Pts',(-0.156361968042692,0.0582897367165174,
1.03317265659175));
#30328=CARTESIAN_POINT('Ctrl Pts',(-0.175624697217396,0.00661754861160513,
1.03687725294402));
#30329=CARTESIAN_POINT('Ctrl Pts',(-0.166740199983629,-0.0555475644614757,
1.04058184929629));
#30330=CARTESIAN_POINT('Ctrl Pts',(-0.133774516953309,-0.0997553861262926,
1.04428644564855));
#30331=CARTESIAN_POINT('Ctrl Pts',(-0.100808833922988,-0.143963207791109,
1.04799104200082));
#30332=CARTESIAN_POINT('Ctrl Pts',(-0.0437619650961137,-0.170213738047662,
1.05169563835309));
#30333=CARTESIAN_POINT('Ctrl Pts',(0.0112582665697782,-0.166493272809894,
1.05540023470536));
#30334=CARTESIAN_POINT('Ctrl Pts',(0.0662784982356701,-0.162772807572126,
1.05910483105763));
#30335=CARTESIAN_POINT('Ctrl Pts',(0.11927209274058,-0.129081346840038,
1.06280942740989));
#30336=CARTESIAN_POINT('Ctrl Pts',(0.145986231044939,-0.0808379786944121,
1.06651402376216));
#30337=CARTESIAN_POINT('Ctrl Pts',(0.159528668319701,-0.0563815362072228,
1.06839202795445));
#30338=CARTESIAN_POINT('Ctrl Pts',(0.166317624329016,-0.0281854412194699,
1.07027003214673));
#30339=CARTESIAN_POINT('Ctrl Pts',(0.166327182499917,6.33242585386815E-6,
1.07214803633902));
#30340=CARTESIAN_POINT('Ctrl Pts',(0.166573628657937,0.000152187718365227,
1.05285196366098));
#30341=CARTESIAN_POINT('Ctrl Pts',(0.166196866546928,-0.0414673682413184,
1.05006909552388));
#30342=CARTESIAN_POINT('Ctrl Pts',(0.150389111841613,-0.0833421755592448,
1.04728622738679));
#30343=CARTESIAN_POINT('Ctrl Pts',(0.122171212866625,-0.113670355101641,
1.04450335924969));
#30344=CARTESIAN_POINT('Ctrl Pts',(0.0846071169549502,-0.154043688572246,
1.04079876289742));
#30345=CARTESIAN_POINT('Ctrl Pts',(0.0250505837066941,-0.173954851556829,
1.03709416654516));
#30346=CARTESIAN_POINT('Ctrl Pts',(-0.0292420016986911,-0.164291387935873,
1.03338957019289));
#30347=CARTESIAN_POINT('Ctrl Pts',(-0.0835345871040766,-0.154627924314917,
1.02968497384062));
#30348=CARTESIAN_POINT('Ctrl Pts',(-0.132563224666591,-0.115389834088422,
1.02598037748835));
#30349=CARTESIAN_POINT('Ctrl Pts',(-0.153889680451665,-0.0645346507397467,
1.02227578113608));
#30350=CARTESIAN_POINT('Ctrl Pts',(-0.175216136236738,-0.0136794673910717,
1.01857118478382));
#30351=CARTESIAN_POINT('Ctrl Pts',(-0.16884041024437,0.0487928090797828,
1.01486658843155));
#30352=CARTESIAN_POINT('Ctrl Pts',(-0.137680389518285,0.0942913851820011,
1.01116199207928));
#30353=CARTESIAN_POINT('Ctrl Pts',(-0.106520368792199,0.139789961284219,
1.00745739572701));
#30354=CARTESIAN_POINT('Ctrl Pts',(-0.0505760533323975,0.168314837017802,
1.00375279937474));
#30355=CARTESIAN_POINT('Ctrl Pts',(0.00454932345543924,0.166811444936069,
1.00004820302248));
#30356=CARTESIAN_POINT('Ctrl Pts',(0.0596747002432758,0.165308052854335,
0.996343606670208));
#30357=CARTESIAN_POINT('Ctrl Pts',(0.113981138359147,0.133776392957287,
0.992639010317939));
#30358=CARTESIAN_POINT('Ctrl Pts',(0.142614988862282,0.0866471011481969,
0.988934413965671));
#30359=CARTESIAN_POINT('Ctrl Pts',(0.158285969463688,0.0608537759501981,
0.986906930530773));
#30360=CARTESIAN_POINT('Ctrl Pts',(0.166267372459907,0.0303885726052033,
0.984879447095876));
#30361=CARTESIAN_POINT('Ctrl Pts',(0.16633703813182,-4.26131537097363E-5,
0.982851963660979));
#30362=CARTESIAN_POINT('Origin',(0.,0.,1.3));
#30363=CARTESIAN_POINT('',(0.166729862742343,-0.000130123946020723,0.912851963660979));
#30364=CARTESIAN_POINT('',(0.16681765906064,8.64047405809373E-5,0.93214803633902));
#30365=CARTESIAN_POINT('',(0.1666,2.04026156737949E-17,1.3));
#30366=CARTESIAN_POINT('Ctrl Pts',(0.16681765906064,8.64047405809373E-5,
0.93214803633902));
#30367=CARTESIAN_POINT('Ctrl Pts',(0.166849023174239,0.00505533653555562,
0.932481542586184));
#30368=CARTESIAN_POINT('Ctrl Pts',(0.166646252238729,0.0100216728157887,
0.932815048833348));
#30369=CARTESIAN_POINT('Ctrl Pts',(0.166201007638075,0.0149661744225974,
0.933148555080512));
#30370=CARTESIAN_POINT('Ctrl Pts',(0.161255218653678,0.0698898310921401,
0.93685315143278));
#30371=CARTESIAN_POINT('Ctrl Pts',(0.126391025843356,0.122119345383236,
0.940557747785048));
#30372=CARTESIAN_POINT('Ctrl Pts',(0.0775642504900456,0.147751626038697,
0.944262344137316));
#30373=CARTESIAN_POINT('Ctrl Pts',(0.0287374751367354,0.173383906694158,
0.947966940489584));
#30374=CARTESIAN_POINT('Ctrl Pts',(-0.0340518827595631,0.172418953713984,
0.951671536841852));
#30375=CARTESIAN_POINT('Ctrl Pts',(-0.0820679309643883,0.145298361306226,
0.95537613319412));
#30376=CARTESIAN_POINT('Ctrl Pts',(-0.130083979169214,0.118177768898468,
0.959080729546388));
#30377=CARTESIAN_POINT('Ctrl Pts',(-0.163326717682566,0.0649015370631265,
0.962785325898656));
#30378=CARTESIAN_POINT('Ctrl Pts',(-0.166582411702781,0.00985184688226562,
0.966489922250924));
#30379=CARTESIAN_POINT('Ctrl Pts',(-0.169838105722997,-0.045197843298595,
0.970194518603192));
#30380=CARTESIAN_POINT('Ctrl Pts',(-0.143106755250076,-0.102020991824975,
0.97389911495546));
#30381=CARTESIAN_POINT('Ctrl Pts',(-0.0986221180718627,-0.134612168562546,
0.977603711307728));
#30382=CARTESIAN_POINT('Ctrl Pts',(-0.054137480893649,-0.167203345300117,
0.981308307659997));
#30383=CARTESIAN_POINT('Ctrl Pts',(0.00810044298985758,-0.175562550248879,
0.985012904012265));
#30384=CARTESIAN_POINT('Ctrl Pts',(0.0596081167151753,-0.155864142731977,
0.988717500364533));
#30385=CARTESIAN_POINT('Ctrl Pts',(0.111115790440493,-0.136165735215075,
0.992422096716801));
#30386=CARTESIAN_POINT('Ctrl Pts',(0.151893214007622,-0.0884097152325082,
0.996126693069068));
#30387=CARTESIAN_POINT('Ctrl Pts',(0.163278367297414,-0.0344518977599609,
0.999831289421336));
#30388=CARTESIAN_POINT('Ctrl Pts',(0.165651681983942,-0.0232040140116242,
1.0006035383939));
#30389=CARTESIAN_POINT('Ctrl Pts',(0.166747775756401,-0.0116866354136458,
1.00137578736646));
#30390=CARTESIAN_POINT('Ctrl Pts',(0.166641299058679,-0.000149160109009599,
1.00214803633902));
#30391=CARTESIAN_POINT('Ctrl Pts',(0.16633703813182,-4.26131537097363E-5,
0.982851963660979));
#30392=CARTESIAN_POINT('Ctrl Pts',(0.166394664840996,-0.0252149691141755,
0.981174850743608));
#30393=CARTESIAN_POINT('Ctrl Pts',(0.161038745460081,-0.0503640488000913,
0.979497737826238));
#30394=CARTESIAN_POINT('Ctrl Pts',(0.150143538011669,-0.0728263241997442,
0.977820624908867));
#30395=CARTESIAN_POINT('Ctrl Pts',(0.126076973767522,-0.122443534017465,
0.974116028556599));
#30396=CARTESIAN_POINT('Ctrl Pts',(0.0749825823888285,-0.158951029931774,
0.970411432204331));
#30397=CARTESIAN_POINT('Ctrl Pts',(0.0202440032863241,-0.165640975250716,
0.966706835852062));
#30398=CARTESIAN_POINT('Ctrl Pts',(-0.0344945758161804,-0.172330920569658,
0.963002239499794));
#30399=CARTESIAN_POINT('Ctrl Pts',(-0.0928773426424964,-0.149203315293232,
0.959297643147526));
#30400=CARTESIAN_POINT('Ctrl Pts',(-0.128185095718787,-0.106842589675449,
0.955593046795258));
#30401=CARTESIAN_POINT('Ctrl Pts',(-0.163492848795077,-0.064481864057666,
0.95188845044299));
#30402=CARTESIAN_POINT('Ctrl Pts',(-0.175725588121342,-0.00288801809852563,
0.948183854090722));
#30403=CARTESIAN_POINT('Ctrl Pts',(-0.159284925787188,0.0497500806758803,
0.944479257738454));
#30404=CARTESIAN_POINT('Ctrl Pts',(-0.142844263453034,0.102388179450286,
0.940774661386186));
#30405=CARTESIAN_POINT('Ctrl Pts',(-0.097730199458461,0.146070531039958,
0.937070065033918));
#30406=CARTESIAN_POINT('Ctrl Pts',(-0.0445894513306832,0.160805840780395,
0.93336546868165));
#30407=CARTESIAN_POINT('Ctrl Pts',(0.00855129679709463,0.175541150520831,
0.929660872329382));
#30408=CARTESIAN_POINT('Ctrl Pts',(0.0697187290580771,0.161329418412033,
0.925956275977114));
#30409=CARTESIAN_POINT('Ctrl Pts',(0.110919243004777,0.124674377251528,
0.922251679624846));
#30410=CARTESIAN_POINT('Ctrl Pts',(0.145765426127824,0.093672621343478,
0.919118440970224));
#30411=CARTESIAN_POINT('Ctrl Pts',(0.16632871557528,0.0466165403829395,
0.915985202315602));
#30412=CARTESIAN_POINT('Ctrl Pts',(0.166729862742343,-0.000130123946020723,
0.912851963660979));
#30413=CARTESIAN_POINT('Origin',(0.,0.,1.3));
#30414=CARTESIAN_POINT('',(0.166745353727506,0.000120148921586877,0.842851963660979));
#30415=CARTESIAN_POINT('',(0.166381444272219,9.40568719243839E-5,0.86214803633902));
#30416=CARTESIAN_POINT('',(0.1666,2.04026156737949E-17,1.3));
#30417=CARTESIAN_POINT('',(-0.126907087985236,0.107935865304853,0.8));
#30418=CARTESIAN_POINT('Ctrl Pts',(0.166745353727506,0.000120148921586877,
0.842851963660979));
#30419=CARTESIAN_POINT('Ctrl Pts',(0.166350216338014,-0.0471541035618327,
0.83968176483079));
#30420=CARTESIAN_POINT('Ctrl Pts',(0.14523873930488,-0.0947247812496833,
0.836511566000602));
#30421=CARTESIAN_POINT('Ctrl Pts',(0.109671969299941,-0.125754000901643,
0.833341367170413));
#30422=CARTESIAN_POINT('Ctrl Pts',(0.0681097413514803,-0.162013787777386,
0.829636770818145));
#30423=CARTESIAN_POINT('Ctrl Pts',(0.00680803444401046,-0.175685325249421,
0.825932174465876));
#30424=CARTESIAN_POINT('Ctrl Pts',(-0.0461862781086293,-0.160386912096395,
0.822227578113608));
#30425=CARTESIAN_POINT('Ctrl Pts',(-0.0991805906612692,-0.14508849894337,
0.81852298176134));
#30426=CARTESIAN_POINT('Ctrl Pts',(-0.143867508859079,-0.100820135165284,
0.814818385409072));
#30427=CARTESIAN_POINT('Ctrl Pts',(-0.159771943968926,-0.0481139506034528,
0.811113789056804));
#30428=CARTESIAN_POINT('Ctrl Pts',(-0.175676379078773,0.00459223395837816,
0.807409192704537));
#30429=CARTESIAN_POINT('Ctrl Pts',(-0.162798331100657,0.0657362393039545,
0.803704596352268));
#30430=CARTESIAN_POINT('Ctrl Pts',(-0.126907087985236,0.107935865304854,
0.8));
#30431=CARTESIAN_POINT('',(0.127144529223414,0.10812516429919,0.8));
#30432=CARTESIAN_POINT('Origin',(0.,0.,0.8));
#30433=CARTESIAN_POINT('Ctrl Pts',(0.127144588893496,0.108125211870903,
0.8));
#30434=CARTESIAN_POINT('Ctrl Pts',(0.0920578520263333,0.149281442964014,
0.803632291818556));
#30435=CARTESIAN_POINT('Ctrl Pts',(0.0350626176413565,0.171873117908773,
0.807264583637111));
#30436=CARTESIAN_POINT('Ctrl Pts',(-0.0186760721562392,0.165810809841732,
0.810896875455666));
#30437=CARTESIAN_POINT('Ctrl Pts',(-0.0734844862772781,0.159627825248711,
0.814601471807934));
#30438=CARTESIAN_POINT('Ctrl Pts',(-0.124905415613006,0.123638729028309,
0.818306068160202));
#30439=CARTESIAN_POINT('Ctrl Pts',(-0.14943866399484,0.0742601129650432,
0.82201066451247));
#30440=CARTESIAN_POINT('Ctrl Pts',(-0.173971912376674,0.0248814969017771,
0.825715260864738));
#30441=CARTESIAN_POINT('Ctrl Pts',(-0.171617479804614,-0.0378866390043534,
0.829419857217006));
#30442=CARTESIAN_POINT('Ctrl Pts',(-0.143435789399569,-0.0852901107552215,
0.833124453569274));
#30443=CARTESIAN_POINT('Ctrl Pts',(-0.115254098994523,-0.132693582506089,
0.836829049921542));
#30444=CARTESIAN_POINT('Ctrl Pts',(-0.0612451507564931,-0.164732390101695,
0.84053364627381));
#30445=CARTESIAN_POINT('Ctrl Pts',(-0.00613536544337925,-0.166758384009028,
0.844238242626078));
#30446=CARTESIAN_POINT('Ctrl Pts',(0.0489744198697346,-0.168784377916361,
0.847942838978346));
#30447=CARTESIAN_POINT('Ctrl Pts',(0.105185042257932,-0.140797558135422,
0.851647435330614));
#30448=CARTESIAN_POINT('Ctrl Pts',(0.136776048425978,-0.0955986339274043,
0.855352031682883));
#30449=CARTESIAN_POINT('Ctrl Pts',(0.156093728823978,-0.0679598063592257,
0.857617366568262));
#30450=CARTESIAN_POINT('Ctrl Pts',(0.166205550297931,-0.0338849643656092,
0.859882701453641));
#30451=CARTESIAN_POINT('Ctrl Pts',(0.166381444272219,9.40568719243839E-5,
0.86214803633902));
#30452=CARTESIAN_POINT('Origin',(0.,0.,0.645407471946233));
#30453=CARTESIAN_POINT('',(0.205717919156333,0.000119231682504745,1.65459252805377));
#30454=CARTESIAN_POINT('',(0.20515534870289,-8.10795385496472E-5,1.66040747194623));
#30455=CARTESIAN_POINT('',(0.205475,1.17874941047504E-14,0.645407471946233));
#30456=CARTESIAN_POINT('',(-0.188262750966373,-0.0823232180103128,1.7));
#30457=CARTESIAN_POINT('Ctrl Pts',(0.20515534870289,-8.1079538549661E-5,
1.66040747194623));
#30458=CARTESIAN_POINT('Ctrl Pts',(0.205035475209089,0.0384765991859779,
1.66249119224068));
#30459=CARTESIAN_POINT('Ctrl Pts',(0.176046579400947,0.14575433740106,1.6682795088874));
#30460=CARTESIAN_POINT('Ctrl Pts',(0.00300247275662535,0.243001989931863,
1.67777242188639));
#30461=CARTESIAN_POINT('Ctrl Pts',(-0.202554499717183,0.133854462473394,
1.6888862109432));
#30462=CARTESIAN_POINT('Ctrl Pts',(-0.215637179506013,-0.0197213743559566,
1.69629540364773));
#30463=CARTESIAN_POINT('Ctrl Pts',(-0.188262750966373,-0.0823232180103128,
1.7));
#30464=CARTESIAN_POINT('',(-0.122364587709818,-0.165532040449643,1.7));
#30465=CARTESIAN_POINT('Origin',(0.,0.,1.7));
#30466=CARTESIAN_POINT('Ctrl Pts',(0.205717919156333,0.000119231682504748,
1.65459252805377));
#30467=CARTESIAN_POINT('Ctrl Pts',(0.205768208325854,0.00728313946640584,
1.65498227116049));
#30468=CARTESIAN_POINT('Ctrl Pts',(0.202179510783538,0.0824912465572326,
1.65907661061947));
#30469=CARTESIAN_POINT('Ctrl Pts',(0.109634140470589,0.216730418270261,
1.66687554643072));
#30470=CARTESIAN_POINT('Ctrl Pts',(-0.122663843019391,0.209602590285094,
1.67798933548753));
#30471=CARTESIAN_POINT('Ctrl Pts',(-0.24177601945125,0.0120092944511596,
1.68903082001062));
#30472=CARTESIAN_POINT('Ctrl Pts',(-0.175954082167323,-0.125816077227026,
1.69636770818144));
#30473=CARTESIAN_POINT('Ctrl Pts',(-0.122364641233049,-0.165532117868825,
1.7));
#30474=CARTESIAN_POINT('Origin',(0.,0.,0.645407471946233));
#30475=CARTESIAN_POINT('',(0.2051889883028,0.000102640746213675,1.58459252805377));
#30476=CARTESIAN_POINT('',(0.205663604651154,-0.000149728163284854,1.59040747194623));
#30477=CARTESIAN_POINT('',(0.205475,1.17874941047504E-14,0.645407471946233));
#30478=CARTESIAN_POINT('Ctrl Pts',(0.205663604651154,-0.000149728163284867,
1.59040747194623));
#30479=CARTESIAN_POINT('Ctrl Pts',(0.205182444335985,0.0585183956951034,
1.59359694746041));
#30480=CARTESIAN_POINT('Ctrl Pts',(0.148135327616145,0.186146531383155,
1.60049101932685));
#30481=CARTESIAN_POINT('Ctrl Pts',(-0.0684290720584363,0.233024356666725,
1.61108968754557));
#30482=CARTESIAN_POINT('Ctrl Pts',(-0.23288917800895,0.0688795811193509,
1.62220347660237));
#30483=CARTESIAN_POINT('Ctrl Pts',(-0.184175405168835,-0.158290127824162,
1.63331726565918));
#30484=CARTESIAN_POINT('Ctrl Pts',(0.0331013206128567,-0.240615925517378,
1.64443105471598));
#30485=CARTESIAN_POINT('Ctrl Pts',(0.185046630854554,-0.128496885183325,
1.65346112347833));
#30486=CARTESIAN_POINT('Ctrl Pts',(0.205248595419634,-0.0300741733602017,
1.65878659588842));
#30487=CARTESIAN_POINT('Ctrl Pts',(0.20515534870289,-8.1079538549661E-5,
1.66040747194623));
#30488=CARTESIAN_POINT('Ctrl Pts',(0.2051889883028,0.000102640746213654,
1.58459252805377));
#30489=CARTESIAN_POINT('Ctrl Pts',(0.205314142408481,0.0277738688435417,
1.58608802638021));
#30490=CARTESIAN_POINT('Ctrl Pts',(0.187212802641802,0.123834372120327,
1.59128812105892));
#30491=CARTESIAN_POINT('Ctrl Pts',(0.041212233239435,0.2393392912824,1.6001928120899));
#30492=CARTESIAN_POINT('Ctrl Pts',(-0.178731921787321,0.164428017156146,
1.6113066011467));
#30493=CARTESIAN_POINT('Ctrl Pts',(-0.235078089364662,-0.0609842187918821,
1.62242039020351));
#30494=CARTESIAN_POINT('Ctrl Pts',(-0.0762596568913861,-0.230580482955351,
1.63353417926032));
#30495=CARTESIAN_POINT('Ctrl Pts',(0.144352083897931,-0.190571029763675,
1.6442582252104));
#30496=CARTESIAN_POINT('Ctrl Pts',(0.205290198398921,-0.0608114238158697,
1.65127767480822));
#30497=CARTESIAN_POINT('Ctrl Pts',(0.205717919156333,0.000119231682504748,
1.65459252805377));
#30498=CARTESIAN_POINT('Origin',(0.,0.,0.645407471946233));
#30499=CARTESIAN_POINT('',(0.205346259354759,-0.00017652456807675,1.51459252805377));
#30500=CARTESIAN_POINT('',(0.205625119184624,0.000163390229490382,1.52040747194623));
#30501=CARTESIAN_POINT('',(0.205475,1.17874941047504E-14,0.645407471946233));
#30502=CARTESIAN_POINT('Ctrl Pts',(0.205625119184624,0.000163390229490371,
1.52040747194623));
#30503=CARTESIAN_POINT('Ctrl Pts',(0.205719589271595,0.0110330279545173,
1.52099810632787));
#30504=CARTESIAN_POINT('Ctrl Pts',(0.199992588366042,0.0899798330776656,
1.52529333706177));
#30505=CARTESIAN_POINT('Ctrl Pts',(0.0977367556084749,0.222326520064881,
1.53329316414794));
#30506=CARTESIAN_POINT('Ctrl Pts',(-0.133782052044684,0.202691772286445,
1.54440695320474));
#30507=CARTESIAN_POINT('Ctrl Pts',(-0.242848712699985,-0.00246927953082339,
1.55552074226155));
#30508=CARTESIAN_POINT('Ctrl Pts',(-0.129633034711377,-0.205369738746763,
1.56663453131835));
#30509=CARTESIAN_POINT('Ctrl Pts',(0.102236927935064,-0.220293776124516,
1.57774832037515));
#30510=CARTESIAN_POINT('Ctrl Pts',(0.20084133199376,-0.0871629660671419,
1.58567263391778));
#30511=CARTESIAN_POINT('Ctrl Pts',(0.205741315141077,-0.00962500803198312,
1.58989235110814));
#30512=CARTESIAN_POINT('Ctrl Pts',(0.205663604651154,-0.000149728163284867,
1.59040747194623));
#30513=CARTESIAN_POINT('Ctrl Pts',(0.205346259354759,-0.000176524568076758,
1.51459252805377));
#30514=CARTESIAN_POINT('Ctrl Pts',(0.204952685935524,0.0478618563462208,
1.51719378159994));
#30515=CARTESIAN_POINT('Ctrl Pts',(0.164184854806731,0.1649162911311,1.52349963149837));
#30516=CARTESIAN_POINT('Ctrl Pts',(-0.0308180903310451,0.240897960470908,
1.53351007774908));
#30517=CARTESIAN_POINT('Ctrl Pts',(-0.219105973246366,0.104757609325286,
1.54462386680588));
#30518=CARTESIAN_POINT('Ctrl Pts',(-0.206843620635952,-0.127268531807556,
1.55573765586268));
#30519=CARTESIAN_POINT('Ctrl Pts',(-0.00525505851706014,-0.242804414954791,
1.56685144491949));
#30520=CARTESIAN_POINT('Ctrl Pts',(0.173370196153793,-0.15045712725832,
1.57646973564985));
#30521=CARTESIAN_POINT('Ctrl Pts',(0.20500411501816,-0.0407723333551383,
1.58238343002794));
#30522=CARTESIAN_POINT('Ctrl Pts',(0.2051889883028,0.000102640746213654,
1.58459252805377));
#30523=CARTESIAN_POINT('Origin',(0.,0.,0.645407471946233));
#30524=CARTESIAN_POINT('',(0.205812292792875,8.2771271442428E-7,1.44459252805377));
#30525=CARTESIAN_POINT('',(0.20514810115636,4.68968264668604E-5,1.45040747194623));
#30526=CARTESIAN_POINT('',(0.205475,1.17874941047504E-14,0.645407471946233));
#30527=CARTESIAN_POINT('Ctrl Pts',(0.20514810115636,4.68968264668648E-5,
1.45040747194623));
#30528=CARTESIAN_POINT('Ctrl Pts',(0.205212209277079,0.0314508805486537,
1.45210386154759));
#30529=CARTESIAN_POINT('Ctrl Pts',(0.183673234943095,0.131351887215635,
1.45750484750122));
#30530=CARTESIAN_POINT('Ctrl Pts',(0.028210615278035,0.241217190661839,
1.46661042980711));
#30531=CARTESIAN_POINT('Ctrl Pts',(-0.187360277963068,0.154524103926572,
1.47772421886392));
#30532=CARTESIAN_POINT('Ctrl Pts',(-0.23143818564818,-0.0736066521476796,
1.48883800792072));
#30533=CARTESIAN_POINT('Ctrl Pts',(-0.0636780941176189,-0.234364395962394,
1.49995179697753));
#30534=CARTESIAN_POINT('Ctrl Pts',(0.15035425339619,-0.183462731047792,
1.51047495165269));
#30535=CARTESIAN_POINT('Ctrl Pts',(0.205127050891722,-0.0571438705105598,
1.5172935099756));
#30536=CARTESIAN_POINT('Ctrl Pts',(0.205625119184624,0.000163390229490371,
1.52040747194623));
#30537=CARTESIAN_POINT('Ctrl Pts',(0.205812290976358,8.27708256686491E-7,
1.44459252805377));
#30538=CARTESIAN_POINT('Ctrl Pts',(0.205812293621698,4.5117938930396E-5,
1.44459494046739));
#30539=CARTESIAN_POINT('Ctrl Pts',(0.205792223959932,0.0681032095145843,
1.44830194923329));
#30540=CARTESIAN_POINT('Ctrl Pts',(0.13158183823911,0.204126920402922,1.45571355435144));
#30541=CARTESIAN_POINT('Ctrl Pts',(-0.10013585656473,0.221256389923926,
1.46682734340825));
#30542=CARTESIAN_POINT('Ctrl Pts',(-0.240198066802314,0.0358673761285168,
1.47794113246505));
#30543=CARTESIAN_POINT('Ctrl Pts',(-0.160404261381875,-0.182351453033287,
1.48905492152186));
#30544=CARTESIAN_POINT('Ctrl Pts',(0.0662093815164626,-0.233661930697804,
1.50016871057866));
#30545=CARTESIAN_POINT('Ctrl Pts',(0.193364787149743,-0.109147888339539,
1.5086812460893));
#30546=CARTESIAN_POINT('Ctrl Pts',(0.20551319671518,-0.0205523937625982,
1.51348918524767));
#30547=CARTESIAN_POINT('Ctrl Pts',(0.205346259354759,-0.000176524568076758,
1.51459252805377));
#30548=CARTESIAN_POINT('Origin',(0.,0.,0.645407471946233));
#30549=CARTESIAN_POINT('',(0.205343844683429,0.000176004178461642,1.37459252805377));
#30550=CARTESIAN_POINT('',(0.205453133831238,-0.000187888241826064,1.38040747194623));
#30551=CARTESIAN_POINT('',(0.205475,1.17874941047504E-14,0.645407471946233));
#30552=CARTESIAN_POINT('Ctrl Pts',(0.205453133831238,-0.000187888241826079,
1.38040747194623));
#30553=CARTESIAN_POINT('Ctrl Pts',(0.204982640394683,0.0514920396676331,
1.38320961676732));
#30554=CARTESIAN_POINT('Ctrl Pts',(0.159017805479884,0.172241441932577,
1.38971635794067));
#30555=CARTESIAN_POINT('Ctrl Pts',(-0.0437982449057285,0.238879228826581,
1.39992769546629));
#30556=CARTESIAN_POINT('Ctrl Pts',(-0.224449621610114,0.0927574233548304,
1.41104148452309));
#30557=CARTESIAN_POINT('Ctrl Pts',(-0.199659714256911,-0.13826630374757,
1.42215527357989));
#30558=CARTESIAN_POINT('Ctrl Pts',(0.00788099391586731,-0.242733314804761,
1.4332690626367));
#30559=CARTESIAN_POINT('Ctrl Pts',(0.177630548818419,-0.142990752308629,
1.44268646209214));
#30560=CARTESIAN_POINT('Ctrl Pts',(0.205072209179237,-0.037129523063069,
1.44839926519532));
#30561=CARTESIAN_POINT('Ctrl Pts',(0.20514810115636,4.68968264668648E-5,
1.45040747194623));
#30562=CARTESIAN_POINT('Ctrl Pts',(0.205343844683429,0.000176004178461609,
1.37459252805377));
#30563=CARTESIAN_POINT('Ctrl Pts',(0.2055108740339,0.0206415845782027,1.37570069568712));
#30564=CARTESIAN_POINT('Ctrl Pts',(0.193294976926761,0.109328542053589,
1.38051345967274));
#30565=CARTESIAN_POINT('Ctrl Pts',(0.0659057470887793,0.233747753644337,
1.38903082001062));
#30566=CARTESIAN_POINT('Ctrl Pts',(-0.160641042350602,0.182142898149225,
1.40014460906743));
#30567=CARTESIAN_POINT('Ctrl Pts',(-0.240151263944613,-0.0361794176709605,
1.41125839812423));
#30568=CARTESIAN_POINT('Ctrl Pts',(-0.0998483101275995,-0.221386302178844,
1.42237218718103));
#30569=CARTESIAN_POINT('Ctrl Pts',(0.131796641356581,-0.203959577192589,
1.43348356382421));
#30570=CARTESIAN_POINT('Ctrl Pts',(0.205808231334455,-0.0679686858761153,
1.44089034411512));
#30571=CARTESIAN_POINT('Ctrl Pts',(0.205812290976358,8.27708256686491E-7,
1.44459252805377));
#30572=CARTESIAN_POINT('Origin',(0.,0.,0.645407471946233));
#30573=CARTESIAN_POINT('',(0.205190393281102,-0.000103909026722956,1.30459252805377));
#30574=CARTESIAN_POINT('',(0.205784930460293,6.78762012092915E-5,1.31040747194623));
#30575=CARTESIAN_POINT('',(0.205475,1.17874941047504E-14,0.645407471946233));
#30576=CARTESIAN_POINT('Ctrl Pts',(0.205784930460293,6.78762012092937E-5,
1.31040747194623));
#30577=CARTESIAN_POINT('Ctrl Pts',(0.205801002271222,0.00380171834571078,
1.31061077563477));
#30578=CARTESIAN_POINT('Ctrl Pts',(0.204016743590097,0.0755578983061786,
1.31451867567558));
#30579=CARTESIAN_POINT('Ctrl Pts',(0.120352309668968,0.210942868533614,
1.32213117206866));
#30580=CARTESIAN_POINT('Ctrl Pts',(-0.111952589707427,0.215518421220722,
1.33324496112546));
#30581=CARTESIAN_POINT('Ctrl Pts',(-0.241786014095534,0.0228275188203595,
1.34435875018226));
#30582=CARTESIAN_POINT('Ctrl Pts',(-0.150309957742793,-0.190757670439842,
1.35547253923907));
#30583=CARTESIAN_POINT('Ctrl Pts',(0.0787465075641072,-0.229740200603712,
1.36658632829588));
#30584=CARTESIAN_POINT('Ctrl Pts',(0.196145957186436,-0.101629499882189,
1.37489797253159));
#30585=CARTESIAN_POINT('Ctrl Pts',(0.205604659733481,-0.0168317924834936,
1.37950502041505));
#30586=CARTESIAN_POINT('Ctrl Pts',(0.205453133831238,-0.000187888241826079,
1.38040747194623));
#30587=CARTESIAN_POINT('Ctrl Pts',(0.205190393281102,-0.000103909026722949,
1.30459252805377));
#30588=CARTESIAN_POINT('Ctrl Pts',(0.205002798510851,0.0408596785255145,
1.30680645090684));
#30589=CARTESIAN_POINT('Ctrl Pts',(0.173264151191812,0.15063609956695,1.31272497011219));
#30590=CARTESIAN_POINT('Ctrl Pts',(-0.00557045627447471,0.242797343170749,
1.3223480856698));
#30591=CARTESIAN_POINT('Ctrl Pts',(-0.207008825709279,0.126999708315969,
1.3334618747266));
#30592=CARTESIAN_POINT('Ctrl Pts',(-0.218969669332857,-0.105042199835232,
1.3445756637834));
#30593=CARTESIAN_POINT('Ctrl Pts',(-0.0305050913306782,-0.240937791217362,
1.35568945284021));
#30594=CARTESIAN_POINT('Ctrl Pts',(0.164305043004325,-0.164739584440547,
1.36569507426366));
#30595=CARTESIAN_POINT('Ctrl Pts',(0.204952496128017,-0.0477747021046654,
1.37199609933485));
#30596=CARTESIAN_POINT('Ctrl Pts',(0.205343844683429,0.000176004178461609,
1.37459252805377));
#30597=CARTESIAN_POINT('Origin',(0.,0.,0.645407471946233));
#30598=CARTESIAN_POINT('',(0.205723053630104,-0.00012021653370823,1.23459252805377));
#30599=CARTESIAN_POINT('',(0.2052527421894,0.000145096082381024,1.24040747194623));
#30600=CARTESIAN_POINT('',(0.205475,1.17874941047504E-14,0.645407471946233));
#30601=CARTESIAN_POINT('Ctrl Pts',(0.2052527421894,0.000145096082381054,
1.24040747194623));
#30602=CARTESIAN_POINT('Ctrl Pts',(0.205410551512377,0.0243477880181972,
1.2417165308545));
#30603=CARTESIAN_POINT('Ctrl Pts',(0.19025975845005,0.116852155262949,1.24673018611503));
#30604=CARTESIAN_POINT('Ctrl Pts',(0.053170711887795,0.236969296798376,
1.25544843772783));
#30605=CARTESIAN_POINT('Ctrl Pts',(-0.170254416296827,0.17319066360285,
1.26656222678464));
#30606=CARTESIAN_POINT('Ctrl Pts',(-0.237843746428552,-0.0491113481040567,
1.27767601584144));
#30607=CARTESIAN_POINT('Ctrl Pts',(-0.0877319981226961,-0.226461185930791,
1.28878980489824));
#30608=CARTESIAN_POINT('Ctrl Pts',(0.138466900336863,-0.197076087766382,
1.29970029026651));
#30609=CARTESIAN_POINT('Ctrl Pts',(0.205508142006035,-0.0642362896597867,
1.3069061792825));
#30610=CARTESIAN_POINT('Ctrl Pts',(0.205784930460293,6.78762012092937E-5,
1.31040747194623));
#30611=CARTESIAN_POINT('Ctrl Pts',(0.205723053630104,-0.000120216533708221,
1.23459252805377));
#30612=CARTESIAN_POINT('Ctrl Pts',(0.205298918797858,0.0608969853087639,
1.23791220612657));
#30613=CARTESIAN_POINT('Ctrl Pts',(0.144198668474879,0.190744063350028,
1.24493648055164));
#30614=CARTESIAN_POINT('Ctrl Pts',(-0.0765564251386213,0.230479269358191,
1.25566535132897));
#30615=CARTESIAN_POINT('Ctrl Pts',(-0.23515855594305,0.0606797610465845,
1.26677914038578));
#30616=CARTESIAN_POINT('Ctrl Pts',(-0.178517393613401,-0.164660620706261,
1.27789292944258));
#30617=CARTESIAN_POINT('Ctrl Pts',(0.0415227636155418,-0.239285268948212,
1.28900671849938));
#30618=CARTESIAN_POINT('Ctrl Pts',(0.187294592944535,-0.123653783093607,
1.29790658470311));
#30619=CARTESIAN_POINT('Ctrl Pts',(0.205316704165066,-0.0276854186132918,
1.30310185455457));
#30620=CARTESIAN_POINT('Ctrl Pts',(0.205190393281102,-0.000103909026722949,
1.30459252805377));
#30621=CARTESIAN_POINT('Origin',(0.,0.,0.645407471946233));
#30622=CARTESIAN_POINT('',(0.205554604385647,0.000179910838621594,1.16459252805377));
#30623=CARTESIAN_POINT('',(0.205260574591088,-0.000148793951100861,1.17040747194623));
#30624=CARTESIAN_POINT('',(0.205475,1.17874941047504E-14,0.645407471946233));
#30625=CARTESIAN_POINT('Ctrl Pts',(0.205260574591088,-0.000148793951100864,
1.17040747194623));
#30626=CARTESIAN_POINT('Ctrl Pts',(0.204961311968991,0.044493502374408,
1.17282228607422));
#30627=CARTESIAN_POINT('Ctrl Pts',(0.168697767785137,0.158064764697474,
1.17894169655448));
#30628=CARTESIAN_POINT('Ctrl Pts',(-0.0186902364010947,0.242140965743205,
1.18876570338701));
#30629=CARTESIAN_POINT('Ctrl Pts',(-0.213572804428157,0.115621059658089,
1.19987949244381));
#30630=CARTESIAN_POINT('Ctrl Pts',(-0.212969762481792,-0.116728113564033,
1.21099328150062));
#30631=CARTESIAN_POINT('Ctrl Pts',(-0.0174330816944656,-0.242234720654174,
1.22210707055742));
#30632=CARTESIAN_POINT('Ctrl Pts',(0.169149144270981,-0.157353841391122,
1.23191180070596));
#30633=CARTESIAN_POINT('Ctrl Pts',(0.204963955993594,-0.0441450839941835,
1.23801193450223));
#30634=CARTESIAN_POINT('Ctrl Pts',(0.2052527421894,0.000145096082381054,
1.24040747194623));
#30635=CARTESIAN_POINT('Ctrl Pts',(0.205554604385647,0.00017991083862162,
1.16459252805377));
#30636=CARTESIAN_POINT('Ctrl Pts',(0.205676289601756,0.0134574818611262,
1.16531336499402));
#30637=CARTESIAN_POINT('Ctrl Pts',(0.198454332603713,0.094840644563722,
1.16973879828655));
#30638=CARTESIAN_POINT('Ctrl Pts',(0.0898833437085198,0.225615966539919,
1.17786882793134));
#30639=CARTESIAN_POINT('Ctrl Pts',(-0.140804956527845,0.197877598659039,
1.18898261698814));
#30640=CARTESIAN_POINT('Ctrl Pts',(-0.242612883217311,-0.0109803793588139,
1.20009640604495));
#30641=CARTESIAN_POINT('Ctrl Pts',(-0.12235448648082,-0.2097878916237,1.21121019510175));
#30642=CARTESIAN_POINT('Ctrl Pts',(0.109896359325859,-0.21657416752884,
1.22232398415856));
#30643=CARTESIAN_POINT('Ctrl Pts',(0.202230669468777,-0.082312541395209,
1.23011809514256));
#30644=CARTESIAN_POINT('Ctrl Pts',(0.20577223226921,-0.00719519062340044,
1.2342076097743));
#30645=CARTESIAN_POINT('Ctrl Pts',(0.205723053630104,-0.000120216533708221,
1.23459252805377));
#30646=CARTESIAN_POINT('Origin',(0.,0.,0.645407471946233));
#30647=CARTESIAN_POINT('',(0.205138522353965,7.81005524626288E-6,1.09459252805377));
#30648=CARTESIAN_POINT('',(0.205789655863746,-6.17368779781373E-5,1.10040747194623));
#30649=CARTESIAN_POINT('',(0.205475,1.17874941047504E-14,0.645407471946233));
#30650=CARTESIAN_POINT('Ctrl Pts',(0.205789655863746,-6.17368779781361E-5,
1.10040747194623));
#30651=CARTESIAN_POINT('Ctrl Pts',(0.205533723504375,0.0645925032691717,
1.10392804129395));
#30652=CARTESIAN_POINT('Ctrl Pts',(0.137841967409279,0.197742342810066,
1.11115320699393));
#30653=CARTESIAN_POINT('Ctrl Pts',(-0.0889063286388705,0.226002736612265,
1.12208296904618));
#30654=CARTESIAN_POINT('Ctrl Pts',(-0.238095468835566,0.0478760895194249,
1.13319675810299));
#30655=CARTESIAN_POINT('Ctrl Pts',(-0.169353126220915,-0.174072085260317,
1.14431054715979));
#30656=CARTESIAN_POINT('Ctrl Pts',(0.0544000534188783,-0.236690106290626,
1.1554243362166));
#30657=CARTESIAN_POINT('Ctrl Pts',(0.190562019135808,-0.116130140045317,
1.16412331114541));
#30658=CARTESIAN_POINT('Ctrl Pts',(0.2054204144752,-0.0239927989965278,
1.16911768972195));
#30659=CARTESIAN_POINT('Ctrl Pts',(0.205260574591088,-0.000148793951100864,
1.17040747194623));
#30660=CARTESIAN_POINT('Ctrl Pts',(0.205138522353965,7.81005524630105E-6,
1.09459252805377));
#30661=CARTESIAN_POINT('Ctrl Pts',(0.205149988139531,0.033826082896543,
1.09641912021375));
#30662=CARTESIAN_POINT('Ctrl Pts',(0.181232693643337,0.1362174972132,1.101950308726));
#30663=CARTESIAN_POINT('Ctrl Pts',(0.019737729131079,0.242057848222183,
1.11118609359052));
#30664=CARTESIAN_POINT('Ctrl Pts',(-0.192661783512051,0.147861479120299,
1.12229988264732));
#30665=CARTESIAN_POINT('Ctrl Pts',(-0.228715780766039,-0.0816741786716276,
1.13341367170413));
#30666=CARTESIAN_POINT('Ctrl Pts',(-0.0554236300753314,-0.236452534483491,
1.14452746076093));
#30667=CARTESIAN_POINT('Ctrl Pts',(0.15406839794226,-0.178801760545413,
1.15492041287748));
#30668=CARTESIAN_POINT('Ctrl Pts',(0.205050912928411,-0.0547799216762583,
1.16160876864176));
#30669=CARTESIAN_POINT('Ctrl Pts',(0.205554604385647,0.00017991083862162,
1.16459252805377));
#30670=CARTESIAN_POINT('Origin',(0.,0.,0.645407471946233));
#30671=CARTESIAN_POINT('',(0.20552593591886,-0.000183965626637278,1.02459252805377));
#30672=CARTESIAN_POINT('',(0.20544247508097,0.000187699708462681,1.03040747194623));
#30673=CARTESIAN_POINT('',(0.205475,1.17874941047504E-14,0.645407471946233));
#30674=CARTESIAN_POINT('Ctrl Pts',(0.20544247508097,0.000187699708462687,
1.03040747194623));
#30675=CARTESIAN_POINT('Ctrl Pts',(0.205596383177594,0.0171893738494543,
1.0313292001614));
#30676=CARTESIAN_POINT('Ctrl Pts',(0.195889593181661,0.102350581389175,
1.03595552472885));
#30677=CARTESIAN_POINT('Ctrl Pts',(0.0775529135379212,0.230145861972334,
1.04428644564855));
#30678=CARTESIAN_POINT('Ctrl Pts',(-0.151298115744515,0.18997487313149,
1.05540023470536));
#30679=CARTESIAN_POINT('Ctrl Pts',(-0.241664263837854,-0.0240822717379046,
1.06651402376216));
#30680=CARTESIAN_POINT('Ctrl Pts',(-0.110832370586897,-0.216096640074974,
1.07762781281897));
#30681=CARTESIAN_POINT('Ctrl Pts',(0.121445648389767,-0.210315303100593,
1.08874160187577));
#30682=CARTESIAN_POINT('Ctrl Pts',(0.204196124007957,-0.074841794914668,
1.09633482158486));
#30683=CARTESIAN_POINT('Ctrl Pts',(0.205803033945758,-0.00344133971228389,
1.10022344494168));
#30684=CARTESIAN_POINT('Ctrl Pts',(0.205789655863746,-6.17368779781361E-5,
1.10040747194623));
#30685=CARTESIAN_POINT('Ctrl Pts',(0.20552593591886,-0.000183965626637285,
1.02459252805377));
#30686=CARTESIAN_POINT('Ctrl Pts',(0.205027284976747,0.0538482597648122,
1.02752487543347));
#30687=CARTESIAN_POINT('Ctrl Pts',(0.155496650182077,0.176951247041673,
1.03416181916545));
#30688=CARTESIAN_POINT('Ctrl Pts',(-0.0521449271278155,0.237197146991165,
1.04450335924969));
#30689=CARTESIAN_POINT('Ctrl Pts',(-0.227563185653378,0.0848326375129703,
1.0556171483065));
#30690=CARTESIAN_POINT('Ctrl Pts',(-0.194690279246867,-0.145180146557101,
1.0667309373633));
#30691=CARTESIAN_POINT('Ctrl Pts',(0.0163848475034698,-0.242307896337387,
1.0778447264201));
#30692=CARTESIAN_POINT('Ctrl Pts',(0.180236614284166,-0.138136714556845,
1.08713192331693));
#30693=CARTESIAN_POINT('Ctrl Pts',(0.205126733847568,-0.0347623261378718,
1.09271452386148));
#30694=CARTESIAN_POINT('Ctrl Pts',(0.205138522353965,7.81005524630105E-6,
1.09459252805377));
#30695=CARTESIAN_POINT('Origin',(0.,0.,0.645407471946233));
#30696=CARTESIAN_POINT('',(0.205743448352251,0.000106566711118361,0.954592528053768));
#30697=CARTESIAN_POINT('',(0.205150677731907,-5.25566492129599E-5,0.960407471946232));
#30698=CARTESIAN_POINT('',(0.205475,1.17874941047504E-14,0.645407471946233));
#30699=CARTESIAN_POINT('Ctrl Pts',(0.205150677731907,-5.25566492129668E-5,
0.960407471946232));
#30700=CARTESIAN_POINT('Ctrl Pts',(0.205064756039612,0.0374795435537448,
0.962434955381129));
#30701=CARTESIAN_POINT('Ctrl Pts',(0.177234439623409,0.143708517228788,
0.968167035168295));
#30702=CARTESIAN_POINT('Ctrl Pts',(0.00662091032790181,0.242770948244842,
0.977603711307729));
#30703=CARTESIAN_POINT('Ctrl Pts',(-0.200374735874429,0.13722805194188,
0.988717500364533));
#30704=CARTESIAN_POINT('Ctrl Pts',(-0.223965113394512,-0.0939212459185429,
0.999831289421336));
#30705=CARTESIAN_POINT('Ctrl Pts',(-0.0425576829655005,-0.239103357370329,
1.01094507847814));
#30706=CARTESIAN_POINT('Ctrl Pts',(0.159527519870246,-0.171541476398135,
1.02113713931977));
#30707=CARTESIAN_POINT('Ctrl Pts',(0.204977798041595,-0.0511435023372491,
1.02762460380914));
#30708=CARTESIAN_POINT('Ctrl Pts',(0.20544247508097,0.000187699708462687,
1.03040747194623));
#30709=CARTESIAN_POINT('Ctrl Pts',(0.205743448352251,0.000106566711118368,
0.954592528053768));
#30710=CARTESIAN_POINT('Ctrl Pts',(0.205782131072789,0.00623496563411944,
0.954926034300931));
#30711=CARTESIAN_POINT('Ctrl Pts',(0.202754080859383,0.0803990246761448,
0.958964136900363));
#30712=CARTESIAN_POINT('Ctrl Pts',(0.112884009708659,0.215032004451281,
0.966706835852063));
#30713=CARTESIAN_POINT('Ctrl Pts',(-0.119438498942156,0.211461649464463,
0.977820624908867));
#30714=CARTESIAN_POINT('Ctrl Pts',(-0.242437629122786,0.0143379927471741,
0.988934413965671));
#30715=CARTESIAN_POINT('Ctrl Pts',(-0.143530830111561,-0.195909362177039,
1.00004820302247));
#30716=CARTESIAN_POINT('Ctrl Pts',(0.086751356142284,-0.226838671363958,
1.01116199207928));
#30717=CARTESIAN_POINT('Ctrl Pts',(0.19782031948766,-0.0967615068704032,
1.01934343375638));
#30718=CARTESIAN_POINT('Ctrl Pts',(0.205657258244577,-0.0144136339232786,
1.02382027908121));
#30719=CARTESIAN_POINT('Ctrl Pts',(0.20552593591886,-0.000183965626637285,
1.02459252805377));
#30720=CARTESIAN_POINT('Origin',(0.,0.,0.645407471946233));
#30721=CARTESIAN_POINT('',(0.205205445749305,0.000116004416325019,0.884592528053768));
#30722=CARTESIAN_POINT('',(0.205635165348036,-0.000160487501855341,0.890407471946233));
#30723=CARTESIAN_POINT('',(0.205475,1.17874941047504E-14,0.645407471946233));
#30724=CARTESIAN_POINT('Ctrl Pts',(0.205635165348036,-0.000160487501855345,
0.890407471946233));
#30725=CARTESIAN_POINT('Ctrl Pts',(0.20514041316225,0.0574941994909011,
0.893540710600855));
#30726=CARTESIAN_POINT('Ctrl Pts',(0.149792439928844,0.184149942781777,
0.900378545607745));
#30727=CARTESIAN_POINT('Ctrl Pts',(-0.0648937601106981,0.234030453531351,
0.910920976966904));
#30728=CARTESIAN_POINT('Ctrl Pts',(-0.231817150854124,0.0724044416546206,
0.922034766023707));
#30729=CARTESIAN_POINT('Ctrl Pts',(-0.186555648217912,-0.155494636948999,
0.933148555080512));
#30730=CARTESIAN_POINT('Ctrl Pts',(0.029462341223335,-0.241067470577576,
0.944262344137316));
#30731=CARTESIAN_POINT('Ctrl Pts',(0.184024675492061,-0.130631009068519,
0.953348649759223));
#30732=CARTESIAN_POINT('Ctrl Pts',(0.205221751249722,-0.031098714158076,
0.958730359028861));
#30733=CARTESIAN_POINT('Ctrl Pts',(0.205150677731907,-5.25566492129668E-5,
0.960407471946232));
#30734=CARTESIAN_POINT('Ctrl Pts',(0.205205445749305,0.000116004416325009,
0.884592528053768));
#30735=CARTESIAN_POINT('Ctrl Pts',(0.205343275267841,0.0267417723340512,
0.886031789520656));
#30736=CARTESIAN_POINT('Ctrl Pts',(0.188156931475396,0.121730614284078,
0.891175647339813));
#30737=CARTESIAN_POINT('Ctrl Pts',(0.0448304764247631,0.238686010114805,
0.900024101511237));
#30738=CARTESIAN_POINT('Ctrl Pts',(-0.176220286722883,0.167116974718297,
0.911137890568042));
#30739=CARTESIAN_POINT('Ctrl Pts',(-0.235976306336092,-0.0574188764093974,
0.922251679624847));
#30740=CARTESIAN_POINT('Ctrl Pts',(-0.0797396575425977,-0.229397140881452,
0.933365468681649));
#30741=CARTESIAN_POINT('Ctrl Pts',(0.142604551604849,-0.192546391773689,
0.944145751491291));
#30742=CARTESIAN_POINT('Ctrl Pts',(0.205352442373934,-0.0618394542260256,
0.951221437948663));
#30743=CARTESIAN_POINT('Ctrl Pts',(0.205743448352251,0.000106566711118368,
0.954592528053768));
#30744=CARTESIAN_POINT('Origin',(0.,0.,0.645407471946233));
#30745=CARTESIAN_POINT('',(0.205269394176581,-0.000252214316689744,0.814592528053768));
#30746=CARTESIAN_POINT('',(0.205654271051376,0.000148184871923512,0.820407471946232));
#30747=CARTESIAN_POINT('',(0.205475,1.17874941047504E-14,0.645407471946233));
#30748=CARTESIAN_POINT('',(0.0530170217188605,-0.198517432567172,0.8));
#30749=CARTESIAN_POINT('Ctrl Pts',(0.0530170217188587,-0.198517432567173,
0.8));
#30750=CARTESIAN_POINT('Ctrl Pts',(0.119028790974553,-0.18088801151799,
0.803704596352268));
#30751=CARTESIAN_POINT('Ctrl Pts',(0.192500600447326,-0.111310459456284,
0.80856877237019));
#30752=CARTESIAN_POINT('Ctrl Pts',(0.205431969941924,-0.0216798251681207,
0.813432948388113));
#30753=CARTESIAN_POINT('Ctrl Pts',(0.205269394176581,-0.000252214316689755,
0.814592528053767));
#30754=CARTESIAN_POINT('',(-0.0531250535940746,-0.19887604744663,0.8));
#30755=CARTESIAN_POINT('Origin',(0.,0.,0.8));
#30756=CARTESIAN_POINT('Ctrl Pts',(-0.053125080564462,-0.198876136975597,
0.8));
#30757=CARTESIAN_POINT('Ctrl Pts',(0.0113386551506616,-0.21601151578625,
0.803632291818556));
#30758=CARTESIAN_POINT('Ctrl Pts',(0.149296237339328,-0.184051126983177,
0.810434782467299));
#30759=CARTESIAN_POINT('Ctrl Pts',(0.205166930984713,-0.0581571994559903,
0.817237273116043));
#30760=CARTESIAN_POINT('Ctrl Pts',(0.205654271051376,0.000148184871923506,
0.820407471946232));
#30761=CARTESIAN_POINT('Origin',(0.,0.,3.1));
#30762=CARTESIAN_POINT('',(-0.126245549239308,1.45328325776573E-5,2.71934196736194));
#30763=CARTESIAN_POINT('',(-0.126374981062586,-0.000161346902988299,2.70565803263806));
#30764=CARTESIAN_POINT('',(-0.12645,1.54856587752183E-17,3.1));
#30765=CARTESIAN_POINT('',(-0.0958116152722464,0.0825211298936403,2.7));
#30766=CARTESIAN_POINT('Ctrl Pts',(-0.126374981062586,-0.000161346902988299,
2.70565803263806));
#30767=CARTESIAN_POINT('Ctrl Pts',(-0.126107573254536,0.0297492098111863,
2.70377202175871));
#30768=CARTESIAN_POINT('Ctrl Pts',(-0.115369380269341,0.0598134784363487,
2.70188601087935));
#30769=CARTESIAN_POINT('Ctrl Pts',(-0.0958116152722464,0.0825211298936403,
2.7));
#30770=CARTESIAN_POINT('',(-0.12645,1.54856587752183E-17,2.7));
#30771=CARTESIAN_POINT('Origin',(0.,0.,2.7));
#30772=CARTESIAN_POINT('',(-0.12645,-1.54856587752183E-17,2.6));
#30773=CARTESIAN_POINT('',(-0.12645,1.54856587752183E-17,3.1));
#30774=CARTESIAN_POINT('Origin',(0.,0.,2.6));
#30775=CARTESIAN_POINT('',(0.095991445127536,0.0826500758460347,2.7));
#30776=CARTESIAN_POINT('Origin',(0.,0.,2.7));
#30777=CARTESIAN_POINT('Ctrl Pts',(0.0959918005672157,0.0826503307119909,
2.7));
#30778=CARTESIAN_POINT('Ctrl Pts',(0.0697118516972522,0.11301027640157,
2.70253749952686));
#30779=CARTESIAN_POINT('Ctrl Pts',(0.0277082938822606,0.129939474688335,
2.70507499905372));
#30780=CARTESIAN_POINT('Ctrl Pts',(-0.0122513412479025,0.126048724837631,
2.70761249858058));
#30781=CARTESIAN_POINT('Ctrl Pts',(-0.0537056163258554,0.122012446376998,
2.71024491008919));
#30782=CARTESIAN_POINT('Ctrl Pts',(-0.092960208469122,0.0955696038330054,
2.7128773215978));
#30783=CARTESIAN_POINT('Ctrl Pts',(-0.1122448026076,0.0586681233168463,
2.71550973310641));
#30784=CARTESIAN_POINT('Ctrl Pts',(-0.121602899042457,0.0407612070094829,
2.71678714452492));
#30785=CARTESIAN_POINT('Ctrl Pts',(-0.126258460357629,0.0203914906379236,
2.71806455594343));
#30786=CARTESIAN_POINT('Ctrl Pts',(-0.126245549239308,1.45328325776573E-5,
2.71934196736194));
#30787=CARTESIAN_POINT('Origin',(0.,0.,3.1));
#30788=CARTESIAN_POINT('',(-0.126511755116174,-0.000105182036976022,2.76934196736194));
#30789=CARTESIAN_POINT('',(-0.12664039552615,3.66938896950461E-5,2.75565803263806));
#30790=CARTESIAN_POINT('',(-0.12645,1.54856587752183E-17,3.1));
#30791=CARTESIAN_POINT('Ctrl Pts',(-0.12664039552615,3.66938896950461E-5,
2.75565803263806));
#30792=CARTESIAN_POINT('Ctrl Pts',(-0.126647890342436,0.00202721792373194,
2.75553223565232));
#30793=CARTESIAN_POINT('Ctrl Pts',(-0.126604975133189,0.00401740611511355,
2.75540643866659));
#30794=CARTESIAN_POINT('Ctrl Pts',(-0.126510633504476,0.00600514734308786,
2.75528064168085));
#30795=CARTESIAN_POINT('Ctrl Pts',(-0.124536452742414,0.0476003640650105,
2.75264823017224));
#30796=CARTESIAN_POINT('Ctrl Pts',(-0.10004305012127,0.0881240748873803,
2.75001581866363));
#30797=CARTESIAN_POINT('Ctrl Pts',(-0.064133889095878,0.109212690295602,
2.74738340715501));
#30798=CARTESIAN_POINT('Ctrl Pts',(-0.0282247280704852,0.130301305703824,
2.7447509956464));
#30799=CARTESIAN_POINT('Ctrl Pts',(0.0191001913591554,0.131954825697897,
2.74211858413779));
#30800=CARTESIAN_POINT('Ctrl Pts',(0.0563882647159258,0.113411365221879,
2.73948617262918));
#30801=CARTESIAN_POINT('Ctrl Pts',(0.0936763380726957,0.0948679047458623,
2.73685376112057));
#30802=CARTESIAN_POINT('Ctrl Pts',(0.120927565356595,0.0561274637997562,
2.73422134961196));
#30803=CARTESIAN_POINT('Ctrl Pts',(0.125787645771127,0.0147753877020813,
2.73158893810334));
#30804=CARTESIAN_POINT('Ctrl Pts',(0.13064772618566,-0.0265766883955932,
2.72895652659473));
#30805=CARTESIAN_POINT('Ctrl Pts',(0.113116659730824,-0.0705403996448371,
2.72632411508612));
#30806=CARTESIAN_POINT('Ctrl Pts',(0.0811433928446468,-0.0972323182667412,
2.72369170357751));
#30807=CARTESIAN_POINT('Ctrl Pts',(0.0491701259584694,-0.123924236888645,
2.7210592920689));
#30808=CARTESIAN_POINT('Ctrl Pts',(0.00275465864095025,-0.133344362883211,
2.71842688056028));
#30809=CARTESIAN_POINT('Ctrl Pts',(-0.0370665720412133,-0.121131225367919,
2.71579446905167));
#30810=CARTESIAN_POINT('Ctrl Pts',(-0.0768878027233769,-0.108918087852628,
2.71316205754306));
#30811=CARTESIAN_POINT('Ctrl Pts',(-0.110114796770184,-0.0750716868274789,
2.71052964603445));
#30812=CARTESIAN_POINT('Ctrl Pts',(-0.121670218183899,-0.0351354691109218,
2.70789723452584));
#30813=CARTESIAN_POINT('Ctrl Pts',(-0.124946671651124,-0.023811852747613,
2.70715083389658));
#30814=CARTESIAN_POINT('Ctrl Pts',(-0.126480809379052,-0.0119986372375087,
2.70640443326732));
#30815=CARTESIAN_POINT('Ctrl Pts',(-0.126374981062586,-0.000161346902988299,
2.70565803263806));
#30816=CARTESIAN_POINT('Ctrl Pts',(-0.126245549239308,1.45328325776573E-5,
2.71934196736194));
#30817=CARTESIAN_POINT('Ctrl Pts',(-0.126231853912779,-0.0216001006849982,
2.72069696745204));
#30818=CARTESIAN_POINT('Ctrl Pts',(-0.120965346567412,-0.0432228820262939,
2.72205196754215));
#30819=CARTESIAN_POINT('Ctrl Pts',(-0.110486681315658,-0.0619230805928583,
2.72340696763225));
#30820=CARTESIAN_POINT('Ctrl Pts',(-0.0901293697515468,-0.0982526854980795,
2.72603937914086));
#30821=CARTESIAN_POINT('Ctrl Pts',(-0.0501001504896328,-0.123551776820195,
2.72867179064947));
#30822=CARTESIAN_POINT('Ctrl Pts',(-0.00855140384117574,-0.126362344661561,
2.73130420215808));
#30823=CARTESIAN_POINT('Ctrl Pts',(0.0329973428072813,-0.129172912502927,
2.7339366136667));
#30824=CARTESIAN_POINT('Ctrl Pts',(0.076065616842282,-0.109494956863544,
2.73656902517531));
#30825=CARTESIAN_POINT('Ctrl Pts',(0.10113334277539,-0.0762433600374486,
2.73920143668392));
#30826=CARTESIAN_POINT('Ctrl Pts',(0.126201068708497,-0.0429917632113539,
2.74183384819253));
#30827=CARTESIAN_POINT('Ctrl Pts',(0.133268246539712,0.00383347480145232,
2.74446625970114));
#30828=CARTESIAN_POINT('Ctrl Pts',(0.119129452671912,0.0430029706396828,
2.74709867120975));
#30829=CARTESIAN_POINT('Ctrl Pts',(0.104990658804112,0.0821724664779139,
2.74973108271837));
#30830=CARTESIAN_POINT('Ctrl Pts',(0.0696458932372969,0.113686220141568,
2.75236349422698));
#30831=CARTESIAN_POINT('Ctrl Pts',(0.0291183743037611,0.123260050517998,
2.75499590573559));
#30832=CARTESIAN_POINT('Ctrl Pts',(-0.0114091446297752,0.132833880894428,
2.7576283172442));
#30833=CARTESIAN_POINT('Ctrl Pts',(-0.0571194169300318,0.120467787983633,
2.76026072875281));
#30834=CARTESIAN_POINT('Ctrl Pts',(-0.0872917850925406,0.0917667415677358,
2.76289314026143));
#30835=CARTESIAN_POINT('Ctrl Pts',(-0.111930332277198,0.0683296655464438,
2.76504274929493));
#30836=CARTESIAN_POINT('Ctrl Pts',(-0.126207827945274,0.0340000461494869,
2.76719235832844));
#30837=CARTESIAN_POINT('Ctrl Pts',(-0.126511755116174,-0.000105182036976022,
2.76934196736194));
#30838=CARTESIAN_POINT('Origin',(0.,0.,3.1));
#30839=CARTESIAN_POINT('',(-0.126553655479795,9.34644642624216E-5,2.81934196736194));
#30840=CARTESIAN_POINT('',(-0.126295222915983,7.47437243418914E-5,2.80565803263806));
#30841=CARTESIAN_POINT('',(-0.12645,1.54856587752183E-17,3.1));
#30842=CARTESIAN_POINT('Ctrl Pts',(-0.126295222915983,7.47437243418914E-5,
2.80565803263806));
#30843=CARTESIAN_POINT('Ctrl Pts',(-0.126381902901803,0.0159778826374278,
2.80466003803733));
#30844=CARTESIAN_POINT('Ctrl Pts',(-0.12359488800886,0.0318517555514631,
2.8036620434366));
#30845=CARTESIAN_POINT('Ctrl Pts',(-0.117794192788123,0.0465350551086,2.80266404883586));
#30846=CARTESIAN_POINT('Ctrl Pts',(-0.102493692318657,0.0852652112740412,
2.80003163732725));
#30847=CARTESIAN_POINT('Ctrl Pts',(-0.0662256093040858,0.115711992156929,
2.79739922581864));
#30848=CARTESIAN_POINT('Ctrl Pts',(-0.0254308011719313,0.124073552736451,
2.79476681431003));
#30849=CARTESIAN_POINT('Ctrl Pts',(0.0153640069602226,0.132435113315973,
2.79213440280142));
#30850=CARTESIAN_POINT('Ctrl Pts',(0.0606855402099605,0.11871145359213,
2.78950199129281));
#30851=CARTESIAN_POINT('Ctrl Pts',(0.089988893871543,0.0891234665506248,
2.78686957978419));
#30852=CARTESIAN_POINT('Ctrl Pts',(0.119292247533126,0.0595354795091193,
2.78423716827558));
#30853=CARTESIAN_POINT('Ctrl Pts',(0.132577421606553,0.0140831651499525,
2.78160475676697));
#30854=CARTESIAN_POINT('Ctrl Pts',(0.123822034418855,-0.0266288104888323,
2.77897234525835));
#30855=CARTESIAN_POINT('Ctrl Pts',(0.115066647231157,-0.067340786127616,
2.77633993374974));
#30856=CARTESIAN_POINT('Ctrl Pts',(0.084270698782333,-0.103312423046018,
2.77370752224113));
#30857=CARTESIAN_POINT('Ctrl Pts',(0.045394477490254,-0.11823815061478,
2.77107511073252));
#30858=CARTESIAN_POINT('Ctrl Pts',(0.00651825619817509,-0.133163878183541,
2.76844269922391));
#30859=CARTESIAN_POINT('Ctrl Pts',(-0.0404382379371578,-0.127043696402664,
2.7658102877153));
#30860=CARTESIAN_POINT('Ctrl Pts',(-0.0741890055533361,-0.102650244201489,
2.76317787620668));
#30861=CARTESIAN_POINT('Ctrl Pts',(-0.106326900403039,-0.0794224998497761,
2.76067126168381));
#30862=CARTESIAN_POINT('Ctrl Pts',(-0.126491054782899,-0.0396262314391609,
2.75816464716093));
#30863=CARTESIAN_POINT('Ctrl Pts',(-0.12664039552615,3.66938896950461E-5,
2.75565803263806));
#30864=CARTESIAN_POINT('Ctrl Pts',(-0.126511755116174,-0.000105182036976022,
2.76934196736194));
#30865=CARTESIAN_POINT('Ctrl Pts',(-0.12658001719922,-0.00776522082814862,
2.76982476983705));
#30866=CARTESIAN_POINT('Ctrl Pts',(-0.125943379547996,-0.015413940155386,
2.77030757231215));
#30867=CARTESIAN_POINT('Ctrl Pts',(-0.124560912333973,-0.022925385115547,
2.77079037478726));
#30868=CARTESIAN_POINT('Ctrl Pts',(-0.117023207388135,-0.0638804654619373,
2.77342278629587));
#30869=CARTESIAN_POINT('Ctrl Pts',(-0.0873133334716985,-0.100754626233721,
2.77605519780449));
#30870=CARTESIAN_POINT('Ctrl Pts',(-0.0488993400374831,-0.116832476461904,
2.7786876093131));
#30871=CARTESIAN_POINT('Ctrl Pts',(-0.0104853466032667,-0.132910326690088,
2.78132002082171));
#30872=CARTESIAN_POINT('Ctrl Pts',(0.0366327663487292,-0.128191866374669,
2.78395243233032));
#30873=CARTESIAN_POINT('Ctrl Pts',(0.0710957359713387,-0.104815935790865,
2.78658484383893));
#30874=CARTESIAN_POINT('Ctrl Pts',(0.105558705593947,-0.0814400052070627,
2.78921725534754));
#30875=CARTESIAN_POINT('Ctrl Pts',(0.12736653188717,-0.0394066043548766,
2.79184966685616));
#30876=CARTESIAN_POINT('Ctrl Pts',(0.126633373335447,0.00222985575585417,
2.79448207836477));
#30877=CARTESIAN_POINT('Ctrl Pts',(0.125900214783723,0.0438663158665862,
2.79711448987338));
#30878=CARTESIAN_POINT('Ctrl Pts',(0.102626071387052,0.0851058352358628,
2.79974690138199));
#30879=CARTESIAN_POINT('Ctrl Pts',(0.067361470922124,0.107253965297467,
2.8023793128906));
#30880=CARTESIAN_POINT('Ctrl Pts',(0.032096870457197,0.12940209535907,2.80501172439922));
#30881=CARTESIAN_POINT('Ctrl Pts',(-0.0151581870759861,0.132458836113002,
2.80764413590783));
#30882=CARTESIAN_POINT('Ctrl Pts',(-0.052982302223486,0.115038507268346,
2.81027654741644));
#30883=CARTESIAN_POINT('Ctrl Pts',(-0.0908064173709864,0.0976181784236899,
2.81290895892505));
#30884=CARTESIAN_POINT('Ctrl Pts',(-0.119199590132803,0.059720779980445,
2.81554137043366));
#30885=CARTESIAN_POINT('Ctrl Pts',(-0.12529077505034,0.0185257648347912,
2.81817378194227));
#30886=CARTESIAN_POINT('Ctrl Pts',(-0.126191803554164,0.0124320600196876,
2.81856317708216));
#30887=CARTESIAN_POINT('Ctrl Pts',(-0.126604835154177,0.00626619900254654,
2.81895257222205));
#30888=CARTESIAN_POINT('Ctrl Pts',(-0.126553655479795,9.34644642624216E-5,
2.81934196736194));
#30889=CARTESIAN_POINT('Origin',(0.,0.,3.1));
#30890=CARTESIAN_POINT('',(-0.126249156657861,1.39511119994357E-5,2.86934196736194));
#30891=CARTESIAN_POINT('',(-0.126382098607383,-0.000107526861324363,2.85565803263806));
#30892=CARTESIAN_POINT('',(-0.12645,1.54856587752183E-17,3.1));
#30893=CARTESIAN_POINT('Ctrl Pts',(-0.126382098607383,-0.000107526861324363,
2.85565803263806));
#30894=CARTESIAN_POINT('Ctrl Pts',(-0.126136963881609,0.0296424659657165,
2.85378784042233));
#30895=CARTESIAN_POINT('Ctrl Pts',(-0.115629819550324,0.0595483512746711,
2.8519176482066));
#30896=CARTESIAN_POINT('Ctrl Pts',(-0.0964566207792818,0.0820798491866498,
2.85004745599088));
#30897=CARTESIAN_POINT('Ctrl Pts',(-0.0694691546368386,0.113794329607957,
2.84741504448226));
#30898=CARTESIAN_POINT('Ctrl Pts',(-0.0253122344935349,0.130898446561428,
2.84478263297365));
#30899=CARTESIAN_POINT('Ctrl Pts',(0.0159971616939493,0.125638656106515,
2.84215022146504));
#30900=CARTESIAN_POINT('Ctrl Pts',(0.0573065578814334,0.120378865651602,
2.83951780995643));
#30901=CARTESIAN_POINT('Ctrl Pts',(0.0957684301130981,0.0927551677883048,
2.83688539844782));
#30902=CARTESIAN_POINT('Ctrl Pts',(0.113947449240963,0.0552897840743664,
2.83425298693921));
#30903=CARTESIAN_POINT('Ctrl Pts',(0.132126468368828,0.017824400360428,
2.83162057543059));
#30904=CARTESIAN_POINT('Ctrl Pts',(0.130022634392893,-0.0294826692041511,
2.82898816392198));
#30905=CARTESIAN_POINT('Ctrl Pts',(0.108589645677727,-0.0651864287383833,
2.82635575241337));
#30906=CARTESIAN_POINT('Ctrl Pts',(0.0871566569625619,-0.100890188272616,
2.82372334090476));
#30907=CARTESIAN_POINT('Ctrl Pts',(0.0463945135081664,-0.124990637776501,
2.82109092939615));
#30908=CARTESIAN_POINT('Ctrl Pts',(0.00478129192095443,-0.126562708640517,
2.81845851788753));
#30909=CARTESIAN_POINT('Ctrl Pts',(-0.036831929666257,-0.128134779504533,
2.81582610637892));
#30910=CARTESIAN_POINT('Ctrl Pts',(-0.0792962293862848,-0.10717847172868,
2.81319369487031));
#30911=CARTESIAN_POINT('Ctrl Pts',(-0.103361920284118,-0.0731935521167569,
2.8105612833617));
#30912=CARTESIAN_POINT('Ctrl Pts',(-0.118303874448411,-0.0520929274442991,
2.80892686645382));
#30913=CARTESIAN_POINT('Ctrl Pts',(-0.126153267003299,-0.0259698452031535,
2.80729244954594));
#30914=CARTESIAN_POINT('Ctrl Pts',(-0.126295222915983,7.47437243418914E-5,
2.80565803263806));
#30915=CARTESIAN_POINT('Ctrl Pts',(-0.126553655479795,9.34644642624216E-5,
2.81934196736194));
#30916=CARTESIAN_POINT('Ctrl Pts',(-0.126258847364269,-0.0354630774409815,
2.82158498373066));
#30917=CARTESIAN_POINT('Ctrl Pts',(-0.110561244917173,-0.0712476866904275,
2.82382800009939));
#30918=CARTESIAN_POINT('Ctrl Pts',(-0.0840069629213228,-0.0947829738698732,
2.82607101646811));
#30919=CARTESIAN_POINT('Ctrl Pts',(-0.0528427688015115,-0.122404065580821,
2.82870342797672));
#30920=CARTESIAN_POINT('Ctrl Pts',(-0.00672518348863185,-0.133153617154654,
2.83133583948533));
#30921=CARTESIAN_POINT('Ctrl Pts',(0.0334400182730099,-0.122158697506542,
2.83396825099395));
#30922=CARTESIAN_POINT('Ctrl Pts',(0.0736052200346521,-0.111163777858429,
2.83660066250256));
#30923=CARTESIAN_POINT('Ctrl Pts',(0.107818038245057,-0.0784243869883676,
2.83923307401117));
#30924=CARTESIAN_POINT('Ctrl Pts',(0.120569301232658,-0.0387817708073496,
2.84186548551978));
#30925=CARTESIAN_POINT('Ctrl Pts',(0.13332056422026,0.000860845373668366,
2.84449789702839));
#30926=CARTESIAN_POINT('Ctrl Pts',(0.124610271985061,0.0474066868656423,
2.847130308537));
#30927=CARTESIAN_POINT('Ctrl Pts',(0.0983869277745218,0.0797558433812344,
2.84976272004562));
#30928=CARTESIAN_POINT('Ctrl Pts',(0.0721635835639831,0.112104999896826,
2.85239513155423));
#30929=CARTESIAN_POINT('Ctrl Pts',(0.0284271873781034,0.130257471436035,
2.85502754306284));
#30930=CARTESIAN_POINT('Ctrl Pts',(-0.0129959127687897,0.125984476806968,
2.85765995457145));
#30931=CARTESIAN_POINT('Ctrl Pts',(-0.0544190129156822,0.121711482177902,
2.86029236608007));
#30932=CARTESIAN_POINT('Ctrl Pts',(-0.0935288170235893,0.0950130213805616,
2.86292477758868));
#30933=CARTESIAN_POINT('Ctrl Pts',(-0.11259627866674,0.0579918974128127,
2.86555718909729));
#30934=CARTESIAN_POINT('Ctrl Pts',(-0.121734428756244,0.0402493895934286,
2.86681878185217));
#30935=CARTESIAN_POINT('Ctrl Pts',(-0.126269172738684,0.0201359308353815,
2.86808037460706));
#30936=CARTESIAN_POINT('Ctrl Pts',(-0.126249156657861,1.39511119994357E-5,
2.86934196736194));
#30937=CARTESIAN_POINT('Origin',(0.,0.,3.1));
#30938=CARTESIAN_POINT('',(-0.126504381589359,-0.000106615302056266,2.91934196736194));
#30939=CARTESIAN_POINT('',(-0.126643227510109,3.12951648517141E-5,2.90565803263806));
#30940=CARTESIAN_POINT('',(-0.12645,1.54856587752183E-17,3.1));
#30941=CARTESIAN_POINT('Ctrl Pts',(-0.126643227510109,3.12951648517141E-5,
2.90565803263806));
#30942=CARTESIAN_POINT('Ctrl Pts',(-0.126649060558016,0.00177143581201147,
2.90554805431595));
#30943=CARTESIAN_POINT('Ctrl Pts',(-0.126616264808321,0.00351135171962892,
2.90543807599384));
#30944=CARTESIAN_POINT('Ctrl Pts',(-0.126544152713349,0.00524963660346066,
2.90532809767173));
#30945=CARTESIAN_POINT('Ctrl Pts',(-0.124818097022822,0.0468567555849086,
2.90269568616312));
#30946=CARTESIAN_POINT('Ctrl Pts',(-0.100566951953931,0.0875294297116145,
2.9000632746545));
#30947=CARTESIAN_POINT('Ctrl Pts',(-0.0647841163292417,0.1088301407863,
2.89743086314589));
#30948=CARTESIAN_POINT('Ctrl Pts',(-0.0290012807045523,0.130130851860986,
2.89479845163728));
#30949=CARTESIAN_POINT('Ctrl Pts',(0.0183132454759347,0.13205959988365,
2.89216604012867));
#30950=CARTESIAN_POINT('Ctrl Pts',(0.0557110953405879,0.113742055209456,
2.88953362862006));
#30951=CARTESIAN_POINT('Ctrl Pts',(0.0931089452052417,0.0954245105352619,
2.88690121711144));
#30952=CARTESIAN_POINT('Ctrl Pts',(0.120590118754061,0.0568606731642085,
2.88426880560283));
#30953=CARTESIAN_POINT('Ctrl Pts',(0.125696998005905,0.0155320946228576,
2.88163639409422));
#30954=CARTESIAN_POINT('Ctrl Pts',(0.130803877257748,-0.025796483918492,
2.87900398258561));
#30955=CARTESIAN_POINT('Ctrl Pts',(0.113536462212617,-0.0698898036301388,
2.87637157107699));
#30956=CARTESIAN_POINT('Ctrl Pts',(0.081722324704119,-0.0967597174754642,
2.87373915956838));
#30957=CARTESIAN_POINT('Ctrl Pts',(0.0499081871956208,-0.12362963132079,
2.87110674805977));
#30958=CARTESIAN_POINT('Ctrl Pts',(0.0035473272237559,-0.133276139299794,
2.86847433655116));
#30959=CARTESIAN_POINT('Ctrl Pts',(-0.0363441991716402,-0.12132633857832,
2.86584192504255));
#30960=CARTESIAN_POINT('Ctrl Pts',(-0.0762357255670363,-0.109376537856846,
2.86320951353394));
#30961=CARTESIAN_POINT('Ctrl Pts',(-0.109657918385963,-0.0758304284348936,
2.86057710202533));
#30962=CARTESIAN_POINT('Ctrl Pts',(-0.121460008724635,-0.035894951779346,
2.85794469051671));
#30963=CARTESIAN_POINT('Ctrl Pts',(-0.124877324339263,-0.0243315656302484,
2.85718247122383));
#30964=CARTESIAN_POINT('Ctrl Pts',(-0.126482006208201,-0.0122324936456281,
2.85642025193094));
#30965=CARTESIAN_POINT('Ctrl Pts',(-0.126382098607383,-0.000107526861324363,
2.85565803263806));
#30966=CARTESIAN_POINT('Ctrl Pts',(-0.126249156657861,1.39511119994357E-5,
2.86934196736194));
#30967=CARTESIAN_POINT('Ctrl Pts',(-0.126227407627626,-0.0218501465218449,
2.87071278611567));
#30968=CARTESIAN_POINT('Ctrl Pts',(-0.120828074559444,-0.0437243044457016,
2.8720836048694));
#30969=CARTESIAN_POINT('Ctrl Pts',(-0.110113563989691,-0.0625778327914941,
2.87345442362312));
#30970=CARTESIAN_POINT('Ctrl Pts',(-0.0895382684910942,-0.0987826518898959,
2.87608683513174));
#30971=CARTESIAN_POINT('Ctrl Pts',(-0.049362558315506,-0.12384850294854,
2.87871924664035));
#30972=CARTESIAN_POINT('Ctrl Pts',(-0.00779867057972899,-0.126412668959158,
2.88135165814896));
#30973=CARTESIAN_POINT('Ctrl Pts',(0.0337652171560469,-0.128976834969775,
2.88398406965757));
#30974=CARTESIAN_POINT('Ctrl Pts',(0.0767172824520115,-0.109039315932365,
2.88661648116618));
#30975=CARTESIAN_POINT('Ctrl Pts',(0.101586725761179,-0.0756380809090063,
2.88924889267479));
#30976=CARTESIAN_POINT('Ctrl Pts',(0.126456169070347,-0.0422368458856463,
2.89188130418341));
#30977=CARTESIAN_POINT('Ctrl Pts',(0.133242990392717,0.00462810512366429,
2.89451371569202));
#30978=CARTESIAN_POINT('Ctrl Pts',(0.118870624347205,0.0437122042621813,
2.89714612720063));
#30979=CARTESIAN_POINT('Ctrl Pts',(0.104498258301693,0.0827963034006972,
2.89977853870924));
#30980=CARTESIAN_POINT('Ctrl Pts',(0.0689667048882996,0.11409955066842,
2.90241095021785));
#30981=CARTESIAN_POINT('Ctrl Pts',(0.0283829370476986,0.123431726145854,
2.90504336172646));
#30982=CARTESIAN_POINT('Ctrl Pts',(-0.0122008307929037,0.132763901623287,
2.90767577323508));
#30983=CARTESIAN_POINT('Ctrl Pts',(-0.0578368130607139,0.120125005310431,
2.91030818474369));
#30984=CARTESIAN_POINT('Ctrl Pts',(-0.0878375513946906,0.0912444338001155,
2.9129405962523));
#30985=CARTESIAN_POINT('Ctrl Pts',(-0.112155666680576,0.0678343076994951,
2.91507438662218));
#30986=CARTESIAN_POINT('Ctrl Pts',(-0.126200703597521,0.0337526498432798,
2.91720817699206));
#30987=CARTESIAN_POINT('Ctrl Pts',(-0.126504381589359,-0.000106615302056266,
2.91934196736194));
#30988=CARTESIAN_POINT('Origin',(0.,0.,3.1));
#30989=CARTESIAN_POINT('',(-0.126560384998288,9.09688539718206E-5,2.96934196736194));
#30990=CARTESIAN_POINT('',(-0.126299886768127,7.7729991388234E-5,2.95565803263806));
#30991=CARTESIAN_POINT('',(-0.12645,1.54856587752183E-17,3.1));
#30992=CARTESIAN_POINT('Ctrl Pts',(-0.126299886768127,7.7729991388234E-5,
2.95565803263806));
#30993=CARTESIAN_POINT('Ctrl Pts',(-0.126388830708229,0.0157273402429332,
2.95467585670095));
#30994=CARTESIAN_POINT('Ctrl Pts',(-0.123692081773928,0.0313473916688532,
2.95369368076385));
#30995=CARTESIAN_POINT('Ctrl Pts',(-0.118069607334697,0.0458317476680533,
2.95271150482674));
#30996=CARTESIAN_POINT('Ctrl Pts',(-0.103000345442256,0.0846524762021514,
2.95007909331813));
#30997=CARTESIAN_POINT('Ctrl Pts',(-0.066914478664464,0.115315070279254,
2.94744668180952));
#30998=CARTESIAN_POINT('Ctrl Pts',(-0.0261702583026162,0.123919727448441,
2.9448142703009));
#30999=CARTESIAN_POINT('Ctrl Pts',(0.0145739620592316,0.132524384617628,
2.94218185879229));
#31000=CARTESIAN_POINT('Ctrl Pts',(0.0599765360051347,0.119071104878899,
2.93954944728368));
#31001=CARTESIAN_POINT('Ctrl Pts',(0.0894558125827043,0.0896584567433833,
2.93691703577507));
#31002=CARTESIAN_POINT('Ctrl Pts',(0.118935089160275,0.0602458086078669,
2.93428462426646));
#31003=CARTESIAN_POINT('Ctrl Pts',(0.13249106836951,0.0148737920755634,
2.93165221275785));
#31004=CARTESIAN_POINT('Ctrl Pts',(0.123978626527973,-0.0258897940256335,
2.92901980124923));
#31005=CARTESIAN_POINT('Ctrl Pts',(0.115466184686436,-0.0666533801268299,
2.92638738974062));
#31006=CARTESIAN_POINT('Ctrl Pts',(0.0848853217941264,-0.10280853579692,
2.92375497823201));
#31007=CARTESIAN_POINT('Ctrl Pts',(0.0460987903596358,-0.117965600062524,
2.9211225667234));
#31008=CARTESIAN_POINT('Ctrl Pts',(0.00731225892514568,-0.133122664328129,
2.91849015521479));
#31009=CARTESIAN_POINT('Ctrl Pts',(-0.0396799410515272,-0.127281637189249,
2.91585774370617));
#31010=CARTESIAN_POINT('Ctrl Pts',(-0.0735755578837821,-0.103090341701714,
2.91322533219756));
#31011=CARTESIAN_POINT('Ctrl Pts',(-0.106055065170122,-0.0799097233361643,
2.91070289901106));
#31012=CARTESIAN_POINT('Ctrl Pts',(-0.126509442293762,-0.0398801022208299,
2.90818046582456));
#31013=CARTESIAN_POINT('Ctrl Pts',(-0.126643227510109,3.12951648517141E-5,
2.90565803263806));
#31014=CARTESIAN_POINT('Ctrl Pts',(-0.126504381589359,-0.000106615302056266,
2.91934196736194));
#31015=CARTESIAN_POINT('Ctrl Pts',(-0.126575344636262,-0.00801880085773389,
2.91984058850067));
#31016=CARTESIAN_POINT('Ctrl Pts',(-0.125895951346516,-0.0159188425067759,
2.9203392096394));
#31017=CARTESIAN_POINT('Ctrl Pts',(-0.124421945835367,-0.0236677318103004,
2.92083783077814));
#31018=CARTESIAN_POINT('Ctrl Pts',(-0.116640107541925,-0.0645770792026294,
2.92347024228675));
#31019=CARTESIAN_POINT('Ctrl Pts',(-0.0867109365548968,-0.101273527279515,
2.92610265379536));
#31020=CARTESIAN_POINT('Ctrl Pts',(-0.0482017639084,-0.117122039303909,
2.92873506530397));
#31021=CARTESIAN_POINT('Ctrl Pts',(-0.0096925912619021,-0.132970551328304,
2.93136747681259));
#31022=CARTESIAN_POINT('Ctrl Pts',(0.0373965830440653,-0.127971127300206,
2.9339998883212));
#31023=CARTESIAN_POINT('Ctrl Pts',(0.071719547440819,-0.104390079267275,
2.93663229982981));
#31024=CARTESIAN_POINT('Ctrl Pts',(0.106042511837572,-0.0808090312343449,
2.93926471133842));
#31025=CARTESIAN_POINT('Ctrl Pts',(0.127599266325111,-0.0386463591965834,
2.94189712284703));
#31026=CARTESIAN_POINT('Ctrl Pts',(0.126617818746111,0.00298498082453686,
2.94452953435564));
#31027=CARTESIAN_POINT('Ctrl Pts',(0.125636371167111,0.0446163208456583,
2.94716194586426));
#31028=CARTESIAN_POINT('Ctrl Pts',(0.10211672152157,0.0857163288501385,
2.94979435737287));
#31029=CARTESIAN_POINT('Ctrl Pts',(0.0667206710566959,0.107653769967896,
2.95242676888148));
#31030=CARTESIAN_POINT('Ctrl Pts',(0.0313246205918224,0.129591211085654,
2.95505918039009));
#31031=CARTESIAN_POINT('Ctrl Pts',(-0.0159478306923833,0.13236608531669,
2.9576915918987));
#31032=CARTESIAN_POINT('Ctrl Pts',(-0.0536673890921198,0.114720501579208,
2.96032400340732));
#31033=CARTESIAN_POINT('Ctrl Pts',(-0.0913869474918552,0.0970749178417258,
2.96295641491593));
#31034=CARTESIAN_POINT('Ctrl Pts',(-0.119553613007122,0.059008876135727,
2.96558882642454));
#31035=CARTESIAN_POINT('Ctrl Pts',(-0.125399024116903,0.0177782700249248,
2.96822123793315));
#31036=CARTESIAN_POINT('Ctrl Pts',(-0.12622857074271,0.0119270630632909,
2.96859481440941));
#31037=CARTESIAN_POINT('Ctrl Pts',(-0.126608575570408,0.00601212294639071,
2.96896839088568));
#31038=CARTESIAN_POINT('Ctrl Pts',(-0.126560384998288,9.09688539718206E-5,
2.96934196736194));
#31039=CARTESIAN_POINT('Origin',(0.,0.,3.1));
#31040=CARTESIAN_POINT('',(-0.126250113253048,1.79623087654263E-5,3.01934196736194));
#31041=CARTESIAN_POINT('',(-0.126375290424941,-0.000106230050797054,3.00565803263806));
#31042=CARTESIAN_POINT('',(-0.12645,1.54856587752183E-17,3.1));
#31043=CARTESIAN_POINT('Ctrl Pts',(-0.126375290424941,-0.000106230050797054,
3.00565803263806));
#31044=CARTESIAN_POINT('Ctrl Pts',(-0.126136144258534,0.0293961593132966,
3.00380365908596));
#31045=CARTESIAN_POINT('Ctrl Pts',(-0.115821844223656,0.0590492800488679,
3.00194928553385));
#31046=CARTESIAN_POINT('Ctrl Pts',(-0.0969443855366137,0.0815031740695626,
3.00009491198175));
#31047=CARTESIAN_POINT('Ctrl Pts',(-0.0701465273355013,0.11337802957871,
2.99746250047314));
#31048=CARTESIAN_POINT('Ctrl Pts',(-0.0260923921578653,0.130745171841498,
2.99483008896453));
#31049=CARTESIAN_POINT('Ctrl Pts',(0.0152476360635642,0.125731821210699,
2.99219767745592));
#31050=CARTESIAN_POINT('Ctrl Pts',(0.0565876642849942,0.120718470579899,
2.98956526594731));
#31051=CARTESIAN_POINT('Ctrl Pts',(0.0952135855502181,0.0933246270555131,
2.98693285443869));
#31052=CARTESIAN_POINT('Ctrl Pts',(0.113615704700958,0.0559683206447137,
2.98430044293008));
#31053=CARTESIAN_POINT('Ctrl Pts',(0.132017823851697,0.0186120142339143,
2.98166803142147));
#31054=CARTESIAN_POINT('Ctrl Pts',(0.130196140887953,-0.0287067550632971,
2.97903561991286));
#31055=CARTESIAN_POINT('Ctrl Pts',(0.108976451346127,-0.0645376969103253,
2.97640320840425));
#31056=CARTESIAN_POINT('Ctrl Pts',(0.0877567618043009,-0.100368638757354,
2.97377079689564));
#31057=CARTESIAN_POINT('Ctrl Pts',(0.0471390656843917,-0.124711753154198,
2.97113838538702));
#31058=CARTESIAN_POINT('Ctrl Pts',(0.00553595882347027,-0.126531950235485,
2.96850597387841));
#31059=CARTESIAN_POINT('Ctrl Pts',(-0.03606714803745,-0.128352147316772,
2.9658735623698));
#31060=CARTESIAN_POINT('Ctrl Pts',(-0.078655665639383,-0.107649427082503,
2.96324115086119));
#31061=CARTESIAN_POINT('Ctrl Pts',(-0.102923595936805,-0.0738086354698221,
2.96060873935258));
#31062=CARTESIAN_POINT('Ctrl Pts',(-0.118136947531953,-0.0525941414955858,
2.95895850378107));
#31063=CARTESIAN_POINT('Ctrl Pts',(-0.126150444648563,-0.0262164832362216,
2.95730826820956));
#31064=CARTESIAN_POINT('Ctrl Pts',(-0.126299886768127,7.7729991388234E-5,
2.95565803263806));
#31065=CARTESIAN_POINT('Ctrl Pts',(-0.126560384998288,9.09688539718206E-5,
2.96934196736194));
#31066=CARTESIAN_POINT('Ctrl Pts',(-0.126269000075926,-0.0357113665330736,
2.97160080239429));
#31067=CARTESIAN_POINT('Ctrl Pts',(-0.110322654377183,-0.0717408868526332,
2.97385963742664));
#31068=CARTESIAN_POINT('Ctrl Pts',(-0.0834402350166293,-0.0952822612815302,
2.97611847245899));
#31069=CARTESIAN_POINT('Ctrl Pts',(-0.0521118781022804,-0.122717015961572,
2.9787508839676));
#31070=CARTESIAN_POINT('Ctrl Pts',(-0.00593100756928766,-0.133191354806051,
2.98138329547621));
#31071=CARTESIAN_POINT('Ctrl Pts',(0.0341679124015605,-0.12195710679034,
2.98401570698482));
#31072=CARTESIAN_POINT('Ctrl Pts',(0.0742668323724097,-0.110722858774629,
2.98664811849343));
#31073=CARTESIAN_POINT('Ctrl Pts',(0.108283801781115,-0.0777800238987277,
2.98928053000205));
#31074=CARTESIAN_POINT('Ctrl Pts',(0.120798430769142,-0.038062071124208,
2.99191294151066));
#31075=CARTESIAN_POINT('Ctrl Pts',(0.133313059757168,0.00165588165031116,
2.99454535301927));
#31076=CARTESIAN_POINT('Ctrl Pts',(0.124325348324518,0.0481489523234473,
2.99717776452788));
#31077=CARTESIAN_POINT('Ctrl Pts',(0.0979095575425482,0.0803411518237943,
2.9998101760365));
#31078=CARTESIAN_POINT('Ctrl Pts',(0.0714937667605778,0.112533351324142,
3.00244258754511));
#31079=CARTESIAN_POINT('Ctrl Pts',(0.0276498966292865,0.130424679651699,
3.00507499905372));
#31080=CARTESIAN_POINT('Ctrl Pts',(-0.0137469851400152,0.125904735947905,
3.00770741056233));
#31081=CARTESIAN_POINT('Ctrl Pts',(-0.0551438669093158,0.121384792244111,
3.01033982207094));
#31082=CARTESIAN_POINT('Ctrl Pts',(-0.0940937603166274,0.0944535765089676,
3.01297223357955));
#31083=CARTESIAN_POINT('Ctrl Pts',(-0.112940108892359,0.0573194028051013,
3.01560464508816));
#31084=CARTESIAN_POINT('Ctrl Pts',(-0.121859038434214,0.039745861833548,
3.01685041917942));
#31085=CARTESIAN_POINT('Ctrl Pts',(-0.126275572181929,0.0198872634041666,
3.01809619327068));
#31086=CARTESIAN_POINT('Ctrl Pts',(-0.126250113253048,1.79623087654263E-5,
3.01934196736194));
#31087=CARTESIAN_POINT('Origin',(0.,0.,3.1));
#31088=CARTESIAN_POINT('',(-0.126496969333234,-0.000107906771987382,3.06934196736194));
#31089=CARTESIAN_POINT('',(-0.126645757366777,2.69067085927681E-5,3.05565803263806));
#31090=CARTESIAN_POINT('',(-0.12645,1.54856587752183E-17,3.1));
#31091=CARTESIAN_POINT('Ctrl Pts',(-0.126645757366777,2.69067085927681E-5,
3.05565803263806));
#31092=CARTESIAN_POINT('Ctrl Pts',(-0.126650109530876,0.00151667558283516,
3.05556387297957));
#31093=CARTESIAN_POINT('Ctrl Pts',(-0.126626072178,0.00300630074643505,
3.05546971332109));
#31094=CARTESIAN_POINT('Ctrl Pts',(-0.126573208557277,0.0044949022237674,
3.0553755536626));
#31095=CARTESIAN_POINT('Ctrl Pts',(-0.125095305962741,0.0461115746257868,
3.05274314215399));
#31096=CARTESIAN_POINT('Ctrl Pts',(-0.10108714199637,0.0869281462553232,
3.05011073064538));
#31097=CARTESIAN_POINT('Ctrl Pts',(-0.0654319685934297,0.108441868097491,
3.04747831913677));
#31098=CARTESIAN_POINT('Ctrl Pts',(-0.0297767951904896,0.129955589939659,
3.04484590762816));
#31099=CARTESIAN_POINT('Ctrl Pts',(0.0175253876490204,0.132166461994459,
3.04221349611954));
#31100=CARTESIAN_POINT('Ctrl Pts',(0.0550318084723819,0.114072263617167,
3.03958108461093));
#31101=CARTESIAN_POINT('Ctrl Pts',(0.092538229295744,0.095978065239874,
3.03694867310232));
#31102=CARTESIAN_POINT('Ctrl Pts',(0.120248888102957,0.0575787964304887,
3.03431626159371));
#31103=CARTESIAN_POINT('Ctrl Pts',(0.125602137884551,0.0162814074734155,
3.0316838500851));
#31104=CARTESIAN_POINT('Ctrl Pts',(0.130955387666146,-0.0250159814836577,
3.02905143857648));
#31105=CARTESIAN_POINT('Ctrl Pts',(0.113951228422121,-0.0692114905884188,
3.02641902706787));
#31106=CARTESIAN_POINT('Ctrl Pts',(0.0822978942873024,-0.0962706490388489,
3.02378661555926));
#31107=CARTESIAN_POINT('Ctrl Pts',(0.0506445601524839,-0.123329807489279,
3.02115420405065));
#31108=CARTESIAN_POINT('Ctrl Pts',(0.00434205112687179,-0.133252615285378,
3.01852179254204));
#31109=CARTESIAN_POINT('Ctrl Pts',(-0.0356200281006283,-0.121540918494949,
3.01588938103343));
#31110=CARTESIAN_POINT('Ctrl Pts',(-0.0755821073281284,-0.10982922170452,
3.01325696952481));
#31111=CARTESIAN_POINT('Ctrl Pts',(-0.109203756757516,-0.0764830203275614,
3.0106245580162));
#31112=CARTESIAN_POINT('Ctrl Pts',(-0.121243790859916,-0.0366186352613279,
3.00799214650759));
#31113=CARTESIAN_POINT('Ctrl Pts',(-0.124802354366684,-0.0248362810993748,
3.00721410855108));
#31114=CARTESIAN_POINT('Ctrl Pts',(-0.126475628781476,-0.012484522820876,
3.00643607059457));
#31115=CARTESIAN_POINT('Ctrl Pts',(-0.126375290424941,-0.000106230050797054,
3.00565803263806));
#31116=CARTESIAN_POINT('Ctrl Pts',(-0.126250113253048,1.79623087654263E-5,
3.01934196736194));
#31117=CARTESIAN_POINT('Ctrl Pts',(-0.126221775608494,-0.0220980188702133,
3.0207286047793));
#31118=CARTESIAN_POINT('Ctrl Pts',(-0.120690113995694,-0.0442272599176159,
3.02211524219665));
#31119=CARTESIAN_POINT('Ctrl Pts',(-0.109738425578795,-0.063233377942656,
3.023501879614));
#31120=CARTESIAN_POINT('Ctrl Pts',(-0.0889475899453455,-0.0993148533139586,
3.02613429112261));
#31121=CARTESIAN_POINT('Ctrl Pts',(-0.0486231149342947,-0.124140672383972,
3.02876670263122));
#31122=CARTESIAN_POINT('Ctrl Pts',(-0.00704467496461261,-0.126456928197685,
3.03139911413984));
#31123=CARTESIAN_POINT('Ctrl Pts',(0.0345337650050683,-0.128773184011397,
3.03403152564845));
#31124=CARTESIAN_POINT('Ctrl Pts',(0.0773661699333803,-0.108579876568808,
3.03666393715706));
#31125=CARTESIAN_POINT('Ctrl Pts',(0.102035984081992,-0.0750309275363891,
3.03929634866567));
#31126=CARTESIAN_POINT('Ctrl Pts',(0.126705798230605,-0.0414819785039689,
3.04192876017428));
#31127=CARTESIAN_POINT('Ctrl Pts',(0.133213021599516,0.00542261211828284,
3.0445611716829));
#31128=CARTESIAN_POINT('Ctrl Pts',(0.118607834643087,0.0444203072460051,
3.04719358319151));
#31129=CARTESIAN_POINT('Ctrl Pts',(0.104002647686659,0.0834180023737263,
3.04982599470012));
#31130=CARTESIAN_POINT('Ctrl Pts',(0.0682850504048921,0.114508802006919,
3.05245840620873));
#31131=CARTESIAN_POINT('Ctrl Pts',(0.0276463521492325,0.123598791852477,
3.05509081771734));
#31132=CARTESIAN_POINT('Ctrl Pts',(-0.0129923461064282,0.132688781698037,
3.05772322922596));
#31133=CARTESIAN_POINT('Ctrl Pts',(-0.0585521453359818,0.119777961755961,
3.06035564073457));
#31134=CARTESIAN_POINT('Ctrl Pts',(-0.0883801220659878,0.0907189955750862,
3.06298805224318));
#31135=CARTESIAN_POINT('Ctrl Pts',(-0.112378957568068,0.0673388865067503,
3.06510602394943));
#31136=CARTESIAN_POINT('Ctrl Pts',(-0.126193947985427,0.0335054291562246,
3.06722399565569));
#31137=CARTESIAN_POINT('Ctrl Pts',(-0.126496969333234,-0.000107906771987382,
3.06934196736194));
#31138=CARTESIAN_POINT('Origin',(0.,0.,3.1));
#31139=CARTESIAN_POINT('',(-0.126566979141993,8.83287276302464E-5,3.11934196736194));
#31140=CARTESIAN_POINT('',(-0.126304742691185,8.06358209441624E-5,3.10565803263806));
#31141=CARTESIAN_POINT('',(-0.12645,1.54856587752183E-17,3.1));
#31142=CARTESIAN_POINT('Ctrl Pts',(-0.126304742691185,8.06358209441624E-5,
3.10565803263806));
#31143=CARTESIAN_POINT('Ctrl Pts',(-0.12639574781383,0.0154767095828029,
3.10469167536458));
#31144=CARTESIAN_POINT('Ctrl Pts',(-0.123787659959305,0.0308430184790688,
3.1037253180911));
#31145=CARTESIAN_POINT('Ctrl Pts',(-0.118340823679398,0.0451268292855474,
3.10275896081762));
#31146=CARTESIAN_POINT('Ctrl Pts',(-0.103503335617549,0.0840367324711176,
3.10012654930901));
#31147=CARTESIAN_POINT('Ctrl Pts',(-0.0676009656676162,0.114913977953889,
3.09749413780039));
#31148=CARTESIAN_POINT('Ctrl Pts',(-0.0269087833345171,0.123761458661173,
3.09486172629178));
#31149=CARTESIAN_POINT('Ctrl Pts',(0.0137833989985814,0.132608939368457,
3.09222931478317));
#31150=CARTESIAN_POINT('Ctrl Pts',(0.0592653937148459,0.119426655300253,
3.08959690327456));
#31151=CARTESIAN_POINT('Ctrl Pts',(0.0889195472648929,0.0901903286649502,
3.08696449176595));
#31152=CARTESIAN_POINT('Ctrl Pts',(0.11857370081494,0.0609540020296468,
3.08433208025733));
#31153=CARTESIAN_POINT('Ctrl Pts',(0.13240001319877,0.015663632827244,3.08169966874872));
#31154=CARTESIAN_POINT('Ctrl Pts',(0.124130814751194,-0.0251499920415489,
3.07906725724011));
#31155=CARTESIAN_POINT('Ctrl Pts',(0.115861616303618,-0.0659636169103418,
3.0764348457315));
#31156=CARTESIAN_POINT('Ctrl Pts',(0.085496907024637,-0.102300497445525,
3.07380243422289));
#31157=CARTESIAN_POINT('Ctrl Pts',(0.0468014538280004,-0.117688594137541,
3.07117002271428));
#31158=CARTESIAN_POINT('Ctrl Pts',(0.0081060006313637,-0.133076690829557,
3.06853761120566));
#31159=CARTESIAN_POINT('Ctrl Pts',(-0.0389201964829282,-0.127516003678407,
3.06590519969705));
#31160=CARTESIAN_POINT('Ctrl Pts',(-0.0729594744287227,-0.103527273515581,
3.06327278818844));
#31161=CARTESIAN_POINT('Ctrl Pts',(-0.105781189400045,-0.0803966047281269,
3.06073453633831));
#31162=CARTESIAN_POINT('Ctrl Pts',(-0.12652843654431,-0.0401326336098284,
3.05819628448819));
#31163=CARTESIAN_POINT('Ctrl Pts',(-0.126645757366777,2.69067085927681E-5,
3.05565803263806));
#31164=CARTESIAN_POINT('Ctrl Pts',(-0.126496969333234,-0.000107906771987382,
3.06934196736194));
#31165=CARTESIAN_POINT('Ctrl Pts',(-0.126570570997419,-0.00827233967750279,
3.0698564071643));
#31166=CARTESIAN_POINT('Ctrl Pts',(-0.125847009061939,-0.0164237861126916,
3.07037084696666));
#31167=CARTESIAN_POINT('Ctrl Pts',(-0.124278591835651,-0.0244092963007763,
3.07088528676901));
#31168=CARTESIAN_POINT('Ctrl Pts',(-0.116252930644851,-0.0652715095760922,
3.07351769827763));
#31169=CARTESIAN_POINT('Ctrl Pts',(-0.0861054540327919,-0.101788823707051,
3.07615010978624));
#31170=CARTESIAN_POINT('Ctrl Pts',(-0.0475024541674668,-0.117407405995615,
3.07878252129485));
#31171=CARTESIAN_POINT('Ctrl Pts',(-0.00889945430214065,-0.133025988284179,
3.08141493280346));
#31172=CARTESIAN_POINT('Ctrl Pts',(0.0381590688164514,-0.127745838730347,
3.08404734431207));
#31173=CARTESIAN_POINT('Ctrl Pts',(0.072340798251519,-0.103960526368831,
3.08667975582068));
#31174=CARTESIAN_POINT('Ctrl Pts',(0.106522527686585,-0.0801752140073166,
3.0893121673293));
#31175=CARTESIAN_POINT('Ctrl Pts',(0.127827463438127,-0.0378847388381192,
3.09194457883791));
#31176=CARTESIAN_POINT('Ctrl Pts',(0.1265977664655,0.00374000808798695,
3.09457699034652));
#31177=CARTESIAN_POINT('Ctrl Pts',(0.125368069492872,0.0453647550140949,
3.09720940185513));
#31178=CARTESIAN_POINT('Ctrl Pts',(0.101603739796073,0.0863237736971122,
3.09984181336374));
#31179=CARTESIAN_POINT('Ctrl Pts',(0.066077495668981,0.108049741788989,
3.10247422487236));
#31180=CARTESIAN_POINT('Ctrl Pts',(0.0305512515418895,0.129775709880865,
3.10510663638097));
#31181=CARTESIAN_POINT('Ctrl Pts',(-0.0167369070154944,0.132268627381602,
3.10773904788958));
#31182=CARTESIAN_POINT('Ctrl Pts',(-0.0543505659626984,0.114398418319861,
3.11037145939819));
#31183=CARTESIAN_POINT('Ctrl Pts',(-0.0919642249099026,0.096528209258119,
3.1130038709068));
#31184=CARTESIAN_POINT('Ctrl Pts',(-0.119903384246927,0.0582948736338987,
3.11563628241541));
#31185=CARTESIAN_POINT('Ctrl Pts',(-0.125502814331461,0.0170301417913753,
3.11826869392403));
#31186=CARTESIAN_POINT('Ctrl Pts',(-0.126263804720884,0.011422059561536,
3.11862645173666));
#31187=CARTESIAN_POINT('Ctrl Pts',(-0.126612176704445,0.00575798695415024,
3.1189842095493));
#31188=CARTESIAN_POINT('Ctrl Pts',(-0.126566979141993,8.83287276302464E-5,
3.11934196736194));
#31189=CARTESIAN_POINT('Origin',(0.,0.,3.1));
#31190=CARTESIAN_POINT('',(-0.126251310180948,2.19509288584552E-5,3.16934196736194));
#31191=CARTESIAN_POINT('',(-0.126368593930883,-0.000104790611567188,3.15565803263806));
#31192=CARTESIAN_POINT('',(-0.12645,1.54856587752183E-17,3.1));
#31193=CARTESIAN_POINT('Ctrl Pts',(-0.126368593930883,-0.000104790611567188,
3.15565803263806));
#31194=CARTESIAN_POINT('Ctrl Pts',(-0.126135626550864,0.029149858613393,
3.15381947774958));
#31195=CARTESIAN_POINT('Ctrl Pts',(-0.116012034435359,0.0585500300902377,
3.15198092286111));
#31196=CARTESIAN_POINT('Ctrl Pts',(-0.0974287026581059,0.0809236008148654,
3.15014236797263));
#31197=CARTESIAN_POINT('Ctrl Pts',(-0.0708214054023045,0.112957697503196,
3.14750995646402));
#31198=CARTESIAN_POINT('Ctrl Pts',(-0.0268716218413343,0.130587246038798,
3.1448775449554));
#31199=CARTESIAN_POINT('Ctrl Pts',(0.014497568206441,0.125820514172312,
3.14224513344679));
#31200=CARTESIAN_POINT('Ctrl Pts',(0.0558667582542159,0.121053782305825,
3.13961272193818));
#31201=CARTESIAN_POINT('Ctrl Pts',(0.0946553547887964,0.0938907700372525,
3.13698031042957));
#31202=CARTESIAN_POINT('Ctrl Pts',(0.113279919572572,0.0566448681887155,
3.13434789892096));
#31203=CARTESIAN_POINT('Ctrl Pts',(0.131904484356347,0.0193989663401779,
3.13171548741235));
#31204=CARTESIAN_POINT('Ctrl Pts',(0.130365017389317,-0.0279298250883239,
3.12908307590374));
#31205=CARTESIAN_POINT('Ctrl Pts',(0.109359381568105,-0.0638866725814309,
3.12645066439512));
#31206=CARTESIAN_POINT('Ctrl Pts',(0.0883537457468925,-0.0998435200745383,
3.12381825288651));
#31207=CARTESIAN_POINT('Ctrl Pts',(0.0478819410714995,-0.12442842363225,
3.1211858413779));
#31208=CARTESIAN_POINT('Ctrl Pts',(0.00629042865298903,-0.126496686825572,
3.11855342986929));
#31209=CARTESIAN_POINT('Ctrl Pts',(-0.0353010837655206,-0.128564950018895,
3.11592101836068));
#31210=CARTESIAN_POINT('Ctrl Pts',(-0.0780123039271484,-0.108116572847827,
3.11328860685206));
#31211=CARTESIAN_POINT('Ctrl Pts',(-0.102481610921079,-0.0744211038181091,
3.11065619534345));
#31212=CARTESIAN_POINT('Ctrl Pts',(-0.117968244532349,-0.0530952287799418,
3.10899014110832));
#31213=CARTESIAN_POINT('Ctrl Pts',(-0.12614784474654,-0.0264630603867145,
3.10732408687319));
#31214=CARTESIAN_POINT('Ctrl Pts',(-0.126304742691185,8.06358209441624E-5,
3.10565803263806));
#31215=CARTESIAN_POINT('Ctrl Pts',(-0.126566979141993,8.83287276302464E-5,
3.11934196736194));
#31216=CARTESIAN_POINT('Ctrl Pts',(-0.126279609310085,-0.0359598261533815,
3.12161662105791));
#31217=CARTESIAN_POINT('Ctrl Pts',(-0.110082106605306,-0.0722337808796859,
3.12389127475389));
#31218=CARTESIAN_POINT('Ctrl Pts',(-0.0828705393299942,-0.0957781595443726,
3.12616592844986));
#31219=CARTESIAN_POINT('Ctrl Pts',(-0.0513791334119502,-0.12302560097677,
3.12879833995848));
#31220=CARTESIAN_POINT('Ctrl Pts',(-0.00513662074381884,-0.133224355780737,
3.13143075146709));
#31221=CARTESIAN_POINT('Ctrl Pts',(0.034894591212013,-0.121751179208655,
3.1340631629757));
#31222=CARTESIAN_POINT('Ctrl Pts',(0.0749258031678458,-0.110278002636571,
3.13669557448431));
#31223=CARTESIAN_POINT('Ctrl Pts',(0.108745714411378,-0.0771328946884361,
3.13932798599292));
#31224=CARTESIAN_POINT('Ctrl Pts',(0.12102326443306,-0.0373410176684702,
3.14196039750153));
#31225=CARTESIAN_POINT('Ctrl Pts',(0.133300814454742,0.00245085935149471,
3.14459280901015));
#31226=CARTESIAN_POINT('Ctrl Pts',(0.124036003254574,0.0488895054432904,
3.14722522051876));
#31227=CARTESIAN_POINT('Ctrl Pts',(0.097428705282154,0.0809236029943958,
3.14985763202737));
#31228=CARTESIAN_POINT('Ctrl Pts',(0.0708214073097326,0.112957700545502,
3.15249004353598));
#31229=CARTESIAN_POINT('Ctrl Pts',(0.0268716225650577,0.130587249555918,
3.15512245504459));
#31230=CARTESIAN_POINT('Ctrl Pts',(-0.0144975685969178,0.125820517561044,
3.15775486655321));
#31231=CARTESIAN_POINT('Ctrl Pts',(-0.0558667597588919,0.121053785566171,
3.16038727806182));
#31232=CARTESIAN_POINT('Ctrl Pts',(-0.0946553573381664,0.0938907725660106,
3.16301968957043));
#31233=CARTESIAN_POINT('Ctrl Pts',(-0.113279922623555,0.0566448697143249,
3.16565210107904));
#31234=CARTESIAN_POINT('Ctrl Pts',(-0.121981975887314,0.039242271290916,
3.16688205650667));
#31235=CARTESIAN_POINT('Ctrl Pts',(-0.126282044039751,0.0196384895744722,
3.16811201193431));
#31236=CARTESIAN_POINT('Ctrl Pts',(-0.126251310180948,2.19509288584552E-5,
3.16934196736194));
#31237=CARTESIAN_POINT('Origin',(0.,0.,3.1));
#31238=CARTESIAN_POINT('',(-0.126489518850073,-0.000109039769437509,3.21934196736194));
#31239=CARTESIAN_POINT('',(-0.126647930997008,2.24668189870201E-5,3.20565803263806));
#31240=CARTESIAN_POINT('',(-0.12645,1.54856587752183E-17,3.1));
#31241=CARTESIAN_POINT('Ctrl Pts',(-0.126647930997008,2.24668189870201E-5,
3.20565803263806));
#31242=CARTESIAN_POINT('Ctrl Pts',(-0.126650996831423,0.00126189995630808,
3.2055796916432));
#31243=CARTESIAN_POINT('Ctrl Pts',(-0.126634359036856,0.00250124877863209,
3.20550135064834));
#31244=CARTESIAN_POINT('Ctrl Pts',(-0.126597763055832,0.00374000798724603,
3.20542300965348));
#31245=CARTESIAN_POINT('Ctrl Pts',(-0.125368066116328,0.0453647537922705,
3.20279059814487));
#31246=CARTESIAN_POINT('Ctrl Pts',(-0.10160373705958,0.0863237713721372,
3.20015818663626));
#31247=CARTESIAN_POINT('Ctrl Pts',(-0.0660774938893213,0.10804973887887,
3.19752577512764));
#31248=CARTESIAN_POINT('Ctrl Pts',(-0.0305512507190632,0.129775706385603,
3.19489336361903));
#31249=CARTESIAN_POINT('Ctrl Pts',(0.0167369065647044,0.132268623819202,
3.19226095211042));
#31250=CARTESIAN_POINT('Ctrl Pts',(0.0543505644988585,0.114398415238764,
3.18962854060181));
#31251=CARTESIAN_POINT('Ctrl Pts',(0.091964222433013,0.0965282066583261,
3.1869961290932));
#31252=CARTESIAN_POINT('Ctrl Pts',(0.119903381017553,0.0582948720638503,
3.18436371758459));
#31253=CARTESIAN_POINT('Ctrl Pts',(0.125502810951281,0.0170301413327138,
3.18173130607597));
#31254=CARTESIAN_POINT('Ctrl Pts',(0.13110224088501,-0.0242345893984227,
3.17909889456736));
#31255=CARTESIAN_POINT('Ctrl Pts',(0.114361942167926,-0.0685307162662204,
3.17646648305875));
#31256=CARTESIAN_POINT('Ctrl Pts',(0.0828705370980449,-0.0957781569647633,
3.17383407155014));
#31257=CARTESIAN_POINT('Ctrl Pts',(0.0513791320281642,-0.123025597663306,
3.17120166004152));
#31258=CARTESIAN_POINT('Ctrl Pts',(0.00513662060548718,-0.133224352192594,
3.16856924853291));
#31259=CARTESIAN_POINT('Ctrl Pts',(-0.0348945902721819,-0.121751175929524,
3.1659368370243));
#31260=CARTESIAN_POINT('Ctrl Pts',(-0.0749258011498519,-0.110277999666453,
3.16330442551569));
#31261=CARTESIAN_POINT('Ctrl Pts',(-0.108745711482513,-0.0771328926110206,
3.16067201400708));
#31262=CARTESIAN_POINT('Ctrl Pts',(-0.121023261173527,-0.0373410166627737,
3.15803960249846));
#31263=CARTESIAN_POINT('Ctrl Pts',(-0.124725803146683,-0.0253409763781187,
3.15724574587833));
#31264=CARTESIAN_POINT('Ctrl Pts',(-0.126469185269255,-0.0127364488245176,
3.15645188925819));
#31265=CARTESIAN_POINT('Ctrl Pts',(-0.126368593930883,-0.000104790611567188,
3.15565803263806));
#31266=CARTESIAN_POINT('Ctrl Pts',(-0.126251310180948,2.19509288584552E-5,
3.16934196736194));
#31267=CARTESIAN_POINT('Ctrl Pts',(-0.126216265913324,-0.0223457977660937,
3.17074442344292));
#31268=CARTESIAN_POINT('Ctrl Pts',(-0.120550447304899,-0.0447301326243598,
3.1721468795239));
#31269=CARTESIAN_POINT('Ctrl Pts',(-0.109359384513483,-0.0638866743021069,
3.17354933560488));
#31270=CARTESIAN_POINT('Ctrl Pts',(-0.0883537481265213,-0.0998435227636405,
3.17618174711349));
#31271=CARTESIAN_POINT('Ctrl Pts',(-0.0478819423610949,-0.124428426983496,
3.1788141586221));
#31272=CARTESIAN_POINT('Ctrl Pts',(-0.00629042882239688,-0.126496690232519,
3.18144657013071));
#31273=CARTESIAN_POINT('Ctrl Pts',(0.0353010847163008,-0.128564953481541,
3.18407898163933));
#31274=CARTESIAN_POINT('Ctrl Pts',(0.0780123060282702,-0.108116575759732,
3.18671139314794));
#31275=CARTESIAN_POINT('Ctrl Pts',(0.102481613681232,-0.0744211058224891,
3.18934380465655));
#31276=CARTESIAN_POINT('Ctrl Pts',(0.126950921334194,-0.040725635885246,
3.19197621616516));
#31277=CARTESIAN_POINT('Ctrl Pts',(0.133178315328148,0.00621692626743081,
3.19460862767377));
#31278=CARTESIAN_POINT('Ctrl Pts',(0.118340826866677,0.0451268305009631,
3.19724103918239));
#31279=CARTESIAN_POINT('Ctrl Pts',(0.103503338405205,0.0840367347344954,
3.199873450691));
#31280=CARTESIAN_POINT('Ctrl Pts',(0.0676009674883078,0.114913981048883,
3.20250586219961));
#31281=CARTESIAN_POINT('Ctrl Pts',(0.026908784059242,0.123761461994453,
3.20513827370822));
#31282=CARTESIAN_POINT('Ctrl Pts',(-0.0137833993698235,0.132608942940023,
3.20777068521683));
#31283=CARTESIAN_POINT('Ctrl Pts',(-0.0592653953110574,0.119426658516775,
3.21040309672544));
#31284=CARTESIAN_POINT('Ctrl Pts',(-0.0889195496597795,0.0901903310940448,
3.21303550823405));
#31285=CARTESIAN_POINT('Ctrl Pts',(-0.11260033459284,0.0668432083338218,
3.21513766127668));
#31286=CARTESIAN_POINT('Ctrl Pts',(-0.126187596109782,0.0332583119648893,
3.21723981431931));
#31287=CARTESIAN_POINT('Ctrl Pts',(-0.126489518850073,-0.000109039769437509,
3.21934196736194));
#31288=CARTESIAN_POINT('Origin',(0.,0.,3.1));
#31289=CARTESIAN_POINT('',(-0.126573425356775,8.55484528903966E-5,3.26934196736194));
#31290=CARTESIAN_POINT('',(-0.126309785017077,8.34376343069358E-5,3.25565803263806));
#31291=CARTESIAN_POINT('',(-0.12645,1.54856587752183E-17,3.1));
#31292=CARTESIAN_POINT('Ctrl Pts',(-0.126309785017077,8.34376343069358E-5,
3.25565803263806));
#31293=CARTESIAN_POINT('Ctrl Pts',(-0.126402648710969,0.0152259667938181,
3.2547074940282));
#31294=CARTESIAN_POINT('Ctrl Pts',(-0.123881624579711,0.0303386118332616,
3.25375695541835));
#31295=CARTESIAN_POINT('Ctrl Pts',(-0.118607831448617,0.0444203060496175,
3.25280641680849));
#31296=CARTESIAN_POINT('Ctrl Pts',(-0.104002644885555,0.0834180001270126,
3.25017400529988));
#31297=CARTESIAN_POINT('Ctrl Pts',(-0.0682850485657758,0.114508798922838,
3.24754159379127));
#31298=CARTESIAN_POINT('Ctrl Pts',(-0.0276463514046418,0.123598788523579,
3.24490918228266));
#31299=CARTESIAN_POINT('Ctrl Pts',(0.0129923457564923,0.13268877812432,
3.24227677077404));
#31300=CARTESIAN_POINT('Ctrl Pts',(0.0585521437589804,0.119777958529977,
3.23964435926544));
#31301=CARTESIAN_POINT('Ctrl Pts',(0.0883801196856296,0.090718993131753,
3.23701194775682));
#31302=CARTESIAN_POINT('Ctrl Pts',(0.118208095612278,0.0616600277335293,
3.23437953624821));
#31303=CARTESIAN_POINT('Ctrl Pts',(0.132304249463088,0.0164529165314243,
3.2317471247396));
#31304=CARTESIAN_POINT('Ctrl Pts',(0.124278588488448,-0.024409295643347,
3.22911471323098));
#31305=CARTESIAN_POINT('Ctrl Pts',(0.116252927513807,-0.0652715078181186,
3.22648230172237));
#31306=CARTESIAN_POINT('Ctrl Pts',(0.0861054517137156,-0.101788820965557,
3.22384989021376));
#31307=CARTESIAN_POINT('Ctrl Pts',(0.0475024528880895,-0.117407402833467,
3.22121747870515));
#31308=CARTESIAN_POINT('Ctrl Pts',(0.00889945406246312,-0.133025984701378,
3.21858506719654));
#31309=CARTESIAN_POINT('Ctrl Pts',(-0.0381590677886978,-0.127745835289761,
3.21595265568793));
#31310=CARTESIAN_POINT('Ctrl Pts',(-0.0723407963031478,-0.103960523568861,
3.21332024417931));
#31311=CARTESIAN_POINT('Ctrl Pts',(-0.105505271014729,-0.0808830665952798,
3.21076617366556));
#31312=CARTESIAN_POINT('Ctrl Pts',(-0.126547978765194,-0.0403854911787608,
3.20821210315181));
#31313=CARTESIAN_POINT('Ctrl Pts',(-0.126647930997008,2.24668189870201E-5,
3.20565803263806));
#31314=CARTESIAN_POINT('Ctrl Pts',(-0.126489518850073,-0.000109039769437509,
3.21934196736194));
#31315=CARTESIAN_POINT('Ctrl Pts',(-0.126565677476903,-0.00852580124482262,
3.21987222582793));
#31316=CARTESIAN_POINT('Ctrl Pts',(-0.125796519899578,-0.0169287208447501,
3.22040248429391));
#31317=CARTESIAN_POINT('Ctrl Pts',(-0.124130818094417,-0.0251499927189283,
3.22093274275989));
#31318=CARTESIAN_POINT('Ctrl Pts',(-0.115861619424122,-0.065963618686957,
3.2235651542685));
#31319=CARTESIAN_POINT('Ctrl Pts',(-0.0854969093273219,-0.102300500200801,
3.22619756577711));
#31320=CARTESIAN_POINT('Ctrl Pts',(-0.0468014550884958,-0.117688597307262,
3.22882997728573));
#31321=CARTESIAN_POINT('Ctrl Pts',(-0.00810600084966979,-0.133076694413723,
3.23146238879434));
#31322=CARTESIAN_POINT('Ctrl Pts',(0.038920197531182,-0.127516007112802,
3.23409480030295));
#31323=CARTESIAN_POINT('Ctrl Pts',(0.0729594763937567,-0.103527276303882,
3.23672721181156));
#31324=CARTESIAN_POINT('Ctrl Pts',(0.106998755256331,-0.0795385454949616,
3.23935962332018));
#31325=CARTESIAN_POINT('Ctrl Pts',(0.128051114600629,-0.0371217711780427,
3.24199203482878));
#31326=CARTESIAN_POINT('Ctrl Pts',(0.126573211966284,0.00449490234484176,
3.2446244463374));
#31327=CARTESIAN_POINT('Ctrl Pts',(0.125095309331938,0.0461115758677259,
3.24725685784601));
#31328=CARTESIAN_POINT('Ctrl Pts',(0.10108714471895,0.0869281485965757,
3.24988926935462));
#31329=CARTESIAN_POINT('Ctrl Pts',(0.0654319703557041,0.108441871018171,
3.25252168086323));
#31330=CARTESIAN_POINT('Ctrl Pts',(0.0297767959924581,0.129955593439766,
3.25515409237185));
#31331=CARTESIAN_POINT('Ctrl Pts',(-0.0175253881210462,0.132166465554107,
3.25778650388046));
#31332=CARTESIAN_POINT('Ctrl Pts',(-0.0550318099545696,0.114072266689479,
3.26041891538907));
#31333=CARTESIAN_POINT('Ctrl Pts',(-0.0925382317880931,0.09597806782485,
3.26305132689768));
#31334=CARTESIAN_POINT('Ctrl Pts',(-0.120248891341636,0.0575787979812516,
3.26568373840629));
#31335=CARTESIAN_POINT('Ctrl Pts',(-0.125602141267406,0.0162814079119122,
3.26831614991491));
#31336=CARTESIAN_POINT('Ctrl Pts',(-0.126297505847784,0.0109170511726472,
3.26865808906392));
#31337=CARTESIAN_POINT('Ctrl Pts',(-0.126615635779588,0.00550379470022512,
3.26900002821293));
#31338=CARTESIAN_POINT('Ctrl Pts',(-0.126573425356775,8.55484528903966E-5,
3.26934196736194));
#31339=CARTESIAN_POINT('Origin',(0.,0.,3.1));
#31340=CARTESIAN_POINT('',(-0.126252746279467,2.59119664437757E-5,3.31934196736194));
#31341=CARTESIAN_POINT('',(-0.126362016509238,-0.00010321110317447,3.30565803263806));
#31342=CARTESIAN_POINT('',(-0.12645,1.54856587752183E-17,3.1));
#31343=CARTESIAN_POINT('Ctrl Pts',(-0.126362016509238,-0.00010321110317447,
3.30565803263806));
#31344=CARTESIAN_POINT('Ctrl Pts',(-0.126135404540093,0.0289035586789932,
3.30383529641321));
#31345=CARTESIAN_POINT('Ctrl Pts',(-0.116200394811108,0.0580506048820654,
3.30201256018836));
#31346=CARTESIAN_POINT('Ctrl Pts',(-0.0979095549055491,0.080341149659951,
3.30018982396351));
#31347=CARTESIAN_POINT('Ctrl Pts',(-0.0714937648350404,0.112533348293265,
3.2975574124549));
#31348=CARTESIAN_POINT('Ctrl Pts',(-0.0276498958846022,0.130424676138957,
3.29492500094628));
#31349=CARTESIAN_POINT('Ctrl Pts',(0.0137469847697539,0.125904732556904,
3.29229258943767));
#31350=CARTESIAN_POINT('Ctrl Pts',(0.05514386542411,0.12138478897485,3.28966017792906));
#31351=CARTESIAN_POINT('Ctrl Pts',(0.0940937577823839,0.0944535739650504,
3.28702776642045));
#31352=CARTESIAN_POINT('Ctrl Pts',(0.112940105850529,0.057319401261323,
3.28439535491184));
#31353=CARTESIAN_POINT('Ctrl Pts',(0.131786453918674,0.0201852285575958,
3.28176294340322));
#31354=CARTESIAN_POINT('Ctrl Pts',(0.13052925769669,-0.0271519018400594,
3.27913053189461));
#31355=CARTESIAN_POINT('Ctrl Pts',(0.109738422623206,-0.0632333762395775,
3.276498120386));
#31356=CARTESIAN_POINT('Ctrl Pts',(0.0889475875497212,-0.099314850639096,
3.27386570887739));
#31357=CARTESIAN_POINT('Ctrl Pts',(0.0486231136247353,-0.124140669040477,
3.27123329736878));
#31358=CARTESIAN_POINT('Ctrl Pts',(0.00704467477488957,-0.126456924791809,
3.26860088586016));
#31359=CARTESIAN_POINT('Ctrl Pts',(-0.0345337640749562,-0.128773180543141,
3.26596847435155));
#31360=CARTESIAN_POINT('Ctrl Pts',(-0.0773661678496626,-0.108579873644424,
3.26333606284294));
#31361=CARTESIAN_POINT('Ctrl Pts',(-0.102035981333843,-0.0750309255155824,
3.26070365133433));
#31362=CARTESIAN_POINT('Ctrl Pts',(-0.117797761200207,-0.0535961815725874,
3.25902177843557));
#31363=CARTESIAN_POINT('Ctrl Pts',(-0.126145472985543,-0.026709592283637,
3.25733990553681));
#31364=CARTESIAN_POINT('Ctrl Pts',(-0.126309785017077,8.34376343069358E-5,
3.25565803263806));
#31365=CARTESIAN_POINT('Ctrl Pts',(-0.126573425356775,8.55484528903966E-5,
3.26934196736194));
#31366=CARTESIAN_POINT('Ctrl Pts',(-0.126290679707385,-0.0362084626390545,
3.27163243972154));
#31367=CARTESIAN_POINT('Ctrl Pts',(-0.109839596819478,-0.0727263630692267,
3.27392291208114));
#31368=CARTESIAN_POINT('Ctrl Pts',(-0.0822978965038287,-0.0962706516317226,
3.27621338444074));
#31369=CARTESIAN_POINT('Ctrl Pts',(-0.0506445615164858,-0.123329810810936,
3.27884579594935));
#31370=CARTESIAN_POINT('Ctrl Pts',(-0.00434205124380389,-0.133252618874282,
3.28147820745796));
#31371=CARTESIAN_POINT('Ctrl Pts',(0.0356200290599969,-0.121540921768417,
3.28411061896657));
#31372=CARTESIAN_POINT('Ctrl Pts',(0.0755821093637979,-0.109829224662552,
3.28674303047519));
#31373=CARTESIAN_POINT('Ctrl Pts',(0.109203759698717,-0.0764830223874748,
3.2893754419838));
#31374=CARTESIAN_POINT('Ctrl Pts',(0.121243794125388,-0.0366186362475693,
3.29200785349241));
#31375=CARTESIAN_POINT('Ctrl Pts',(0.133283828552059,0.00324574989233616,
3.29464026500102));
#31376=CARTESIAN_POINT('Ctrl Pts',(0.123742247070482,0.0496283198970706,
3.29727267650964));
#31377=CARTESIAN_POINT('Ctrl Pts',(0.0969443881476166,0.0815031762647041,
3.29990508801825));
#31378=CARTESIAN_POINT('Ctrl Pts',(0.0701465292247518,0.113378032632337,
3.30253749952686));
#31379=CARTESIAN_POINT('Ctrl Pts',(0.0260923928606002,0.130745175362871,
3.30516991103547));
#31380=CARTESIAN_POINT('Ctrl Pts',(-0.0152476364742436,0.125731824597042,
3.30780232254408));
#31381=CARTESIAN_POINT('Ctrl Pts',(-0.0565876658090873,0.120718473831214,
3.31043473405269));
#31382=CARTESIAN_POINT('Ctrl Pts',(-0.095213588114623,0.0933246295690233,
3.31306714556131));
#31383=CARTESIAN_POINT('Ctrl Pts',(-0.113615707760984,0.0559683221521016,
3.31569955706992));
#31384=CARTESIAN_POINT('Ctrl Pts',(-0.122103244730499,0.0387386200124153,
3.31691369383393));
#31385=CARTESIAN_POINT('Ctrl Pts',(-0.12628858288157,0.0193896083672227,
3.31812783059793));
#31386=CARTESIAN_POINT('Ctrl Pts',(-0.126252746279467,2.59119664437757E-5,
3.31934196736194));
#31387=CARTESIAN_POINT('Origin',(0.,0.,3.1));
#31388=CARTESIAN_POINT('',(-0.126482040448775,-0.000110013702131137,3.36934196736194));
#31389=CARTESIAN_POINT('',(-0.126649735277799,1.79833793418055E-5,3.35565803263806));
#31390=CARTESIAN_POINT('',(-0.12645,1.54856587752183E-17,3.1));
#31391=CARTESIAN_POINT('Ctrl Pts',(-0.126649735277799,1.79833793418055E-5,
3.35565803263806));
#31392=CARTESIAN_POINT('Ctrl Pts',(-0.126651722007443,0.00100711151136191,
3.35559551030682));
#31393=CARTESIAN_POINT('Ctrl Pts',(-0.126641125668946,0.0019961959922384,
3.35553298797559));
#31394=CARTESIAN_POINT('Ctrl Pts',(-0.126617815335903,0.00298498074413288,
3.35547046564436));
#31395=CARTESIAN_POINT('Ctrl Pts',(-0.12563636778334,0.0446163196439928,
3.35283805413574));
#31396=CARTESIAN_POINT('Ctrl Pts',(-0.102116718771259,0.085716326541524,
3.35020564262713));
#31397=CARTESIAN_POINT('Ctrl Pts',(-0.0667206692597134,0.107653767068442,
3.34757323111852));
#31398=CARTESIAN_POINT('Ctrl Pts',(-0.0313246197481669,0.12959120759536,
3.34494081960991));
#31399=CARTESIAN_POINT('Ctrl Pts',(0.0159478302628458,0.132366081751665,
3.3423084081013));
#31400=CARTESIAN_POINT('Ctrl Pts',(0.0536673876466801,0.114720498489436,
3.33967599659268));
#31401=CARTESIAN_POINT('Ctrl Pts',(0.0913869450305144,0.0970749152272078,
3.33704358508407));
#31402=CARTESIAN_POINT('Ctrl Pts',(0.11955360978717,0.059008874546446,3.33441117357546));
#31403=CARTESIAN_POINT('Ctrl Pts',(0.12539902073952,0.0177782695461103,
3.33177876206685));
#31404=CARTESIAN_POINT('Ctrl Pts',(0.13124443169187,-0.0234523354542255,
3.32914635055824));
#31405=CARTESIAN_POINT('Ctrl Pts',(0.114768588839913,-0.0678475047741352,
3.32651393904963));
#31406=CARTESIAN_POINT('Ctrl Pts',(0.083440232769335,-0.0952822587152781,
3.32388152754101));
#31407=CARTESIAN_POINT('Ctrl Pts',(0.0521118766987572,-0.122717012656421,
3.3212491160324));
#31408=CARTESIAN_POINT('Ctrl Pts',(0.00593100740955835,-0.133191351218797,
3.31861670452379));
#31409=CARTESIAN_POINT('Ctrl Pts',(-0.0341679114813036,-0.121957103505662,
3.31598429301518));
#31410=CARTESIAN_POINT('Ctrl Pts',(-0.0742668303721658,-0.110722855792528,
3.31335188150657));
#31411=CARTESIAN_POINT('Ctrl Pts',(-0.108283798864691,-0.0777800218038817,
3.31071946999795));
#31412=CARTESIAN_POINT('Ctrl Pts',(-0.120798427515664,-0.0380620700990904,
3.30808705848934));
#31413=CARTESIAN_POINT('Ctrl Pts',(-0.124647668210362,-0.0258456503973156,
3.30727738320558));
#31414=CARTESIAN_POINT('Ctrl Pts',(-0.126462679516819,-0.0129882705177865,
3.30646770792182));
#31415=CARTESIAN_POINT('Ctrl Pts',(-0.126362016509238,-0.00010321110317447,
3.30565803263806));
#31416=CARTESIAN_POINT('Ctrl Pts',(-0.126252746279467,2.59119664437757E-5,
3.31934196736194));
#31417=CARTESIAN_POINT('Ctrl Pts',(-0.126210884316958,-0.0225934851076951,
3.32076024210655));
#31418=CARTESIAN_POINT('Ctrl Pts',(-0.120409070525885,-0.0452329200835406,
3.32217851685115));
#31419=CARTESIAN_POINT('Ctrl Pts',(-0.108976454281191,-0.064537698648537,
3.32359679159575));
#31420=CARTESIAN_POINT('Ctrl Pts',(-0.0877567641678496,-0.100368641460601,
3.32622920310437));
#31421=CARTESIAN_POINT('Ctrl Pts',(-0.047139066953979,-0.124711756513075,
3.32886161461298));
#31422=CARTESIAN_POINT('Ctrl Pts',(-0.00553595897255799,-0.126531953643381,
3.33149402612159));
#31423=CARTESIAN_POINT('Ctrl Pts',(0.0360671490088627,-0.128352150773687,
3.3341264376302));
#31424=CARTESIAN_POINT('Ctrl Pts',(0.0786556677578339,-0.107649429981826,
3.33675884913881));
#31425=CARTESIAN_POINT('Ctrl Pts',(0.102923598708863,-0.0738086374577052,
3.33939126064743));
#31426=CARTESIAN_POINT('Ctrl Pts',(0.127191529659892,-0.0399678449335842,
3.34202367215604));
#31427=CARTESIAN_POINT('Ctrl Pts',(0.133138872812978,0.00701101932279596,
3.34465608366465));
#31428=CARTESIAN_POINT('Ctrl Pts',(0.118069610514671,0.0458317489024548,
3.34728849517326));
#31429=CARTESIAN_POINT('Ctrl Pts',(0.103000348216365,0.0846524784821133,
3.34992090668187));
#31430=CARTESIAN_POINT('Ctrl Pts',(0.0669144804666656,0.11531507338505,
3.35255331819048));
#31431=CARTESIAN_POINT('Ctrl Pts',(0.0261702590074494,0.123919730785983,
3.3551857296991));
#31432=CARTESIAN_POINT('Ctrl Pts',(-0.0145739624517671,0.132524388186917,
3.35781814120771));
#31433=CARTESIAN_POINT('Ctrl Pts',(-0.059976537620501,0.119071108085846,
3.36045055271632));
#31434=CARTESIAN_POINT('Ctrl Pts',(-0.0894558149920353,0.0896584591581523,
3.36308296422493));
#31435=CARTESIAN_POINT('Ctrl Pts',(-0.112819802593213,0.0663472783512584,
3.36516929860394));
#31436=CARTESIAN_POINT('Ctrl Pts',(-0.126181642003826,0.033011291498231,
3.36725563298294));
#31437=CARTESIAN_POINT('Ctrl Pts',(-0.126482040448775,-0.000110013702131137,
3.36934196736194));
#31438=CARTESIAN_POINT('Origin',(0.,0.,3.1));
#31439=CARTESIAN_POINT('',(-0.126579711874066,8.26312290282544E-5,3.41934196736194));
#31440=CARTESIAN_POINT('',(-0.126315008613134,8.61315354740502E-5,3.40565803263806));
#31441=CARTESIAN_POINT('',(-0.12645,1.54856587752183E-17,3.1));
#31442=CARTESIAN_POINT('Ctrl Pts',(-0.126315008613134,8.61315354740502E-5,
3.40565803263806));
#31443=CARTESIAN_POINT('Ctrl Pts',(-0.12640952887744,0.0149751122618111,
3.40472331269183));
#31444=CARTESIAN_POINT('Ctrl Pts',(-0.123973978584825,0.029834173019371,
3.4037885927456));
#31445=CARTESIAN_POINT('Ctrl Pts',(-0.118870621145655,0.0437122030848606,
3.40285387279937));
#31446=CARTESIAN_POINT('Ctrl Pts',(-0.104498255487237,0.0827963011707195,
3.40022146129076));
#31447=CARTESIAN_POINT('Ctrl Pts',(-0.0689667030308244,0.114099547595362,
3.39758904978215));
#31448=CARTESIAN_POINT('Ctrl Pts',(-0.0283829362832705,0.123431722821457,
3.39495663827353));
#31449=CARTESIAN_POINT('Ctrl Pts',(0.0122008304642834,0.132763898047552,
3.39232422676492));
#31450=CARTESIAN_POINT('Ctrl Pts',(0.0578368115029788,0.120125002075099,
3.38969181525631));
#31451=CARTESIAN_POINT('Ctrl Pts',(0.0878375490289461,0.0912444313426293,
3.3870594037477));
#31452=CARTESIAN_POINT('Ctrl Pts',(0.117838286554913,0.0623638606101592,
3.38442699223909));
#31453=CARTESIAN_POINT('Ctrl Pts',(0.132203780568153,0.0172416151176717,
3.38179458073047));
#31454=CARTESIAN_POINT('Ctrl Pts',(0.124421942484303,-0.0236677311728431,
3.37916216922186));
#31455=CARTESIAN_POINT('Ctrl Pts',(0.116640104400452,-0.0645770774633583,
3.37652975771325));
#31456=CARTESIAN_POINT('Ctrl Pts',(0.0867109342195124,-0.1012735245519,
3.37389734620464));
#31457=CARTESIAN_POINT('Ctrl Pts',(0.0482017626101867,-0.117122036149449,
3.37126493469603));
#31458=CARTESIAN_POINT('Ctrl Pts',(0.00969259100086189,-0.132970547746997,
3.36863252318742));
#31459=CARTESIAN_POINT('Ctrl Pts',(-0.0373965820368482,-0.127971123853552,
3.3660001116788));
#31460=CARTESIAN_POINT('Ctrl Pts',(-0.0717195455091802,-0.104390076455735,
3.36336770017019));
#31461=CARTESIAN_POINT('Ctrl Pts',(-0.105227305247545,-0.0813691018472357,
3.36079781099281));
#31462=CARTESIAN_POINT('Ctrl Pts',(-0.126568073655319,-0.0406386849075436,
3.35822792181544));
#31463=CARTESIAN_POINT('Ctrl Pts',(-0.126649735277799,1.79833793418055E-5,
3.35565803263806));
#31464=CARTESIAN_POINT('Ctrl Pts',(-0.126482040448775,-0.000110013702131137,
3.36934196736194));
#31465=CARTESIAN_POINT('Ctrl Pts',(-0.126560666733329,-0.00877918363707953,
3.36988804449155));
#31466=CARTESIAN_POINT('Ctrl Pts',(-0.125744482172779,-0.0174336462000347,
3.37043412162116));
#31467=CARTESIAN_POINT('Ctrl Pts',(-0.123978629867097,-0.0258897947229394,
3.37098019875077));
#31468=CARTESIAN_POINT('Ctrl Pts',(-0.115466187796289,-0.0666533819220227,
3.37361261025938));
#31469=CARTESIAN_POINT('Ctrl Pts',(-0.0848853240803387,-0.102808538565874,
3.37624502176799));
#31470=CARTESIAN_POINT('Ctrl Pts',(-0.046098791601206,-0.117965603239704,
3.3788774332766));
#31471=CARTESIAN_POINT('Ctrl Pts',(-0.00731225912207339,-0.133122667913533,
3.38150984478522));
#31472=CARTESIAN_POINT('Ctrl Pts',(0.0396799421202415,-0.127281640617341,
3.38414225629383));
#31473=CARTESIAN_POINT('Ctrl Pts',(0.0735755598654084,-0.103090344478252,
3.38677466780244));
#31474=CARTESIAN_POINT('Ctrl Pts',(0.107471177610575,-0.0788990483391635,
3.38940707931105));
#31475=CARTESIAN_POINT('Ctrl Pts',(0.128270211858594,-0.0363574833571786,
3.39203949081966));
#31476=CARTESIAN_POINT('Ctrl Pts',(0.126544156121574,0.00524963674486975,
3.39467190232827));
#31477=CARTESIAN_POINT('Ctrl Pts',(0.124818100384554,0.0468567568469189,
3.39730431383689));
#31478=CARTESIAN_POINT('Ctrl Pts',(0.100566954662495,0.0875294320690312,
3.3999367253455));
#31479=CARTESIAN_POINT('Ctrl Pts',(0.0647841180740634,0.108830143717421,
3.40256913685411));
#31480=CARTESIAN_POINT('Ctrl Pts',(0.0290012814856321,0.13013085536581,
3.40520154836272));
#31481=CARTESIAN_POINT('Ctrl Pts',(-0.0183132459691715,0.132059603440478,
3.40783395987133));
#31482=CARTESIAN_POINT('Ctrl Pts',(-0.0557110968410662,0.113742058272906,
3.41046637137995));
#31483=CARTESIAN_POINT('Ctrl Pts',(-0.0931089477129611,0.0954245131053351,
3.41309878288856));
#31484=CARTESIAN_POINT('Ctrl Pts',(-0.120590122001947,0.056860674695525,
3.41573119439717));
#31485=CARTESIAN_POINT('Ctrl Pts',(-0.125697001391323,0.0155320950411155,
3.41836360590578));
#31486=CARTESIAN_POINT('Ctrl Pts',(-0.126329675264624,0.0104120382364903,
3.41868972639117));
#31487=CARTESIAN_POINT('Ctrl Pts',(-0.126618950983805,0.00524954849512788,
3.41901584687656));
#31488=CARTESIAN_POINT('Ctrl Pts',(-0.126579711874066,8.26312290282544E-5,
3.41934196736194));
#31489=CARTESIAN_POINT('Origin',(0.,0.,3.1));
#31490=CARTESIAN_POINT('',(-0.126254420230949,2.98387352259399E-5,3.46934196736194));
#31491=CARTESIAN_POINT('',(-0.126355565467006,-0.000101493988421879,3.45565803263806));
#31492=CARTESIAN_POINT('',(-0.12645,1.54856587752183E-17,3.1));
#31493=CARTESIAN_POINT('Ctrl Pts',(-0.126355565467006,-0.000101493988421879,
3.45565803263806));
#31494=CARTESIAN_POINT('Ctrl Pts',(-0.126135472102513,0.0286572548844595,
3.45385111507683));
#31495=CARTESIAN_POINT('Ctrl Pts',(-0.116386929963108,0.0575510084273647,
3.45204419751561));
#31496=CARTESIAN_POINT('Ctrl Pts',(-0.0983869251245805,0.079755841232973,
3.45023727995438));
#31497=CARTESIAN_POINT('Ctrl Pts',(-0.0721635816202546,0.112104996877157,
3.44760486844577));
#31498=CARTESIAN_POINT('Ctrl Pts',(-0.0284271866124946,0.130257467927816,
3.44497245693716));
#31499=CARTESIAN_POINT('Ctrl Pts',(0.0129959124187107,0.125984473413918,
3.44234004542855));
#31500=CARTESIAN_POINT('Ctrl Pts',(0.0544190114499162,0.121711478900021,
3.43970763391994));
#31501=CARTESIAN_POINT('Ctrl Pts',(0.0935288145045671,0.0950130188215667,
3.43707522241132));
#31502=CARTESIAN_POINT('Ctrl Pts',(0.112596275634196,0.0579918958508686,
3.43444281090271));
#31503=CARTESIAN_POINT('Ctrl Pts',(0.131663736763825,0.0209707728801704,
3.4318103993941));
#31504=CARTESIAN_POINT('Ctrl Pts',(0.130688855968432,-0.0263730129827715,
3.42917798788549));
#31505=CARTESIAN_POINT('Ctrl Pts',(0.110113561023984,-0.0625778311060434,
3.42654557637688));
#31506=CARTESIAN_POINT('Ctrl Pts',(0.0895382660795356,-0.0987826492293151,
3.42391316486827));
#31507=CARTESIAN_POINT('Ctrl Pts',(0.0493625569860325,-0.123848499612917,
3.42128075335965));
#31508=CARTESIAN_POINT('Ctrl Pts',(0.00779867036970612,-0.12641266555449,
3.41864834185104));
#31509=CARTESIAN_POINT('Ctrl Pts',(-0.0337652162466206,-0.128976831496062,
3.41601593034243));
#31510=CARTESIAN_POINT('Ctrl Pts',(-0.0767172803857706,-0.109039312995606,
3.41338351883382));
#31511=CARTESIAN_POINT('Ctrl Pts',(-0.101586723025134,-0.0756380788718395,
3.41075110732521));
#31512=CARTESIAN_POINT('Ctrl Pts',(-0.117625493100354,-0.0540969964234629,
3.40905341576282));
#31513=CARTESIAN_POINT('Ctrl Pts',(-0.126143335529839,-0.0269560826095475,
3.40735572420044));
#31514=CARTESIAN_POINT('Ctrl Pts',(-0.126315008613134,8.61315354740502E-5,
3.40565803263806));
#31515=CARTESIAN_POINT('Ctrl Pts',(-0.126579711874066,8.26312290282544E-5,
3.41934196736194));
#31516=CARTESIAN_POINT('Ctrl Pts',(-0.126302216866535,-0.0364572840554096,
3.42164825838517));
#31517=CARTESIAN_POINT('Ctrl Pts',(-0.109595120153288,-0.0732186276029635,
3.42395454940839));
#31518=CARTESIAN_POINT('Ctrl Pts',(-0.0817223269051259,-0.0967597200814019,
3.42626084043162));
#31519=CARTESIAN_POINT('Ctrl Pts',(-0.0499081885397876,-0.123629634650501,
3.42889325194023));
#31520=CARTESIAN_POINT('Ctrl Pts',(-0.00354732731934525,-0.133276142889689,
3.43152566344884));
#31521=CARTESIAN_POINT('Ctrl Pts',(0.0363442001504806,-0.121326341846207,
3.43415807495745));
#31522=CARTESIAN_POINT('Ctrl Pts',(0.0762357276203061,-0.109376540802726,
3.43679048646606));
#31523=CARTESIAN_POINT('Ctrl Pts',(0.109657921339515,-0.0758304304765741,
3.43942289797468));
#31524=CARTESIAN_POINT('Ctrl Pts',(0.121460011995994,-0.0358949527457304,
3.44205530948329));
#31525=CARTESIAN_POINT('Ctrl Pts',(0.133262102652474,0.00404052498511346,
3.4446877209919));
#31526=CARTESIAN_POINT('Ctrl Pts',(0.123444090246223,0.0503653701206494,
3.44732013250051));
#31527=CARTESIAN_POINT('Ctrl Pts',(0.0964566233770265,0.0820798513966518,
3.44995254400912));
#31528=CARTESIAN_POINT('Ctrl Pts',(0.0694691565078302,0.113794332672654,
3.45258495551774));
#31529=CARTESIAN_POINT('Ctrl Pts',(0.0253122351756883,0.130898450089123,
3.45521736702635));
#31530=CARTESIAN_POINT('Ctrl Pts',(-0.0159971621245858,0.12563865949158,
3.45784977853496));
#31531=CARTESIAN_POINT('Ctrl Pts',(-0.0573065594248602,0.120378868894038,
3.46048219004357));
#31532=CARTESIAN_POINT('Ctrl Pts',(-0.0957684326932668,0.0927551702824843,
3.46311460155218));
#31533=CARTESIAN_POINT('Ctrl Pts',(-0.113947452310361,0.0552897855612304,
3.46574701306079));
#31534=CARTESIAN_POINT('Ctrl Pts',(-0.122222848532838,0.0382349107810562,
3.46694533116118));
#31535=CARTESIAN_POINT('Ctrl Pts',(-0.126295183358791,0.0191406182899676,
3.46814364926156));
#31536=CARTESIAN_POINT('Ctrl Pts',(-0.126254420230949,2.98387352259399E-5,
3.46934196736194));
#31537=CARTESIAN_POINT('Origin',(0.,0.,3.1));
#31538=CARTESIAN_POINT('',(-0.126474550616365,-0.00011099430647141,3.51934196736194));
#31539=CARTESIAN_POINT('',(-0.12665116202208,1.34725138570783E-5,3.50565803263806));
#31540=CARTESIAN_POINT('',(-0.12645,1.54856587752183E-17,3.1));
#31541=CARTESIAN_POINT('Ctrl Pts',(-0.12665116202208,1.34725138570783E-5,
3.50565803263806));
#31542=CARTESIAN_POINT('Ctrl Pts',(-0.126652289762307,0.000752320916696393,
3.50561132897045));
#31543=CARTESIAN_POINT('Ctrl Pts',(-0.126646377467723,0.00149115078533116,
3.50556462530284));
#31544=CARTESIAN_POINT('Ctrl Pts',(-0.126633369929918,0.00222985570861129,
3.50551792163523));
#31545=CARTESIAN_POINT('Ctrl Pts',(-0.125900211401467,0.0438663147077999,
3.50288551012662));
#31546=CARTESIAN_POINT('Ctrl Pts',(-0.102626068622182,0.0851058329421116,
3.50025309861801));
#31547=CARTESIAN_POINT('Ctrl Pts',(-0.067361469104998,0.107253962401741,
3.4976206871094));
#31548=CARTESIAN_POINT('Ctrl Pts',(-0.0320968695878142,0.129402091861371,
3.49498827560079));
#31549=CARTESIAN_POINT('Ctrl Pts',(0.0151581866672683,0.132458832546319,
3.49235586409217));
#31550=CARTESIAN_POINT('Ctrl Pts',(0.0529823007948782,0.115038504173862,
3.48972345258356));
#31551=CARTESIAN_POINT('Ctrl Pts',(0.0908064149224882,0.0976181758014056,
3.48709104107495));
#31552=CARTESIAN_POINT('Ctrl Pts',(0.119199586922625,0.0597207783715444,
3.48445862956634));
#31553=CARTESIAN_POINT('Ctrl Pts',(0.125290771676778,0.0185257643337426,
3.48182621805773));
#31554=CARTESIAN_POINT('Ctrl Pts',(0.131381956430931,-0.0226692497040593,
3.47919380654911));
#31555=CARTESIAN_POINT('Ctrl Pts',(0.115171153939098,-0.0671618803498017,
3.4765613950405));
#31556=CARTESIAN_POINT('Ctrl Pts',(0.0840069606582608,-0.0947829713159226,
3.47392898353189));
#31557=CARTESIAN_POINT('Ctrl Pts',(0.0528427673774234,-0.122404062282043,
3.47129657202328));
#31558=CARTESIAN_POINT('Ctrl Pts',(0.00672518330758078,-0.133153613568543,
3.46866416051467));
#31559=CARTESIAN_POINT('Ctrl Pts',(-0.0334400173720784,-0.122158694217057,
3.46603174900606));
#31560=CARTESIAN_POINT('Ctrl Pts',(-0.0736052180517379,-0.111163774865571,
3.46339933749744));
#31561=CARTESIAN_POINT('Ctrl Pts',(-0.107818035341214,-0.0784243848761005,
3.46076692598883));
#31562=CARTESIAN_POINT('Ctrl Pts',(-0.120569297985506,-0.0387817697625104,
3.45813451448022));
#31563=CARTESIAN_POINT('Ctrl Pts',(-0.12456794717085,-0.0263503019894106,
3.45730902053283));
#31564=CARTESIAN_POINT('Ctrl Pts',(-0.126456115566329,-0.013239986655944,
3.45648352658544));
#31565=CARTESIAN_POINT('Ctrl Pts',(-0.126355565467006,-0.000101493988421879,
3.45565803263806));
#31566=CARTESIAN_POINT('Ctrl Pts',(-0.126254420230949,2.98387352259399E-5,
3.46934196736194));
#31567=CARTESIAN_POINT('Ctrl Pts',(-0.126205636746063,-0.0228410859189539,
3.47077606077017));
#31568=CARTESIAN_POINT('Ctrl Pts',(-0.120265979813939,-0.045735623724726,
3.4722101541784));
#31569=CARTESIAN_POINT('Ctrl Pts',(-0.108589648601543,-0.0651864304899691,
3.47364424758663));
#31570=CARTESIAN_POINT('Ctrl Pts',(-0.0871566593098471,-0.100890190988961,
3.47627665909524));
#31571=CARTESIAN_POINT('Ctrl Pts',(-0.0463945147606729,-0.124990641155991,
3.47890907060385));
#31572=CARTESIAN_POINT('Ctrl Pts',(-0.00478129205129982,-0.126562712056682,
3.48154148211247));
#31573=CARTESIAN_POINT('Ctrl Pts',(0.0368319306580732,-0.128134782957373,
3.48417389362108));
#31574=CARTESIAN_POINT('Ctrl Pts',(0.0792962315276452,-0.107178474591724,
3.48680630512969));
#31575=CARTESIAN_POINT('Ctrl Pts',(0.103361923070995,-0.0731935540746058,
3.4894387166383));
#31576=CARTESIAN_POINT('Ctrl Pts',(0.127427614614345,-0.0392086335574879,
3.49207112814691));
#31577=CARTESIAN_POINT('Ctrl Pts',(0.133094696831473,0.00780489911109889,
3.49470353965553));
#31578=CARTESIAN_POINT('Ctrl Pts',(0.117794195954941,0.0465350563376696,
3.49733595116414));
#31579=CARTESIAN_POINT('Ctrl Pts',(0.102493695078409,0.0852652135642405,
3.49996836267275));
#31580=CARTESIAN_POINT('Ctrl Pts',(0.0662256111082176,0.115711995348795,
3.50260077418136));
#31581=CARTESIAN_POINT('Ctrl Pts',(0.0254308018677658,0.124073556121702,
3.50523318568997));
#31582=CARTESIAN_POINT('Ctrl Pts',(-0.0153640073726858,0.13243511689461,
3.50786559719859));
#31583=CARTESIAN_POINT('Ctrl Pts',(-0.0606855418833975,0.118711456655871,
3.5104980087072));
#31584=CARTESIAN_POINT('Ctrl Pts',(-0.0899888963160071,0.0891234688732135,
3.51313042021581));
#31585=CARTESIAN_POINT('Ctrl Pts',(-0.113037365625426,0.0658511220193964,
3.51520093593118));
#31586=CARTESIAN_POINT('Ctrl Pts',(-0.12617608552629,0.032764207609907,
3.51727145164656));
#31587=CARTESIAN_POINT('Ctrl Pts',(-0.126474550616365,-0.00011099430647141,
3.51934196736194));
#31588=CARTESIAN_POINT('Origin',(0.,0.,3.1));
#31589=CARTESIAN_POINT('',(-0.126585968300139,7.56654190205152E-5,3.56934196736194));
#31590=CARTESIAN_POINT('',(-0.126320239448181,8.84447983197572E-5,3.55565803263806));
#31591=CARTESIAN_POINT('',(-0.12645,1.54856587752183E-17,3.1));
#31592=CARTESIAN_POINT('',(0.0958116152722374,0.0825211298936506,3.6));
#31593=CARTESIAN_POINT('Ctrl Pts',(-0.126585968300139,7.56654190205153E-5,
3.56934196736194));
#31594=CARTESIAN_POINT('Ctrl Pts',(-0.126314022279117,-0.0367013527487602,
3.57166407704879));
#31595=CARTESIAN_POINT('Ctrl Pts',(-0.109347743467702,-0.0736867832767084,
3.57398618673564));
#31596=CARTESIAN_POINT('Ctrl Pts',(-0.0811433985852254,-0.0972323262171825,
3.57630829642249));
#31597=CARTESIAN_POINT('Ctrl Pts',(-0.0491701276919849,-0.123924242866945,
3.57894070793111));
#31598=CARTESIAN_POINT('Ctrl Pts',(-0.00275464590947525,-0.133344354062013,
3.58157311943972));
#31599=CARTESIAN_POINT('Ctrl Pts',(0.0370665801591162,-0.121131220741312,
3.58420553094833));
#31600=CARTESIAN_POINT('Ctrl Pts',(0.0768878062277077,-0.108918087420612,
3.58683794245694));
#31601=CARTESIAN_POINT('Ctrl Pts',(0.110114776582381,-0.0750717095841421,
3.58947035396555));
#31602=CARTESIAN_POINT('Ctrl Pts',(0.121670197120012,-0.035135491975585,
3.59210276547417));
#31603=CARTESIAN_POINT('Ctrl Pts',(0.133225617657642,0.004800725632972,
3.59473517698278));
#31604=CARTESIAN_POINT('Ctrl Pts',(0.12310948837823,0.0508267830136165,
3.59736758849139));
#31605=CARTESIAN_POINT('Ctrl Pts',(0.0958116152722374,0.0825211298936506,
3.6));
#31606=CARTESIAN_POINT('',(-0.0959914412498779,0.0826500850312143,3.6));
#31607=CARTESIAN_POINT('Origin',(0.,0.,3.6));
#31608=CARTESIAN_POINT('Ctrl Pts',(-0.0959917963302685,0.0826503396631676,
3.6));
#31609=CARTESIAN_POINT('Ctrl Pts',(-0.0697118464080321,0.11301028941478,
3.59746250047314));
#31610=CARTESIAN_POINT('Ctrl Pts',(-0.0277082920252644,0.129939468632456,
3.59492500094628));
#31611=CARTESIAN_POINT('Ctrl Pts',(0.0122513409849536,0.126048715034846,
3.59238750141942));
#31612=CARTESIAN_POINT('Ctrl Pts',(0.0537056138636675,0.122012432687161,
3.58975508991081));
#31613=CARTESIAN_POINT('Ctrl Pts',(0.0929602052199782,0.095569602745952,
3.5871226784022));
#31614=CARTESIAN_POINT('Ctrl Pts',(0.112244799198078,0.058668125616663,
3.58449026689359));
#31615=CARTESIAN_POINT('Ctrl Pts',(0.131529393176178,0.0217666484873742,
3.58185785538498));
#31616=CARTESIAN_POINT('Ctrl Pts',(0.130843989776067,-0.0255934758299944,
3.57922544387636));
#31617=CARTESIAN_POINT('Ctrl Pts',(0.11048667870984,-0.0619230812123589,
3.57659303236775));
#31618=CARTESIAN_POINT('Ctrl Pts',(0.0901293676436137,-0.0982526865947235,
3.57396062085914));
#31619=CARTESIAN_POINT('Ctrl Pts',(0.0501001489112715,-0.123551773042084,
3.57132820935053));
#31620=CARTESIAN_POINT('Ctrl Pts',(0.00855140333287623,-0.126362339932449,
3.56869579784192));
#31621=CARTESIAN_POINT('Ctrl Pts',(-0.032997342245519,-0.129172906822815,
3.5660633863333));
#31622=CARTESIAN_POINT('Ctrl Pts',(-0.0760656146699672,-0.109494954156186,
3.56343097482469));
#31623=CARTESIAN_POINT('Ctrl Pts',(-0.101133339862815,-0.0762433587436205,
3.56079856331608));
#31624=CARTESIAN_POINT('Ctrl Pts',(-0.117450622825668,-0.0545989659182217,
3.55908505309007));
#31625=CARTESIAN_POINT('Ctrl Pts',(-0.126140944400475,-0.0272033229899018,
3.55737154286407));
#31626=CARTESIAN_POINT('Ctrl Pts',(-0.126320239448181,8.84447983197572E-5,
3.55565803263806));
#31627=CARTESIAN_POINT('Origin',(0.,0.,3.71042117235887));
#31628=CARTESIAN_POINT('',(-0.154532329218545,4.4775541170855E-5,2.73957882764113));
#31629=CARTESIAN_POINT('',(-0.154050519949587,1.7733618556367E-5,2.73542117235887));
#31630=CARTESIAN_POINT('',(-0.1543,1.43283619370552E-14,3.71042117235887));
#31631=CARTESIAN_POINT('',(0.03985138418574,-0.149064942821847,2.7));
#31632=CARTESIAN_POINT('Ctrl Pts',(-0.154050519949587,1.77336185563769E-5,
2.73542117235887));
#31633=CARTESIAN_POINT('Ctrl Pts',(-0.154066274679179,0.0248826176783822,
2.73414376094036));
#31634=CARTESIAN_POINT('Ctrl Pts',(-0.136678442565,0.100960491967761,2.73023393801324));
#31635=CARTESIAN_POINT('Ctrl Pts',(-0.0176337922607613,0.181151847216363,
2.72369170357751));
#31636=CARTESIAN_POINT('Ctrl Pts',(0.14217180017934,0.113903091069576,2.71579446905167));
#31637=CARTESIAN_POINT('Ctrl Pts',(0.172848115381474,-0.0569943527276058,
2.70789723452584));
#31638=CARTESIAN_POINT('Ctrl Pts',(0.0891618565332066,-0.135882161272415,
2.70263241150861));
#31639=CARTESIAN_POINT('Ctrl Pts',(0.0398513841857358,-0.149064942821848,
2.7));
#31640=CARTESIAN_POINT('',(-0.0398513841857137,-0.149064942821854,2.7));
#31641=CARTESIAN_POINT('Origin',(0.,0.,2.7));
#31642=CARTESIAN_POINT('Ctrl Pts',(-0.154532329218545,4.47755411708581E-5,
2.73957882764113));
#31643=CARTESIAN_POINT('Ctrl Pts',(-0.154541474731814,0.00247370285197769,
2.73945303065539));
#31644=CARTESIAN_POINT('Ctrl Pts',(-0.153393280968798,0.0557210645369631,
2.73669482216104));
#31645=CARTESIAN_POINT('Ctrl Pts',(-0.0921890914137533,0.156981837366664,
2.73130420215808));
#31646=CARTESIAN_POINT('Ctrl Pts',(0.081054919689294,0.163034936656946,
2.72340696763225));
#31647=CARTESIAN_POINT('Ctrl Pts',(0.180814453969382,0.0212164304176998,
2.71550973310641));
#31648=CARTESIAN_POINT('Ctrl Pts',(0.117409156055766,-0.137788854076994,
2.70770741056233));
#31649=CARTESIAN_POINT('Ctrl Pts',(0.00742265010309158,-0.161856516962739,
2.70253749952686));
#31650=CARTESIAN_POINT('Ctrl Pts',(-0.0399441884684105,-0.149319082708151,
2.7));
#31651=CARTESIAN_POINT('Origin',(0.,0.,3.71042117235887));
#31652=CARTESIAN_POINT('',(-0.154111134012939,9.12056675990702E-5,2.78957882764113));
#31653=CARTESIAN_POINT('',(-0.154375356381381,-0.000128347871137961,2.78542117235887));
#31654=CARTESIAN_POINT('',(-0.1543,1.43283619370552E-14,3.71042117235887));
#31655=CARTESIAN_POINT('Ctrl Pts',(-0.154375356381381,-0.000128347871137957,
2.78542117235887));
#31656=CARTESIAN_POINT('Ctrl Pts',(-0.154004490723256,0.0414883916240874,
2.78327156332537));
#31657=CARTESIAN_POINT('Ctrl Pts',(-0.115247407249284,0.134678118697344,
2.77848954278325));
#31658=CARTESIAN_POINT('Ctrl Pts',(0.0418557848916964,0.17717956471448,
2.77107511073252));
#31659=CARTESIAN_POINT('Ctrl Pts',(0.171243621830244,0.0618160489303277,
2.76317787620668));
#31660=CARTESIAN_POINT('Ctrl Pts',(0.145372553280857,-0.109598760687136,
2.75528064168085));
#31661=CARTESIAN_POINT('Ctrl Pts',(-0.0122890050489303,-0.181634550845065,
2.74738340715501));
#31662=CARTESIAN_POINT('Ctrl Pts',(-0.13512250192602,-0.104001863717814,
2.74076358404769));
#31663=CARTESIAN_POINT('Ctrl Pts',(-0.154033808293727,-0.0263574182340484,
2.73677617244897));
#31664=CARTESIAN_POINT('Ctrl Pts',(-0.154050519949587,1.77336185563769E-5,
2.73542117235887));
#31665=CARTESIAN_POINT('Ctrl Pts',(-0.154111134012939,9.12056675990824E-5,
2.78957882764113));
#31666=CARTESIAN_POINT('Ctrl Pts',(-0.154216904845773,0.0194969338944761,
2.7885808330404));
#31667=CARTESIAN_POINT('Ctrl Pts',(-0.141845660080373,0.0899592653630177,
2.78495042693105));
#31668=CARTESIAN_POINT('Ctrl Pts',(-0.0365555263461618,0.178349534836247,
2.7786876093131));
#31669=CARTESIAN_POINT('Ctrl Pts',(0.129354617910885,0.128110846926664,
2.77079037478726));
#31670=CARTESIAN_POINT('Ctrl Pts',(0.177988125847537,-0.0382780523762908,
2.76289314026143));
#31671=CARTESIAN_POINT('Ctrl Pts',(0.0652523050728403,-0.169960699505811,
2.75499590573559));
#31672=CARTESIAN_POINT('Ctrl Pts',(-0.10390483603623,-0.147913217635949,
2.74722446819549));
#31673=CARTESIAN_POINT('Ctrl Pts',(-0.154350096899974,-0.0483537169716228,
2.742085442164));
#31674=CARTESIAN_POINT('Ctrl Pts',(-0.154532329218545,4.47755411708581E-5,
2.73957882764113));
#31675=CARTESIAN_POINT('Origin',(0.,0.,3.71042117235887));
#31676=CARTESIAN_POINT('',(-0.154217143654561,-0.000131209131675823,2.83957882764113));
#31677=CARTESIAN_POINT('',(-0.154426485097132,0.00011404955978979,2.83542117235887));
#31678=CARTESIAN_POINT('',(-0.1543,1.43283619370552E-14,3.71042117235887));
#31679=CARTESIAN_POINT('Ctrl Pts',(-0.154426485097132,0.000114049559789811,
2.83542117235887));
#31680=CARTESIAN_POINT('Ctrl Pts',(-0.154488936846892,0.00764629898056818,
2.83503177721898));
#31681=CARTESIAN_POINT('Ctrl Pts',(-0.15057776842572,0.0660334076153961,
2.83200997057048));
#31682=CARTESIAN_POINT('Ctrl Pts',(-0.0761594594163292,0.165362226259928,
2.82635575241337));
#31683=CARTESIAN_POINT('Ctrl Pts',(0.0968288057644592,0.154172306963803,
2.81845851788754));
#31684=CARTESIAN_POINT('Ctrl Pts',(0.182029287997112,0.0032053357021354,
2.8105612833617));
#31685=CARTESIAN_POINT('Ctrl Pts',(0.102196604793212,-0.150667825661861,
2.80266404883587));
#31686=CARTESIAN_POINT('Ctrl Pts',(-0.0702903425019912,-0.167940860695529,
2.79476681431002));
#31687=CARTESIAN_POINT('Ctrl Pts',(-0.14944611336054,-0.069697339741445,
2.7890191888177));
#31688=CARTESIAN_POINT('Ctrl Pts',(-0.154458652857569,-0.00947547310228015,
2.78590397483398));
#31689=CARTESIAN_POINT('Ctrl Pts',(-0.154375356381381,-0.000128347871137957,
2.78542117235887));
#31690=CARTESIAN_POINT('Ctrl Pts',(-0.154217143654561,-0.000131209131675806,
2.83957882764113));
#31691=CARTESIAN_POINT('Ctrl Pts',(-0.153918019192818,0.0361710755121499,
2.8377086354254));
#31692=CARTESIAN_POINT('Ctrl Pts',(-0.123049963751881,0.124029060195803,
2.83320603170106));
#31693=CARTESIAN_POINT('Ctrl Pts',(0.0229951363840201,0.180599411232496,
2.82607101646811));
#31694=CARTESIAN_POINT('Ctrl Pts',(0.163793876249876,0.0794763606914083,
2.81817378194228));
#31695=CARTESIAN_POINT('Ctrl Pts',(0.1560922965942,-0.0937023067775016,
2.81027654741644));
#31696=CARTESIAN_POINT('Ctrl Pts',(0.00687287227597422,-0.181927677084725,
2.8023793128906));
#31697=CARTESIAN_POINT('Ctrl Pts',(-0.128932992743455,-0.114906920263654,
2.7954800729655));
#31698=CARTESIAN_POINT('Ctrl Pts',(-0.153937912998098,-0.0316895778160955,
2.79121324454901));
#31699=CARTESIAN_POINT('Ctrl Pts',(-0.154111134012939,9.12056675990824E-5,
2.78957882764113));
#31700=CARTESIAN_POINT('Origin',(0.,0.,3.71042117235887));
#31701=CARTESIAN_POINT('',(-0.154535784933253,3.81877733398595E-5,2.88957882764113));
#31702=CARTESIAN_POINT('',(-0.154054921884602,1.70237768407695E-5,2.88542117235887));
#31703=CARTESIAN_POINT('',(-0.1543,1.43283619370552E-14,3.71042117235887));
#31704=CARTESIAN_POINT('Ctrl Pts',(-0.154054921884602,1.70237768407841E-5,
2.88542117235887));
#31705=CARTESIAN_POINT('Ctrl Pts',(-0.154079346410273,0.0245707720672152,
2.88415957960399));
#31706=CARTESIAN_POINT('Ctrl Pts',(-0.1369997697474,0.100325734672348,2.88026557534049));
#31707=CARTESIAN_POINT('Ctrl Pts',(-0.0186809878927599,0.181096514045709,
2.87373915956839));
#31708=CARTESIAN_POINT('Ctrl Pts',(0.14142638889208,0.114645117640021,2.86584192504255));
#31709=CARTESIAN_POINT('Ctrl Pts',(0.173312464619039,-0.0557468952238434,
2.85794469051671));
#31710=CARTESIAN_POINT('Ctrl Pts',(0.0480683875166603,-0.175597144601074,
2.85004745599088));
#31711=CARTESIAN_POINT('Ctrl Pts',(-0.112431541495112,-0.138186203572753,
2.84253961660493));
#31712=CARTESIAN_POINT('Ctrl Pts',(-0.154066746922155,-0.0432736484708866,
2.8376641887276));
#31713=CARTESIAN_POINT('Ctrl Pts',(-0.154426485097132,0.000114049559789811,
2.83542117235887));
#31714=CARTESIAN_POINT('Ctrl Pts',(-0.154535784933253,3.8187773339879E-5,
2.88957882764113));
#31715=CARTESIAN_POINT('Ctrl Pts',(-0.154542902681706,0.00216158596911697,
2.88946884931902));
#31716=CARTESIAN_POINT('Ctrl Pts',(-0.153545003294962,0.0551032333888324,
2.8867264594883));
#31717=CARTESIAN_POINT('Ctrl Pts',(-0.0931239936920636,0.15643799622185,
2.88135165814895));
#31718=CARTESIAN_POINT('Ctrl Pts',(0.080081970475175,0.163498632518342,
2.87345442362313));
#31719=CARTESIAN_POINT('Ctrl Pts',(0.180683277203119,0.0223266252501708,
2.86555718909729));
#31720=CARTESIAN_POINT('Ctrl Pts',(0.11747183849698,-0.139087354145018,
2.85765995457145));
#31721=CARTESIAN_POINT('Ctrl Pts',(-0.0522430059551858,-0.174400668051551,
2.84976272004562));
#31722=CARTESIAN_POINT('Ctrl Pts',(-0.145618409602951,-0.0806790644135928,
2.84373567773551));
#31723=CARTESIAN_POINT('Ctrl Pts',(-0.154339055420526,-0.0149266411191706,
2.84034104693401));
#31724=CARTESIAN_POINT('Ctrl Pts',(-0.154217143654561,-0.000131209131675806,
2.83957882764113));
#31725=CARTESIAN_POINT('Origin',(0.,0.,3.71042117235887));
#31726=CARTESIAN_POINT('',(-0.154116825055928,9.48496454908493E-5,2.93957882764113));
#31727=CARTESIAN_POINT('',(-0.154366358871002,-0.000130096805920683,2.93542117235887));
#31728=CARTESIAN_POINT('',(-0.1543,1.43283619370552E-14,3.71042117235887));
#31729=CARTESIAN_POINT('Ctrl Pts',(-0.154366358871002,-0.000130096805920679,
2.93542117235887));
#31730=CARTESIAN_POINT('Ctrl Pts',(-0.153995797272422,0.0411865074797718,
2.93328738198899));
#31731=CARTESIAN_POINT('Ctrl Pts',(-0.115714146224304,0.134080683615333,
2.9285211801105));
#31732=CARTESIAN_POINT('Ctrl Pts',(0.0407990816336726,0.177427059877793,
2.9211225667234));
#31733=CARTESIAN_POINT('Ctrl Pts',(0.170870699467283,0.0628341523235889,
2.91322533219756));
#31734=CARTESIAN_POINT('Ctrl Pts',(0.146025941933673,-0.108726036068736,
2.90532809767173));
#31735=CARTESIAN_POINT('Ctrl Pts',(-0.0112102069433731,-0.181712019164164,
2.89743086314589));
#31736=CARTESIAN_POINT('Ctrl Pts',(-0.134787821110527,-0.104611252124613,
2.89079522137494));
#31737=CARTESIAN_POINT('Ctrl Pts',(-0.154028382735806,-0.026662535455284,
2.8867919911126));
#31738=CARTESIAN_POINT('Ctrl Pts',(-0.154054921884602,1.70237768407841E-5,
2.88542117235887));
#31739=CARTESIAN_POINT('Ctrl Pts',(-0.154116825055928,9.48496454908822E-5,
2.93957882764113));
#31740=CARTESIAN_POINT('Ctrl Pts',(-0.154225358468008,0.0191912107511692,
2.93859665170402));
#31741=CARTESIAN_POINT('Ctrl Pts',(-0.1421149984489,0.0893365787084054,
2.93498206425831));
#31742=CARTESIAN_POINT('Ctrl Pts',(-0.0376184643267171,0.178128537842515,
2.92873506530397));
#31743=CARTESIAN_POINT('Ctrl Pts',(0.128588348481182,0.128879639534425,
2.92083783077814));
#31744=CARTESIAN_POINT('Ctrl Pts',(0.178213202383553,-0.0372153106656781,
2.9129405962523));
#31745=CARTESIAN_POINT('Ctrl Pts',(0.0662647529343645,-0.169569771398652,
2.90504336172647));
#31746=CARTESIAN_POINT('Ctrl Pts',(-0.10336559476711,-0.148485092132862,
2.89725610552274));
#31747=CARTESIAN_POINT('Ctrl Pts',(-0.154372534171041,-0.0486635015632469,
2.89210126082763));
#31748=CARTESIAN_POINT('Ctrl Pts',(-0.154535784933253,3.8187773339879E-5,
2.88957882764113));
#31749=CARTESIAN_POINT('Origin',(0.,0.,3.71042117235887));
#31750=CARTESIAN_POINT('',(-0.154208836002914,-0.000129626704909153,2.98957882764113));
#31751=CARTESIAN_POINT('',(-0.154434696759477,0.000111004303427491,2.98542117235887));
#31752=CARTESIAN_POINT('',(-0.1543,1.43283619370552E-14,3.71042117235887));
#31753=CARTESIAN_POINT('Ctrl Pts',(-0.154434696759477,0.000111004303427509,
2.98542117235887));
#31754=CARTESIAN_POINT('Ctrl Pts',(-0.15449350107168,0.00733626390374423,
2.98504759588261));
#31755=CARTESIAN_POINT('Ctrl Pts',(-0.150762340620084,0.0654133961639385,
2.98204160789773));
#31756=CARTESIAN_POINT('Ctrl Pts',(-0.0771442428547834,0.164905101290741,
2.97640320840425));
#31757=CARTESIAN_POINT('Ctrl Pts',(0.0959076962473017,0.15474702077238,
2.96850597387841));
#31758=CARTESIAN_POINT('Ctrl Pts',(0.182006911912947,0.00429076371209153,
2.96060873935257));
#31759=CARTESIAN_POINT('Ctrl Pts',(0.103093336173269,-0.150055625266004,
2.95271150482674));
#31760=CARTESIAN_POINT('Ctrl Pts',(-0.069287674394006,-0.168357194128057,
2.9448142703009));
#31761=CARTESIAN_POINT('Ctrl Pts',(-0.14924717784082,-0.0703180680940833,
2.93905082614495));
#31762=CARTESIAN_POINT('Ctrl Pts',(-0.154452951185252,-0.00978490290509501,
2.9359197934976));
#31763=CARTESIAN_POINT('Ctrl Pts',(-0.154366358871002,-0.000130096805920679,
2.93542117235887));
#31764=CARTESIAN_POINT('Ctrl Pts',(-0.154208836002914,-0.00012962670490916,
2.98957882764113));
#31765=CARTESIAN_POINT('Ctrl Pts',(-0.15391701905173,0.0358705210125992,
2.98772445408903));
#31766=CARTESIAN_POINT('Ctrl Pts',(-0.123464382903156,0.123420397725162,
2.98323766902831));
#31767=CARTESIAN_POINT('Ctrl Pts',(0.0219177299165732,0.180733333857582,
2.97611847245899));
#31768=CARTESIAN_POINT('Ctrl Pts',(0.163317009898163,0.0804517192475515,
2.96822123793315));
#31769=CARTESIAN_POINT('Ctrl Pts',(0.156648310460303,-0.0927697778475837,
2.96032400340732));
#31770=CARTESIAN_POINT('Ctrl Pts',(0.00795766962277319,-0.181883480135435,
2.95242676888148));
#31771=CARTESIAN_POINT('Ctrl Pts',(-0.128557747147415,-0.11552191978543,
2.94551171029275));
#31772=CARTESIAN_POINT('Ctrl Pts',(-0.1539344690334,-0.0319905366812824,
2.94122906321263));
#31773=CARTESIAN_POINT('Ctrl Pts',(-0.154116825055928,9.48496454908822E-5,
2.93957882764113));
#31774=CARTESIAN_POINT('Origin',(0.,0.,3.71042117235887));
#31775=CARTESIAN_POINT('',(-0.154538871978598,3.2832780837988E-5,3.03957882764113));
#31776=CARTESIAN_POINT('',(-0.154056089165245,2.19184202627989E-5,3.03542117235887));
#31777=CARTESIAN_POINT('',(-0.1543,1.43283619370552E-14,3.71042117235887));
#31778=CARTESIAN_POINT('Ctrl Pts',(-0.154056089165245,2.19184202628134E-5,
3.03542117235887));
#31779=CARTESIAN_POINT('Ctrl Pts',(-0.154087155299894,0.0242673368387721,
3.03417539826761));
#31780=CARTESIAN_POINT('Ctrl Pts',(-0.137310014833352,0.0997044362362006,
3.03029721266774));
#31781=CARTESIAN_POINT('Ctrl Pts',(-0.0197606177252597,0.180981890321858,
3.02378661555926));
#31782=CARTESIAN_POINT('Ctrl Pts',(0.140740192743497,0.115486470133437,
3.01588938103343));
#31783=CARTESIAN_POINT('Ctrl Pts',(0.173641826766224,-0.0547123627222005,
3.00799214650759));
#31784=CARTESIAN_POINT('Ctrl Pts',(0.0491147003187017,-0.175307366787479,
3.00009491198175));
#31785=CARTESIAN_POINT('Ctrl Pts',(-0.11194410582055,-0.138777425062269,
2.99257125393218));
#31786=CARTESIAN_POINT('Ctrl Pts',(-0.15407913571938,-0.0435766220328422,
2.98768000739122));
#31787=CARTESIAN_POINT('Ctrl Pts',(-0.154434696759477,0.000111004303427509,
2.98542117235887));
#31788=CARTESIAN_POINT('Ctrl Pts',(-0.154538871978598,3.28327808380407E-5,
3.03957882764113));
#31789=CARTESIAN_POINT('Ctrl Pts',(-0.154544182685759,0.00185071603346938,
3.03948466798264));
#31790=CARTESIAN_POINT('Ctrl Pts',(-0.153694834634547,0.0544858891421056,
3.03675809681555));
#31791=CARTESIAN_POINT('Ctrl Pts',(-0.0940552495850459,0.15587987322763,
3.03139911413983));
#31792=CARTESIAN_POINT('Ctrl Pts',(0.0791055288760802,0.163973290975094,
3.02350187961401));
#31793=CARTESIAN_POINT('Ctrl Pts',(0.180546920428939,0.0234037256776295,
3.01560464508816));
#31794=CARTESIAN_POINT('Ctrl Pts',(0.118299191571216,-0.138384342053441,
3.00770741056233));
#31795=CARTESIAN_POINT('Ctrl Pts',(-0.0512020455023775,-0.174709116500372,
2.99981017603649));
#31796=CARTESIAN_POINT('Ctrl Pts',(-0.145381230907426,-0.0813015016053826,
2.99376731506276));
#31797=CARTESIAN_POINT('Ctrl Pts',(-0.154331273396456,-0.0152341784994835,
2.99035686559764));
#31798=CARTESIAN_POINT('Ctrl Pts',(-0.154208836002914,-0.00012962670490916,
2.98957882764113));
#31799=CARTESIAN_POINT('Origin',(0.,0.,3.71042117235887));
#31800=CARTESIAN_POINT('',(-0.154122750472518,9.83954699399631E-5,3.08957882764113));
#31801=CARTESIAN_POINT('',(-0.154357314101369,-0.000131672715837502,3.08542117235887));
#31802=CARTESIAN_POINT('',(-0.1543,1.43283619370552E-14,3.71042117235887));
#31803=CARTESIAN_POINT('Ctrl Pts',(-0.154357314101369,-0.000131672715837496,
3.08542117235887));
#31804=CARTESIAN_POINT('Ctrl Pts',(-0.153987553769485,0.0408848376338906,
3.08330320065262));
#31805=CARTESIAN_POINT('Ctrl Pts',(-0.11617759776856,0.133482913719063,
3.07855281743775));
#31806=CARTESIAN_POINT('Ctrl Pts',(0.039740276922879,0.17766720864428,3.07117002271427));
#31807=CARTESIAN_POINT('Ctrl Pts',(0.170492952144154,0.0638520156810144,
3.06327278818844));
#31808=CARTESIAN_POINT('Ctrl Pts',(0.146671728755708,-0.107853282848364,
3.0553755536626));
#31809=CARTESIAN_POINT('Ctrl Pts',(-0.0101263751692898,-0.181775639631079,
3.04747831913677));
#31810=CARTESIAN_POINT('Ctrl Pts',(-0.134457266065241,-0.105231153897523,
3.04082685870219));
#31811=CARTESIAN_POINT('Ctrl Pts',(-0.154021510291741,-0.026965000487735,
3.03680780977622));
#31812=CARTESIAN_POINT('Ctrl Pts',(-0.154056089165245,2.19184202628134E-5,
3.03542117235887));
#31813=CARTESIAN_POINT('Ctrl Pts',(-0.154122750472518,9.83954699399839E-5,
3.08957882764113));
#31814=CARTESIAN_POINT('Ctrl Pts',(-0.154233799032612,0.0188853799021587,
3.08861247036765));
#31815=CARTESIAN_POINT('Ctrl Pts',(-0.142381965748736,0.0887139061579003,
3.08501370158555));
#31816=CARTESIAN_POINT('Ctrl Pts',(-0.0386800578824722,0.177901034213339,
3.07878252129485));
#31817=CARTESIAN_POINT('Ctrl Pts',(0.127817493356429,0.129644179368171,
3.07088528676902));
#31818=CARTESIAN_POINT('Ctrl Pts',(0.178431965499368,-0.0361518815554529,
3.06298805224317));
#31819=CARTESIAN_POINT('Ctrl Pts',(0.0672747972491473,-0.169171588947593,
3.05509081771735));
#31820=CARTESIAN_POINT('Ctrl Pts',(-0.102823100152332,-0.149058093692613,
3.04728774284999));
#31821=CARTESIAN_POINT('Ctrl Pts',(-0.154395711813265,-0.0489716517674636,
3.04211707949126));
#31822=CARTESIAN_POINT('Ctrl Pts',(-0.154538871978598,3.28327808380407E-5,
3.03957882764113));
#31823=CARTESIAN_POINT('Origin',(0.,0.,3.71042117235887));
#31824=CARTESIAN_POINT('',(-0.154200664638475,-0.000127870236170058,3.13957882764113));
#31825=CARTESIAN_POINT('',(-0.154442743231392,0.000107782702043065,3.13542117235887));
#31826=CARTESIAN_POINT('',(-0.1543,1.43283619370552E-14,3.71042117235887));
#31827=CARTESIAN_POINT('Ctrl Pts',(-0.154442743231391,0.000107782702043087,
3.13542117235887));
#31828=CARTESIAN_POINT('Ctrl Pts',(-0.154497895338046,0.00702615569019676,
3.13506341454624));
#31829=CARTESIAN_POINT('Ctrl Pts',(-0.150944880930953,0.0647935208243374,
3.13207324522499));
#31830=CARTESIAN_POINT('Ctrl Pts',(-0.0781262761399388,0.164442122383114,
3.12645066439512));
#31831=CARTESIAN_POINT('Ctrl Pts',(0.0949831631341886,0.155316210867962,
3.11855342986929));
#31832=CARTESIAN_POINT('Ctrl Pts',(0.181978087741923,0.00537607841744088,
3.11065619534345));
#31833=CARTESIAN_POINT('Ctrl Pts',(0.10398635378076,-0.149438164016893,
3.10275896081762));
#31834=CARTESIAN_POINT('Ctrl Pts',(-0.0682824508977375,-0.168767394767933,
3.09486172629178));
#31835=CARTESIAN_POINT('Ctrl Pts',(-0.14904624696594,-0.0709390773474446,
3.0890824634722));
#31836=CARTESIAN_POINT('Ctrl Pts',(-0.154447126175577,-0.0100942824218163,
3.08593561216123));
#31837=CARTESIAN_POINT('Ctrl Pts',(-0.154357314101369,-0.000131672715837496,
3.08542117235887));
#31838=CARTESIAN_POINT('Ctrl Pts',(-0.154200664638475,-0.000127870236170063,
3.13957882764113));
#31839=CARTESIAN_POINT('Ctrl Pts',(-0.153916387321455,0.03556997377657,
3.13774027275265));
#31840=CARTESIAN_POINT('Ctrl Pts',(-0.123875930184563,0.122811200111113,
3.13326930635556));
#31841=CARTESIAN_POINT('Ctrl Pts',(0.0208395441149821,0.180860825645154,
3.12616592844986));
#31842=CARTESIAN_POINT('Ctrl Pts',(0.162834335224968,0.0814242232005321,
3.11826869392403));
#31843=CARTESIAN_POINT('Ctrl Pts',(0.157198753896076,-0.0918339622660831,
3.1103714593982));
#31844=CARTESIAN_POINT('Ctrl Pts',(0.00904218304404205,-0.181832790711041,
3.10247422487235));
#31845=CARTESIAN_POINT('Ctrl Pts',(-0.128179738775568,-0.116136573115574,
3.09554334762));
#31846=CARTESIAN_POINT('Ctrl Pts',(-0.153931296515552,-0.0322914212547928,
3.09124488187626));
#31847=CARTESIAN_POINT('Ctrl Pts',(-0.154122750472518,9.83954699399839E-5,
3.08957882764113));
#31848=CARTESIAN_POINT('Origin',(0.,0.,3.71042117235887));
#31849=CARTESIAN_POINT('',(-0.154541524340359,2.74150270591633E-5,3.18957882764113));
#31850=CARTESIAN_POINT('',(-0.154057549710717,2.67855146112065E-5,3.18542117235887));
#31851=CARTESIAN_POINT('',(-0.1543,1.43283619370552E-14,3.71042117235887));
#31852=CARTESIAN_POINT('Ctrl Pts',(-0.154057549710717,2.67855146112127E-5,
3.18542117235887));
#31853=CARTESIAN_POINT('Ctrl Pts',(-0.154095052553054,0.0239637717781011,
3.18419121693124));
#31854=CARTESIAN_POINT('Ctrl Pts',(-0.137617732079011,0.0990829983563936,
3.18032884999499));
#31855=CARTESIAN_POINT('Ctrl Pts',(-0.0208395446762738,0.180860830516292,
3.17383407155014));
#31856=CARTESIAN_POINT('Ctrl Pts',(0.140048991174337,0.116323715159066,
3.1659368370243));
#31857=CARTESIAN_POINT('Ctrl Pts',(0.173965014144346,-0.0536758837012937,
3.15803960249847));
#31858=CARTESIAN_POINT('Ctrl Pts',(0.050159265511441,-0.175011355976434,
3.15014236797263));
#31859=CARTESIAN_POINT('Ctrl Pts',(-0.111453603442084,-0.139367747346172,
3.14260289125943));
#31860=CARTESIAN_POINT('Ctrl Pts',(-0.154092081585972,-0.0438798036810342,
3.13769582605485));
#31861=CARTESIAN_POINT('Ctrl Pts',(-0.154442743231391,0.000107782702043087,
3.13542117235887));
#31862=CARTESIAN_POINT('Ctrl Pts',(-0.154541524340359,2.74150270592019E-5,
3.18957882764113));
#31863=CARTESIAN_POINT('Ctrl Pts',(-0.154545265409953,0.0015398273092893,
3.18950048664627));
#31864=CARTESIAN_POINT('Ctrl Pts',(-0.153842769766794,0.0538687068697594,
3.1867897341428));
#31865=CARTESIAN_POINT('Ctrl Pts',(-0.0949831605760139,0.155316206684809,
3.18144657013072));
#31866=CARTESIAN_POINT('Ctrl Pts',(0.0781262740357409,0.164442117954189,
3.17354933560488));
#31867=CARTESIAN_POINT('Ctrl Pts',(0.180404142828019,0.0244799939226929,
3.16565210107904));
#31868=CARTESIAN_POINT('Ctrl Pts',(0.119122337560023,-0.137676408822293,
3.15775486655321));
#31869=CARTESIAN_POINT('Ctrl Pts',(-0.0501592641604809,-0.175011351262844,
3.14985763202737));
#31870=CARTESIAN_POINT('Ctrl Pts',(-0.145141798308845,-0.081923988470417,
3.14379895239001));
#31871=CARTESIAN_POINT('Ctrl Pts',(-0.15432341073188,-0.0155415899851509,
3.14037268426126));
#31872=CARTESIAN_POINT('Ctrl Pts',(-0.154200664638475,-0.000127870236170063,
3.13957882764113));
#31873=CARTESIAN_POINT('Origin',(0.,0.,3.71042117235887));
#31874=CARTESIAN_POINT('',(-0.154128903346263,0.000101814369117867,3.23957882764113));
#31875=CARTESIAN_POINT('',(-0.15434822268538,-0.000133055250486845,3.23542117235887));
#31876=CARTESIAN_POINT('',(-0.1543,1.43283619370552E-14,3.71042117235887));
#31877=CARTESIAN_POINT('Ctrl Pts',(-0.15434822268538,-0.00013305525048684,
3.23542117235887));
#31878=CARTESIAN_POINT('Ctrl Pts',(-0.153979802923996,0.0405832940781535,
3.23331901931624));
#31879=CARTESIAN_POINT('Ctrl Pts',(-0.116638046803031,0.132884381239301,
3.228584454765));
#31880=CARTESIAN_POINT('Ctrl Pts',(0.0386800589242284,0.177901039004767,
3.22121747870515));
#31881=CARTESIAN_POINT('Ctrl Pts',(0.170109141545278,0.0648676082500797,
3.21332024417931));
#31882=CARTESIAN_POINT('Ctrl Pts',(0.147312299474883,-0.106976694007524,
3.20542300965349));
#31883=CARTESIAN_POINT('Ctrl Pts',(-0.00904218328755787,-0.18183279560836,
3.19752577512764));
#31884=CARTESIAN_POINT('Ctrl Pts',(-0.134124100441736,-0.105850839905797,
3.19085849602944));
#31885=CARTESIAN_POINT('Ctrl Pts',(-0.154014787112897,-0.0272673514852388,
3.18682362843985));
#31886=CARTESIAN_POINT('Ctrl Pts',(-0.154057549710717,2.67855146112127E-5,
3.18542117235887));
#31887=CARTESIAN_POINT('Ctrl Pts',(-0.154128903346263,0.000101814369117853,
3.23957882764113));
#31888=CARTESIAN_POINT('Ctrl Pts',(-0.15424221981892,0.0185794122284465,
3.23862828903127));
#31889=CARTESIAN_POINT('Ctrl Pts',(-0.142646569905461,0.0880912185498955,
3.23504533891281));
#31890=CARTESIAN_POINT('Ctrl Pts',(-0.0397402758525677,0.177667203859151,
3.22882997728572));
#31891=CARTESIAN_POINT('Ctrl Pts',(0.127042092635782,0.130404108641901,
3.22093274275989));
#31892=CARTESIAN_POINT('Ctrl Pts',(0.178644383007786,-0.0350871667669908,
3.21303550823405));
#31893=CARTESIAN_POINT('Ctrl Pts',(0.0682824490586963,-0.1687673902225,
3.20513827370822));
#31894=CARTESIAN_POINT('Ctrl Pts',(-0.102277435139451,-0.149629907004419,
3.19731938017724));
#31895=CARTESIAN_POINT('Ctrl Pts',(-0.154419558113643,-0.0492801999911546,
3.19213289815488));
#31896=CARTESIAN_POINT('Ctrl Pts',(-0.154541524340359,2.74150270592019E-5,
3.18957882764113));
#31897=CARTESIAN_POINT('Origin',(0.,0.,3.71042117235887));
#31898=CARTESIAN_POINT('',(-0.154192638571573,-0.000125942848695916,3.28957882764113));
#31899=CARTESIAN_POINT('',(-0.154450609193756,0.000104390085258889,3.28542117235887));
#31900=CARTESIAN_POINT('',(-0.1543,1.43283619370552E-14,3.71042117235887));
#31901=CARTESIAN_POINT('Ctrl Pts',(-0.154450609193756,0.000104390085258887,
3.28542117235887));
#31902=CARTESIAN_POINT('Ctrl Pts',(-0.154502116257734,0.0067159788236037,
3.28507923320986));
#31903=CARTESIAN_POINT('Ctrl Pts',(-0.151125396911172,0.064173784678776,
3.28210488255223));
#31904=CARTESIAN_POINT('Ctrl Pts',(-0.0791055310066521,0.163973295391393,
3.27649812038601));
#31905=CARTESIAN_POINT('Ctrl Pts',(0.0940552521182287,0.155879877425964,
3.26860088586016));
#31906=CARTESIAN_POINT('Ctrl Pts',(0.181942791852133,0.00646120193221371,
3.26070365133433));
#31907=CARTESIAN_POINT('Ctrl Pts',(0.104875673303493,-0.148815388271832,
3.25280641680849));
#31908=CARTESIAN_POINT('Ctrl Pts',(-0.067274799061048,-0.169171593503912,
3.24490918228266));
#31909=CARTESIAN_POINT('Ctrl Pts',(-0.148843209204449,-0.0715602003700874,
3.23911410079945));
#31910=CARTESIAN_POINT('Ctrl Pts',(-0.154441154880871,-0.0104035676716175,
3.23595143082485));
#31911=CARTESIAN_POINT('Ctrl Pts',(-0.15434822268538,-0.00013305525048684,
3.23542117235887));
#31912=CARTESIAN_POINT('Ctrl Pts',(-0.154192638571573,-0.000125942848695916,
3.28957882764113));
#31913=CARTESIAN_POINT('Ctrl Pts',(-0.153916116413885,0.0352694274746551,
3.28775609141628));
#31914=CARTESIAN_POINT('Ctrl Pts',(-0.124284613860796,0.122201478629219,
3.28330094368282));
#31915=CARTESIAN_POINT('Ctrl Pts',(0.0197606171930289,0.18098188544746,
3.27621338444074));
#31916=CARTESIAN_POINT('Ctrl Pts',(0.162345869645737,0.0823938314495476,
3.26831614991491));
#31917=CARTESIAN_POINT('Ctrl Pts',(0.157743606844976,-0.0908948807772195,
3.26041891538907));
#31918=CARTESIAN_POINT('Ctrl Pts',(0.0101263748965706,-0.181775634735301,
3.25252168086324));
#31919=CARTESIAN_POINT('Ctrl Pts',(-0.127798960265965,-0.1167508316284,
3.24557498494725));
#31920=CARTESIAN_POINT('Ctrl Pts',(-0.153928402385683,-0.0325922506078629,
3.24126070053988));
#31921=CARTESIAN_POINT('Ctrl Pts',(-0.154128903346263,0.000101814369117853,
3.23957882764113));
#31922=CARTESIAN_POINT('Origin',(0.,0.,3.71042117235887));
#31923=CARTESIAN_POINT('',(-0.154543726005254,2.19441315424396E-5,3.33957882764113));
#31924=CARTESIAN_POINT('',(-0.154059302102979,3.16189515402649E-5,3.33542117235887));
#31925=CARTESIAN_POINT('',(-0.1543,1.43283619370552E-14,3.71042117235887));
#31926=CARTESIAN_POINT('Ctrl Pts',(-0.154059302102979,3.16189515402656E-5,
3.33542117235887));
#31927=CARTESIAN_POINT('Ctrl Pts',(-0.15410303154311,0.0236600756904899,
3.33420703559487));
#31928=CARTESIAN_POINT('Ctrl Pts',(-0.137922930779561,0.0984614290803482,
3.33036048732225));
#31929=CARTESIAN_POINT('Ctrl Pts',(-0.0219177305069036,0.180733338725286,
3.32388152754101));
#31930=CARTESIAN_POINT('Ctrl Pts',(0.139352809018331,0.117156823343995,
3.31598429301518));
#31931=CARTESIAN_POINT('Ctrl Pts',(0.174282014774141,-0.0526374957955154,
3.30808705848934));
#31932=CARTESIAN_POINT('Ctrl Pts',(0.0512020468814229,-0.174709121205821,
3.3001898239635));
#31933=CARTESIAN_POINT('Ctrl Pts',(-0.110960029365619,-0.139957157472604,
3.29263452858669));
#31934=CARTESIAN_POINT('Ctrl Pts',(-0.154105590184654,-0.0441832011483282,
3.28771164471847));
#31935=CARTESIAN_POINT('Ctrl Pts',(-0.154450609193756,0.000104390085258887,
3.28542117235887));
#31936=CARTESIAN_POINT('Ctrl Pts',(-0.154543726005254,2.19441315424298E-5,
3.33957882764113));
#31937=CARTESIAN_POINT('Ctrl Pts',(-0.154546150302478,0.00122892294348618,
3.33951630530989));
#31938=CARTESIAN_POINT('Ctrl Pts',(-0.153988815888461,0.0532516871969489,
3.33682137147005));
#31939=CARTESIAN_POINT('Ctrl Pts',(-0.0959076936642258,0.154747016604558,
3.33149402612159));
#31940=CARTESIAN_POINT('Ctrl Pts',(0.0771442407770374,0.164905096849345,
3.32359679159575));
#31941=CARTESIAN_POINT('Ctrl Pts',(0.180254949482897,0.0255553915814562,
3.31569955706992));
#31942=CARTESIAN_POINT('Ctrl Pts',(0.119941247180243,-0.13696357938087,
3.30780232254408));
#31943=CARTESIAN_POINT('Ctrl Pts',(-0.0491146989958762,-0.175307362065916,
3.29990508801825));
#31944=CARTESIAN_POINT('Ctrl Pts',(-0.144900102757682,-0.0825465196247692,
3.29383058971726));
#31945=CARTESIAN_POINT('Ctrl Pts',(-0.154315472118983,-0.0158488741865795,
3.29038850292489));
#31946=CARTESIAN_POINT('Ctrl Pts',(-0.154192638571573,-0.000125942848695916,
3.28957882764113));
#31947=CARTESIAN_POINT('Origin',(0.,0.,3.71042117235887));
#31948=CARTESIAN_POINT('',(-0.15413527741405,0.000105101588974824,3.38957882764113));
#31949=CARTESIAN_POINT('',(-0.15433909720242,-0.000134243687139869,3.38542117235887));
#31950=CARTESIAN_POINT('',(-0.1543,1.43283619370552E-14,3.71042117235887));
#31951=CARTESIAN_POINT('Ctrl Pts',(-0.15433909720242,-0.000134243687139867,
3.38542117235887));
#31952=CARTESIAN_POINT('Ctrl Pts',(-0.153972537455045,0.0402818685502336,
3.38333483797987));
#31953=CARTESIAN_POINT('Ctrl Pts',(-0.117095500692927,0.132285100657941,
3.37861609209226));
#31954=CARTESIAN_POINT('Ctrl Pts',(0.0376184653398806,0.178128542640067,
3.37126493469602));
#31955=CARTESIAN_POINT('Ctrl Pts',(0.169719281325138,0.0658808939206553,
3.36336770017019));
#31956=CARTESIAN_POINT('Ctrl Pts',(0.14794763130091,-0.10609630073556,3.35547046564435));
#31957=CARTESIAN_POINT('Ctrl Pts',(-0.00795766983708003,-0.181883485034118,
3.34757323111852));
#31958=CARTESIAN_POINT('Ctrl Pts',(-0.133788315045723,-0.106470301039161,
3.34089013335669));
#31959=CARTESIAN_POINT('Ctrl Pts',(-0.154008220246,-0.0275695907640756,
3.33683944710348));
#31960=CARTESIAN_POINT('Ctrl Pts',(-0.154059302102979,3.16189515402656E-5,
3.33542117235887));
#31961=CARTESIAN_POINT('Ctrl Pts',(-0.15413527741405,0.000105101588974825,
3.38957882764113));
#31962=CARTESIAN_POINT('Ctrl Pts',(-0.154250615308729,0.0182733082008614,
3.3886441076949));
#31963=CARTESIAN_POINT('Ctrl Pts',(-0.142908820182152,0.0874685218643051,
3.38507697624006));
#31964=CARTESIAN_POINT('Ctrl Pts',(-0.0407990805348497,0.177427055099143,
3.3788774332766));
#31965=CARTESIAN_POINT('Ctrl Pts',(0.126262173896246,0.131159400329288,
3.37098019875077));
#31966=CARTESIAN_POINT('Ctrl Pts',(0.178850447353964,-0.0340212041663437,
3.36308296422493));
#31967=CARTESIAN_POINT('Ctrl Pts',(0.0692876725278909,-0.168357189593675,
3.3551857296991));
#31968=CARTESIAN_POINT('Ctrl Pts',(-0.101728594599068,-0.150200514568663,
3.3473510175045));
#31969=CARTESIAN_POINT('Ctrl Pts',(-0.15444407880598,-0.0495891584122831,
3.3421487168185));
#31970=CARTESIAN_POINT('Ctrl Pts',(-0.154543726005254,2.19441315424298E-5,
3.33957882764113));
#31971=CARTESIAN_POINT('Origin',(0.,0.,3.71042117235887));
#31972=CARTESIAN_POINT('',(-0.154184766718537,-0.000123847547745311,3.43957882764113));
#31973=CARTESIAN_POINT('',(-0.154458280286029,0.000100830356962909,3.43542117235887));
#31974=CARTESIAN_POINT('',(-0.1543,1.43283619370552E-14,3.71042117235887));
#31975=CARTESIAN_POINT('Ctrl Pts',(-0.154458280286029,0.000100830356962935,
3.43542117235887));
#31976=CARTESIAN_POINT('Ctrl Pts',(-0.154506161619621,0.00640573612334919,
3.43509505187348));
#31977=CARTESIAN_POINT('Ctrl Pts',(-0.151303896650316,0.0635541898545394,
3.43213651987949));
#31978=CARTESIAN_POINT('Ctrl Pts',(-0.0800819726320239,0.163498636922,3.42654557637688));
#31979=CARTESIAN_POINT('Ctrl Pts',(0.0931239962001525,0.156438000435139,
3.41864834185104));
#31980=CARTESIAN_POINT('Ctrl Pts',(0.181901025498224,0.00754609564814438,
3.41075110732521));
#31981=CARTESIAN_POINT('Ctrl Pts',(0.10576126311461,-0.148187320169658,
3.40285387279937));
#31982=CARTESIAN_POINT('Ctrl Pts',(-0.0662647547190597,-0.169569775965683,
3.39495663827354));
#31983=CARTESIAN_POINT('Ctrl Pts',(-0.148638055997427,-0.0721814340714305,
3.3891457381267));
#31984=CARTESIAN_POINT('Ctrl Pts',(-0.154435040545295,-0.0107127563084332,
3.38596724948848));
#31985=CARTESIAN_POINT('Ctrl Pts',(-0.15433909720242,-0.000134243687139867,
3.38542117235887));
#31986=CARTESIAN_POINT('Ctrl Pts',(-0.154184766718538,-0.000123847547745311,
3.43957882764113));
#31987=CARTESIAN_POINT('Ctrl Pts',(-0.153916198856604,0.0349688764624186,
3.4377719100799));
#31988=CARTESIAN_POINT('Ctrl Pts',(-0.124690442079412,0.121591245361209,
3.43333258101007));
#31989=CARTESIAN_POINT('Ctrl Pts',(0.0186809873893989,0.181096509168673,
3.42626084043161));
#31990=CARTESIAN_POINT('Ctrl Pts',(0.161851630600137,0.0833605094034181,
3.41836360590578));
#31991=CARTESIAN_POINT('Ctrl Pts',(0.158282849894819,-0.0899525667211824,
3.41046637137994));
#31992=CARTESIAN_POINT('Ctrl Pts',(0.0112102066414966,-0.181712014270169,
3.40256913685411));
#31993=CARTESIAN_POINT('Ctrl Pts',(-0.127415402859048,-0.117364684067358,
3.3956066222745));
#31994=CARTESIAN_POINT('Ctrl Pts',(-0.153925794165715,-0.032893029234098,
3.39127651920351));
#31995=CARTESIAN_POINT('Ctrl Pts',(-0.15413527741405,0.000105101588974825,
3.38957882764113));
#31996=CARTESIAN_POINT('Origin',(0.,0.,3.71042117235887));
#31997=CARTESIAN_POINT('',(-0.154545466983052,1.64397697926255E-5,3.48957882764113));
#31998=CARTESIAN_POINT('',(-0.154061344734167,3.6410572125671E-5,3.48542117235887));
#31999=CARTESIAN_POINT('',(-0.1543,1.43283619370552E-14,3.71042117235887));
#32000=CARTESIAN_POINT('Ctrl Pts',(-0.154061344734167,3.64105721256669E-5,
3.48542117235887));
#32001=CARTESIAN_POINT('Ctrl Pts',(-0.154111085743468,0.0233562467547802,
3.48422285425849));
#32002=CARTESIAN_POINT('Ctrl Pts',(-0.13822562008929,0.0978397409961887,
3.48039212464949));
#32003=CARTESIAN_POINT('Ctrl Pts',(-0.0229951370022999,0.180599416102118,
3.47392898353189));
#32004=CARTESIAN_POINT('Ctrl Pts',(0.138651671100891,0.117985766817156,
3.46603174900605));
#32005=CARTESIAN_POINT('Ctrl Pts',(0.174592817347261,-0.0515972368462645,
3.45813451448022));
#32006=CARTESIAN_POINT('Ctrl Pts',(0.0522430073621133,-0.174400672749591,
3.45023727995438));
#32007=CARTESIAN_POINT('Ctrl Pts',(-0.110463377019167,-0.140545639944236,
3.44266616591394));
#32008=CARTESIAN_POINT('Ctrl Pts',(-0.15411966834722,-0.0444868242763973,
3.4377274633821));
#32009=CARTESIAN_POINT('Ctrl Pts',(-0.154458280286029,0.000100830356962935,
3.43542117235887));
#32010=CARTESIAN_POINT('Ctrl Pts',(-0.154545466983052,1.64397697926493E-5,
3.48957882764113));
#32011=CARTESIAN_POINT('Ctrl Pts',(-0.154546843102601,0.000918015954509084,
3.48953212397352));
#32012=CARTESIAN_POINT('Ctrl Pts',(-0.154132992535152,0.0526348504359433,
3.4868530087973));
#32013=CARTESIAN_POINT('Ctrl Pts',(-0.0968288031440013,0.15417230277993,
3.48154148211247));
#32014=CARTESIAN_POINT('Ctrl Pts',(0.0761594573579975,0.165362221823523,
3.47364424758663));
#32015=CARTESIAN_POINT('Ctrl Pts',(0.180099349163956,0.0266298748857393,
3.46574701306079));
#32016=CARTESIAN_POINT('Ctrl Pts',(0.120755889508211,-0.136245876208876,
3.45784977853496));
#32017=CARTESIAN_POINT('Ctrl Pts',(-0.0480683862207756,-0.175597139874519,
3.44995254400912));
#32018=CARTESIAN_POINT('Ctrl Pts',(-0.144656135320296,-0.0831690899066176,
3.44386222704451));
#32019=CARTESIAN_POINT('Ctrl Pts',(-0.154307462490191,-0.0161560295849065,
3.44040432158851));
#32020=CARTESIAN_POINT('Ctrl Pts',(-0.154184766718538,-0.000123847547745311,
3.43957882764113));
#32021=CARTESIAN_POINT('Origin',(0.,0.,3.71042117235887));
#32022=CARTESIAN_POINT('',(-0.154141660315178,0.000107924336747972,3.53957882764113));
#32023=CARTESIAN_POINT('',(-0.154329957770701,-0.000135440264844456,3.53542117235887));
#32024=CARTESIAN_POINT('',(-0.1543,1.43283619370552E-14,3.71042117235887));
#32025=CARTESIAN_POINT('Ctrl Pts',(-0.154329957770701,-0.000135440264844458,
3.53542117235887));
#32026=CARTESIAN_POINT('Ctrl Pts',(-0.153965757190248,0.0399803656323286,
3.5333506566435));
#32027=CARTESIAN_POINT('Ctrl Pts',(-0.117549955642843,0.13168538088825,
3.52864772941951));
#32028=CARTESIAN_POINT('Ctrl Pts',(0.0365555273815534,0.178349539831362,
3.52131239068689));
#32029=CARTESIAN_POINT('Ctrl Pts',(0.169323388748115,0.0668919258489962,
3.51341515616108));
#32030=CARTESIAN_POINT('Ctrl Pts',(0.148577699872602,-0.105212180693424,
3.50551792163523));
#32031=CARTESIAN_POINT('Ctrl Pts',(-0.00687287246844015,-0.181927682017732,
3.4976206871094));
#32032=CARTESIAN_POINT('Ctrl Pts',(-0.133449900938225,-0.107089534990244,
3.49092177068394));
#32033=CARTESIAN_POINT('Ctrl Pts',(-0.154001816923033,-0.0278717244546827,
3.4868552657671));
#32034=CARTESIAN_POINT('Ctrl Pts',(-0.154061344734167,3.64105721256669E-5,
3.48542117235887));
#32035=CARTESIAN_POINT('Ctrl Pts',(-0.154141660315178,0.000107924336747963,
3.53957882764113));
#32036=CARTESIAN_POINT('Ctrl Pts',(-0.154258987201045,0.017967079764623,
3.53865992635852));
#32037=CARTESIAN_POINT('Ctrl Pts',(-0.14316956514131,0.0868471600938436,
3.53510861356731));
#32038=CARTESIAN_POINT('Ctrl Pts',(-0.0418557834629445,0.177179558878914,
3.52892488926748));
#32039=CARTESIAN_POINT('Ctrl Pts',(0.125477426630257,0.13191056683484,3.52102765474164));
#32040=CARTESIAN_POINT('Ctrl Pts',(0.179050327003836,-0.0329543119327003,
3.51313042021581));
#32041=CARTESIAN_POINT('Ctrl Pts',(0.0702903405429243,-0.167940855985405,
3.50523318568997));
#32042=CARTESIAN_POINT('Ctrl Pts',(-0.101176526834898,-0.15076997316947,
3.49738265483174));
#32043=CARTESIAN_POINT('Ctrl Pts',(-0.154469279323916,-0.0498985397050101,
3.49216453548213));
#32044=CARTESIAN_POINT('Ctrl Pts',(-0.154545466983052,1.64397697926493E-5,
3.48957882764113));
#32045=CARTESIAN_POINT('Origin',(0.,0.,3.71042117235887));
#32046=CARTESIAN_POINT('',(-0.154140927489633,-0.000180264065019253,3.58957882764113));
#32047=CARTESIAN_POINT('',(-0.15446591465964,9.2330361050462E-5,3.58542117235887));
#32048=CARTESIAN_POINT('',(-0.1543,1.43283619370552E-14,3.71042117235887));
#32049=CARTESIAN_POINT('',(-0.0398513841857247,-0.149064942821851,3.6));
#32050=CARTESIAN_POINT('Ctrl Pts',(-0.0398513841857247,-0.149064942821851,
3.6));
#32051=CARTESIAN_POINT('Ctrl Pts',(-0.0891618565331957,-0.135882161272422,
3.59736758849139));
#32052=CARTESIAN_POINT('Ctrl Pts',(-0.14437796139003,-0.0838321271698221,
3.59389386437176));
#32053=CARTESIAN_POINT('Ctrl Pts',(-0.154259564981832,-0.0165262407662603,
3.59042014025214));
#32054=CARTESIAN_POINT('Ctrl Pts',(-0.154140927489633,-0.000180264065019272,
3.58957882764113));
#32055=CARTESIAN_POINT('',(0.0399440158046003,-0.149318575284508,3.6));
#32056=CARTESIAN_POINT('Origin',(0.,0.,3.6));
#32057=CARTESIAN_POINT('Ctrl Pts',(0.0399441988940755,-0.14931907659749,
3.6));
#32058=CARTESIAN_POINT('Ctrl Pts',(-0.00742263582378978,-0.161856507480607,
3.59746250047314));
#32059=CARTESIAN_POINT('Ctrl Pts',(-0.110807703402812,-0.13923343552822,
3.59260289125943));
#32060=CARTESIAN_POINT('Ctrl Pts',(-0.154134073844742,-0.0447846479172299,
3.58774328204572));
#32061=CARTESIAN_POINT('Ctrl Pts',(-0.15446591465964,9.23303610504333E-5,
3.58542117235887));
#32062=CARTESIAN_POINT('Origin',(-1.70916393953233E-17,-6.81365885416763E-18,
2.7));
#32063=CARTESIAN_POINT('Ctrl Pts',(-0.0958116152722464,0.0825211298936403,
2.7));
#32064=CARTESIAN_POINT('Ctrl Pts',(-0.100666302508711,0.0779874972024075,
2.7));
#32065=CARTESIAN_POINT('Ctrl Pts',(-0.10511524090547,0.0730607151536329,
2.7));
#32066=CARTESIAN_POINT('Ctrl Pts',(-0.109154515912936,0.0678088625732328,
2.7));
#32067=CARTESIAN_POINT('Ctrl Pts',(-0.111628556611506,0.0645921226872924,
2.7));
#32068=CARTESIAN_POINT('Ctrl Pts',(-0.113949938179476,0.0612512837881844,
2.7));
#32069=CARTESIAN_POINT('Ctrl Pts',(-0.116112529388643,0.0578058814506189,
2.7));
#32070=CARTESIAN_POINT('Ctrl Pts',(-0.120278296492253,0.0511690544554421,
2.7));
#32071=CARTESIAN_POINT('Ctrl Pts',(-0.123843133570631,0.0441670378484578,
2.7));
#32072=CARTESIAN_POINT('Ctrl Pts',(-0.126794163478656,0.0368991818833284,
2.7));
#32073=CARTESIAN_POINT('Ctrl Pts',(-0.128540684647383,0.0325978143303114,
2.7));
#32074=CARTESIAN_POINT('Ctrl Pts',(-0.130072629552482,0.0281986906446855,
2.7));
#32075=CARTESIAN_POINT('Ctrl Pts',(-0.13137784724267,0.0237479033105473,
2.7));
#32076=CARTESIAN_POINT('Ctrl Pts',(-0.134168070532741,0.0142332525574809,
2.7));
#32077=CARTESIAN_POINT('Ctrl Pts',(-0.135935427906691,0.00446386180413974,
2.7));
#32078=CARTESIAN_POINT('Ctrl Pts',(-0.136643098733652,-0.00537896296213896,
2.7));
#32079=CARTESIAN_POINT('Ctrl Pts',(-0.136956933956429,-0.00974402223206864,
2.7));
#32080=CARTESIAN_POINT('Ctrl Pts',(-0.137061776691848,-0.0141238933117977,
2.7));
#32081=CARTESIAN_POINT('Ctrl Pts',(-0.136951314304003,-0.0185038366743994,
2.7));
#32082=CARTESIAN_POINT('Ctrl Pts',(-0.136873618225507,-0.0215845633357163,
2.7));
#32083=CARTESIAN_POINT('Ctrl Pts',(-0.13668911286562,-0.0246638039330577,
2.7));
#32084=CARTESIAN_POINT('Ctrl Pts',(-0.136397287648127,-0.0277243541204411,
2.7));
#32085=CARTESIAN_POINT('Ctrl Pts',(-0.136038403631432,-0.031488191097877,
2.7));
#32086=CARTESIAN_POINT('Ctrl Pts',(-0.135517191903042,-0.0352286565107813,
2.7));
#32087=CARTESIAN_POINT('Ctrl Pts',(-0.134831588718299,-0.0389361603135121,
2.7));
#32088=CARTESIAN_POINT('Ctrl Pts',(-0.133471069242182,-0.0462933769129071,
2.7));
#32089=CARTESIAN_POINT('Ctrl Pts',(-0.131464409754198,-0.0535208830833808,
2.7));
#32090=CARTESIAN_POINT('Ctrl Pts',(-0.128873836850864,-0.0605679807942907,
2.7));
#32091=CARTESIAN_POINT('Ctrl Pts',(-0.127324936193114,-0.064781432678084,
2.7));
#32092=CARTESIAN_POINT('Ctrl Pts',(-0.125566934259419,-0.0689304108686299,
2.7));
#32093=CARTESIAN_POINT('Ctrl Pts',(-0.123610254975486,-0.0730036509543968,
2.7));
#32094=CARTESIAN_POINT('Ctrl Pts',(-0.122225010943685,-0.0758873281953399,
2.7));
#32095=CARTESIAN_POINT('Ctrl Pts',(-0.120744058613202,-0.0787247786003408,
2.7));
#32096=CARTESIAN_POINT('Ctrl Pts',(-0.11917349881759,-0.0815104554030709,
2.7));
#32097=CARTESIAN_POINT('Ctrl Pts',(-0.115042560220701,-0.0888374351557691,
2.7));
#32098=CARTESIAN_POINT('Ctrl Pts',(-0.11029123440495,-0.095810889712998,
2.7));
#32099=CARTESIAN_POINT('Ctrl Pts',(-0.104997440961948,-0.102362839712403,
2.7));
#32100=CARTESIAN_POINT('Ctrl Pts',(-0.101348653506344,-0.106878821158406,
2.7));
#32101=CARTESIAN_POINT('Ctrl Pts',(-0.0974416313653614,-0.11119454456931,
2.7));
#32102=CARTESIAN_POINT('Ctrl Pts',(-0.09329635857045,-0.115285413781573,
2.7));
#32103=CARTESIAN_POINT('Ctrl Pts',(-0.0904535089763086,-0.118090953116413,
2.7));
#32104=CARTESIAN_POINT('Ctrl Pts',(-0.0874964288334564,-0.12079189694507,
2.7));
#32105=CARTESIAN_POINT('Ctrl Pts',(-0.0844493327259437,-0.123365242468763,
2.7));
#32106=CARTESIAN_POINT('Ctrl Pts',(-0.0762097423121146,-0.130323773594913,
2.7));
#32107=CARTESIAN_POINT('Ctrl Pts',(-0.0672905965515622,-0.136377649112853,
2.7));
#32108=CARTESIAN_POINT('Ctrl Pts',(-0.0578267373609757,-0.141381851878944,
2.7));
#32109=CARTESIAN_POINT('Ctrl Pts',(-0.0536817029967175,-0.143573620798307,
2.7));
#32110=CARTESIAN_POINT('Ctrl Pts',(-0.0494316342727489,-0.145563646977507,
2.7));
#32111=CARTESIAN_POINT('Ctrl Pts',(-0.0450857388735961,-0.147337358046063,
2.7));
#32112=CARTESIAN_POINT('Ctrl Pts',(-0.043386269574786,-0.148030970576765,
2.7));
#32113=CARTESIAN_POINT('Ctrl Pts',(-0.0416721350945774,-0.148691483593437,
2.7));
#32114=CARTESIAN_POINT('Ctrl Pts',(-0.0399441884684126,-0.149319082708151,
2.7));
#32115=CARTESIAN_POINT('Ctrl Pts',(0.0398513841857358,-0.149064942821848,
2.7));
#32116=CARTESIAN_POINT('Ctrl Pts',(0.0462200530662091,-0.146737857425647,
2.7));
#32117=CARTESIAN_POINT('Ctrl Pts',(0.0524055534681357,-0.143963403134301,
2.7));
#32118=CARTESIAN_POINT('Ctrl Pts',(0.0583783483111506,-0.140779078044469,
2.7));
#32119=CARTESIAN_POINT('Ctrl Pts',(0.062793202477668,-0.138425350642158,
2.7));
#32120=CARTESIAN_POINT('Ctrl Pts',(0.067091772966825,-0.135847508755531,
2.7));
#32121=CARTESIAN_POINT('Ctrl Pts',(0.0712602009478766,-0.133058650089746,
2.7));
#32122=CARTESIAN_POINT('Ctrl Pts',(0.0751200675142575,-0.130476232360243,
2.7));
#32123=CARTESIAN_POINT('Ctrl Pts',(0.078861342939135,-0.127717307612303,
2.7));
#32124=CARTESIAN_POINT('Ctrl Pts',(0.0824683178131891,-0.124797523957272,
2.7));
#32125=CARTESIAN_POINT('Ctrl Pts',(0.0880430571667216,-0.12028486905563,
2.7));
#32126=CARTESIAN_POINT('Ctrl Pts',(0.093301870580488,-0.115385246850429,
2.7));
#32127=CARTESIAN_POINT('Ctrl Pts',(0.098201122907525,-0.11013722292202,
2.7));
#32128=CARTESIAN_POINT('Ctrl Pts',(0.100467267721939,-0.107709754113023,
2.7));
#32129=CARTESIAN_POINT('Ctrl Pts',(0.102654039344122,-0.10520989028497,
2.7));
#32130=CARTESIAN_POINT('Ctrl Pts',(0.104752062819345,-0.102648267464436,
2.7));
#32131=CARTESIAN_POINT('Ctrl Pts',(0.111288676944248,-0.0946672605266598,
2.7));
#32132=CARTESIAN_POINT('Ctrl Pts',(0.11698432795861,-0.0860702972477514,
2.7));
#32133=CARTESIAN_POINT('Ctrl Pts',(0.121705201609602,-0.0769745632194894,
2.7));
#32134=CARTESIAN_POINT('Ctrl Pts',(0.12379312017453,-0.0729517586830322,
2.7));
#32135=CARTESIAN_POINT('Ctrl Pts',(0.125689731189231,-0.0688311600363216,
2.7));
#32136=CARTESIAN_POINT('Ctrl Pts',(0.127380076370131,-0.0646223264534606,
2.7));
#32137=CARTESIAN_POINT('Ctrl Pts',(0.128615050131834,-0.0615473337827676,
2.7));
#32138=CARTESIAN_POINT('Ctrl Pts',(0.129739752069541,-0.0584245102417657,
2.7));
#32139=CARTESIAN_POINT('Ctrl Pts',(0.130743760465559,-0.0552728510655911,
2.7));
#32140=CARTESIAN_POINT('Ctrl Pts',(0.131931576408969,-0.0515442059342363,
2.7));
#32141=CARTESIAN_POINT('Ctrl Pts',(0.132952645794869,-0.0477702728539015,
2.7));
#32142=CARTESIAN_POINT('Ctrl Pts',(0.13379905511372,-0.0439575955102323,
2.7));
#32143=CARTESIAN_POINT('Ctrl Pts',(0.135238114697535,-0.0374753064460584,
2.7));
#32144=CARTESIAN_POINT('Ctrl Pts',(0.136172820012768,-0.0308808878255892,
2.7));
#32145=CARTESIAN_POINT('Ctrl Pts',(0.136617245503396,-0.0242291498972301,
2.7));
#32146=CARTESIAN_POINT('Ctrl Pts',(0.136949796542121,-0.0192518423303904,
2.7));
#32147=CARTESIAN_POINT('Ctrl Pts',(0.13700760567975,-0.0142424066500717,
2.7));
#32148=CARTESIAN_POINT('Ctrl Pts',(0.136793131026844,-0.00922497436481165,
2.7));
#32149=CARTESIAN_POINT('Ctrl Pts',(0.136645101058571,-0.00576195282855203,
2.7));
#32150=CARTESIAN_POINT('Ctrl Pts',(0.1363675285007,-0.00230375513318918,
2.7));
#32151=CARTESIAN_POINT('Ctrl Pts',(0.13596351343207,0.00113554936727295,
2.7));
#32152=CARTESIAN_POINT('Ctrl Pts',(0.13510375104742,0.00845454528710606,
2.7));
#32153=CARTESIAN_POINT('Ctrl Pts',(0.133671961121794,0.0156977511556185,
2.7));
#32154=CARTESIAN_POINT('Ctrl Pts',(0.131684102868306,0.0227886248739312,
2.7));
#32155=CARTESIAN_POINT('Ctrl Pts',(0.130343128964387,0.0275720024591066,
2.7));
#32156=CARTESIAN_POINT('Ctrl Pts',(0.128748781223598,0.0322859803615266,
2.7));
#32157=CARTESIAN_POINT('Ctrl Pts',(0.126902487239724,0.0369045444632721,
2.7));
#32158=CARTESIAN_POINT('Ctrl Pts',(0.125403567336896,0.0406541410687207,
2.7));
#32159=CARTESIAN_POINT('Ctrl Pts',(0.123736334503949,0.0443441630809861,
2.7));
#32160=CARTESIAN_POINT('Ctrl Pts',(0.121913684068145,0.047935992310073,
2.7));
#32161=CARTESIAN_POINT('Ctrl Pts',(0.117743460752234,0.0561540958496606,
2.7));
#32162=CARTESIAN_POINT('Ctrl Pts',(0.112753744605352,0.0638862445298334,
2.7));
#32163=CARTESIAN_POINT('Ctrl Pts',(0.106960788703284,0.0709645017846505,
2.7));
#32164=CARTESIAN_POINT('Ctrl Pts',(0.104535029275377,0.0739284720891533,
2.7));
#32165=CARTESIAN_POINT('Ctrl Pts',(0.101968022916162,0.0767773427076814,
2.7));
#32166=CARTESIAN_POINT('Ctrl Pts',(0.0992594073891335,0.0794964656217155,
2.7));
#32167=CARTESIAN_POINT('Ctrl Pts',(0.0981919726164135,0.0805680412369242,
2.7));
#32168=CARTESIAN_POINT('Ctrl Pts',(0.0971025353237707,0.0816194476022307,
2.7));
#32169=CARTESIAN_POINT('Ctrl Pts',(0.0959918005672169,0.0826503307119895,
2.7));
#32170=CARTESIAN_POINT('Origin',(0.,0.,3.71042117235887));
#32171=CARTESIAN_POINT('Ctrl Pts',(-0.15446591465964,9.23303610504368E-5,
3.58542117235887));
#32172=CARTESIAN_POINT('Ctrl Pts',(-0.154510258305412,0.00608920819750747,
3.58511087053711));
#32173=CARTESIAN_POINT('Ctrl Pts',(-0.151481073290489,0.0629168758661166,
3.58216815720674));
#32174=CARTESIAN_POINT('Ctrl Pts',(-0.0810549264538156,0.163034932450524,
3.57659303236775));
#32175=CARTESIAN_POINT('Ctrl Pts',(0.0921890963056651,0.156981846810788,
3.56869579784192));
#32176=CARTESIAN_POINT('Ctrl Pts',(0.181852962765875,0.00863524897295638,
3.56079856331608));
#32177=CARTESIAN_POINT('Ctrl Pts',(0.10664300202618,-0.147556335146073,
3.55290132879024));
#32178=CARTESIAN_POINT('Ctrl Pts',(-0.0652523071804818,-0.169960705131912,
3.54500409426442));
#32179=CARTESIAN_POINT('Ctrl Pts',(-0.1484307843993,-0.072802923531341,
3.53917737545395));
#32180=CARTESIAN_POINT('Ctrl Pts',(-0.154428794390259,-0.0110220529132785,
3.53598306815211));
#32181=CARTESIAN_POINT('Ctrl Pts',(-0.154329957770701,-0.000135440264844458,
3.53542117235887));
#32182=CARTESIAN_POINT('Ctrl Pts',(-0.154140927489633,-0.000180264065019272,
3.58957882764113));
#32183=CARTESIAN_POINT('Ctrl Pts',(-0.153888356116389,0.0346192390763322,
3.58778772874353));
#32184=CARTESIAN_POINT('Ctrl Pts',(-0.125147291545086,0.121067307783401,
3.58336421833732));
#32185=CARTESIAN_POINT('Ctrl Pts',(0.0176337902165689,0.181151815132919,
3.5763082964225));
#32186=CARTESIAN_POINT('Ctrl Pts',(0.161334465098627,0.0843516096779105,
3.56841106189666));
#32187=CARTESIAN_POINT('Ctrl Pts',(0.158825384561566,-0.0890212772063117,
3.56051382737082));
#32188=CARTESIAN_POINT('Ctrl Pts',(0.0122890037691484,-0.181634540286447,
3.55261659284499));
#32189=CARTESIAN_POINT('Ctrl Pts',(-0.127027468209772,-0.117980653400407,
3.54563825960175));
#32190=CARTESIAN_POINT('Ctrl Pts',(-0.153922876401689,-0.0331947231106458,
3.54129233786714));
#32191=CARTESIAN_POINT('Ctrl Pts',(-0.154141660315178,0.000107924336747963,
3.53957882764113));
#32192=CARTESIAN_POINT('Ctrl Pts',(0.0958116152722374,0.0825211298936506,
3.6));
#32193=CARTESIAN_POINT('Ctrl Pts',(0.12310948837823,0.0508267830136165,
3.59736758849139));
#32194=CARTESIAN_POINT('Ctrl Pts',(0.143341746937054,-0.0412253317476725,
3.59210276547417));
#32195=CARTESIAN_POINT('Ctrl Pts',(0.0436608358730345,-0.142764465257081,
3.58420553094833));
#32196=CARTESIAN_POINT('Ctrl Pts',(-0.0955856094744946,-0.114504131671876,
3.57630829642249));
#32197=CARTESIAN_POINT('Ctrl Pts',(-0.148178789486409,0.0173870346414916,
3.56841106189666));
#32198=CARTESIAN_POINT('Ctrl Pts',(-0.066425116332372,0.133608342244775,
3.56051382737082));
#32199=CARTESIAN_POINT('Ctrl Pts',(0.0755496515090821,0.128647793449282,
3.55261659284499));
#32200=CARTESIAN_POINT('Ctrl Pts',(0.149029858339241,0.0070766508919659,
3.54471935831915));
#32201=CARTESIAN_POINT('Ctrl Pts',(0.0873947349721999,-0.120923516391581,
3.53682212379332));
#32202=CARTESIAN_POINT('Ctrl Pts',(-0.0534747520607383,-0.13928406457505,
3.52892488926748));
#32203=CARTESIAN_POINT('Ctrl Pts',(-0.145862599457632,-0.0313691495625942,
3.52102765474165));
#32204=CARTESIAN_POINT('Ctrl Pts',(-0.106007076394109,0.104987796417131,
3.5131304202158));
#32205=CARTESIAN_POINT('Ctrl Pts',(0.029957527138026,0.146158777133349,
3.50523318568998));
#32206=CARTESIAN_POINT('Ctrl Pts',(0.138761779048601,0.0548184317796861,
3.49733595116414));
#32207=CARTESIAN_POINT('Ctrl Pts',(0.121760532397217,-0.0862221662260755,
3.4894387166383));
#32208=CARTESIAN_POINT('Ctrl Pts',(-0.0056323702114988,-0.149091091323021,
3.48154148211246));
#32209=CARTESIAN_POINT('Ctrl Pts',(-0.127918803859021,-0.0767897408219312,
3.47364424758663));
#32210=CARTESIAN_POINT('Ctrl Pts',(-0.134230305961673,0.0651314716709306,
3.46574701306079));
#32211=CARTESIAN_POINT('Ctrl Pts',(-0.0188446861564537,0.148002567505592,
3.45784977853496));
#32212=CARTESIAN_POINT('Ctrl Pts',(0.113626077839972,0.0966902152561852,
3.44995254400912));
#32213=CARTESIAN_POINT('Ctrl Pts',(0.143080115058725,-0.0422843201504222,
3.44205530948329));
#32214=CARTESIAN_POINT('Ctrl Pts',(0.0428135339010967,-0.142922651128878,
3.43415807495745));
#32215=CARTESIAN_POINT('Ctrl Pts',(-0.0962690497602299,-0.113983126411312,
3.42626084043161));
#32216=CARTESIAN_POINT('Ctrl Pts',(-0.148071296290933,0.0182968362857149,
3.41836360590578));
#32217=CARTESIAN_POINT('Ctrl Pts',(-0.0656277734239754,0.133988351515145,
3.41046637137994));
#32218=CARTESIAN_POINT('Ctrl Pts',(0.076315808940436,0.128202107291143,
3.40256913685411));
#32219=CARTESIAN_POINT('Ctrl Pts',(0.149069246106613,0.0061840816248079,
3.39467190232827));
#32220=CARTESIAN_POINT('Ctrl Pts',(0.086672143362556,-0.121440613321149,
3.38677466780244));
#32221=CARTESIAN_POINT('Ctrl Pts',(-0.0543044603643882,-0.138963695209725,
3.37887743327661));
#32222=CARTESIAN_POINT('Ctrl Pts',(-0.14604705151224,-0.0304982252781714,
3.37098019875076));
#32223=CARTESIAN_POINT('Ctrl Pts',(-0.105379112789235,0.105617827984774,
3.36308296422493));
#32224=CARTESIAN_POINT('Ctrl Pts',(0.0308286127169663,0.145977668287988,
3.35518572969909));
#32225=CARTESIAN_POINT('Ctrl Pts',(0.139086215966064,0.0539898835791761,
3.34728849517326));
#32226=CARTESIAN_POINT('Ctrl Pts',(0.121244186506805,-0.0869467091899644,
3.33939126064743));
#32227=CARTESIAN_POINT('Ctrl Pts',(-0.00652136974010873,-0.149054871565549,
3.33149402612159));
#32228=CARTESIAN_POINT('Ctrl Pts',(-0.12837446138172,-0.0760255264081264,
3.32359679159575));
#32229=CARTESIAN_POINT('Ctrl Pts',(-0.133839510420159,0.0659307853068325,
3.31569955706992));
#32230=CARTESIAN_POINT('Ctrl Pts',(-0.0179617435035512,0.148112318093405,
3.30780232254408));
#32231=CARTESIAN_POINT('Ctrl Pts',(0.114200665588904,0.0960108899018034,
3.29990508801825));
#32232=CARTESIAN_POINT('Ctrl Pts',(0.142825410033637,-0.0431368201123976,
3.29200785349241));
#32233=CARTESIAN_POINT('Ctrl Pts',(0.0419604590288785,-0.143175426937629,
3.28411061896658));
#32234=CARTESIAN_POINT('Ctrl Pts',(-0.0969470717891682,-0.113407002747589,
3.27621338444074));
#32235=CARTESIAN_POINT('Ctrl Pts',(-0.147959550895179,0.0191795281376522,
3.26831614991491));
#32236=CARTESIAN_POINT('Ctrl Pts',(-0.0648275722345507,0.134377337668448,
3.26041891538907));
#32237=CARTESIAN_POINT('Ctrl Pts',(0.0770789801059626,0.127744721325426,
3.25252168086324));
#32238=CARTESIAN_POINT('Ctrl Pts',(0.149103473944927,0.00529500313887513,
3.24462444633739));
#32239=CARTESIAN_POINT('Ctrl Pts',(0.085946395912033,-0.121955319811881,
3.23672721181157));
#32240=CARTESIAN_POINT('Ctrl Pts',(-0.0551321992305218,-0.138637381714645,
3.22882997728572));
#32241=CARTESIAN_POINT('Ctrl Pts',(-0.146226329520922,-0.0296267371731131,
3.22093274275989));
#32242=CARTESIAN_POINT('Ctrl Pts',(-0.104747391252292,0.106244374093527,
3.21303550823405));
#32243=CARTESIAN_POINT('Ctrl Pts',(0.0316985965714106,0.145791227363271,
3.20513827370822));
#32244=CARTESIAN_POINT('Ctrl Pts',(0.139405709322103,0.0531594884201076,
3.19724103918239));
#32245=CARTESIAN_POINT('Ctrl Pts',(0.12072352734024,-0.0876681980379225,
3.18934380465655));
#32246=CARTESIAN_POINT('Ctrl Pts',(-0.00741013659566878,-0.149013331203351,
3.18144657013072));
#32247=CARTESIAN_POINT('Ctrl Pts',(-0.128825553891948,-0.0752586185437851,
3.17354933560487));
#32248=CARTESIAN_POINT('Ctrl Pts',(-0.133443954917441,0.0667277595658497,
3.16565210107904));
#32249=CARTESIAN_POINT('Ctrl Pts',(-0.0170781621796165,0.148216798566333,
3.15775486655321));
#32250=CARTESIAN_POINT('Ctrl Pts',(0.114771192054407,0.0953281515350871,
3.14985763202737));
#32251=CARTESIAN_POINT('Ctrl Pts',(0.14256562565491,-0.0439877867403021,
3.14196039750153));
#32252=CARTESIAN_POINT('Ctrl Pts',(0.0411058919243144,-0.143423110584706,
3.1340631629757));
#32253=CARTESIAN_POINT('Ctrl Pts',(-0.0976216460800827,-0.112826846172802,
3.12616592844987));
#32254=CARTESIAN_POINT('Ctrl Pts',(-0.147842543583951,0.0200615380096788,
3.11826869392402));
#32255=CARTESIAN_POINT('Ctrl Pts',(-0.0640250655728793,0.134761544882338,
3.11037145939819));
#32256=CARTESIAN_POINT('Ctrl Pts',(0.0778394100992752,0.127282792380129,
3.10247422487235));
#32257=CARTESIAN_POINT('Ctrl Pts',(0.14913239918967,0.00440573633107837,
3.09457699034652));
#32258=CARTESIAN_POINT('Ctrl Pts',(0.0852175919350427,-0.122465689176514,
3.08667975582068));
#32259=CARTESIAN_POINT('Ctrl Pts',(-0.0559579774207319,-0.138306137838011,
3.07878252129485));
#32260=CARTESIAN_POINT('Ctrl Pts',(-0.14640040725691,-0.028754195445133,
3.07088528676901));
#32261=CARTESIAN_POINT('Ctrl Pts',(-0.104111944565534,0.106867141813886,
3.06298805224318));
#32262=CARTESIAN_POINT('Ctrl Pts',(0.0325674531231242,0.145599601640112,
3.05509081771734));
#32263=CARTESIAN_POINT('Ctrl Pts',(0.139720244968427,0.0523272027405333,
3.04719358319151));
#32264=CARTESIAN_POINT('Ctrl Pts',(0.120198574861694,-0.0883865691262194,
3.03929634866567));
#32265=CARTESIAN_POINT('Ctrl Pts',(-0.00829863992324496,-0.148966491453986,
3.03139911413983));
#32266=CARTESIAN_POINT('Ctrl Pts',(-0.129272064956395,-0.0744890342439453,
3.023501879614));
#32267=CARTESIAN_POINT('Ctrl Pts',(-0.133043653723939,0.0675223607738245,
3.01560464508816));
#32268=CARTESIAN_POINT('Ctrl Pts',(-0.0161939735020032,0.148316007979255,
3.00770741056233));
#32269=CARTESIAN_POINT('Ctrl Pts',(0.115337636891868,0.0946420229965858,
2.9998101760365));
#32270=CARTESIAN_POINT('Ctrl Pts',(0.142300771189819,-0.0448371890228274,
2.99191294151066));
#32271=CARTESIAN_POINT('Ctrl Pts',(0.040249862963706,-0.14366569365053,
2.98401570698482));
#32272=CARTESIAN_POINT('Ctrl Pts',(-0.0982927486352741,-0.112242677117094,
2.97611847245899));
#32273=CARTESIAN_POINT('Ctrl Pts',(-0.14772027852239,0.0209428344297273,
2.96822123793315));
#32274=CARTESIAN_POINT('Ctrl Pts',(-0.0632202819765869,0.135140959547726,
2.96032400340732));
#32275=CARTESIAN_POINT('Ctrl Pts',(0.0785970718760291,0.126816336854618,
2.95242676888148));
#32276=CARTESIAN_POINT('Ctrl Pts',(0.149156020812652,0.00351631284117927,
2.94452953435565));
#32277=CARTESIAN_POINT('Ctrl Pts',(0.0844857573500313,-0.122971703272108,
2.93663229982981));
#32278=CARTESIAN_POINT('Ctrl Pts',(-0.0567817655678681,-0.137969975356402,
2.92873506530398));
#32279=CARTESIAN_POINT('Ctrl Pts',(-0.146569278528953,-0.0278806311257436,
2.92083783077813));
#32280=CARTESIAN_POINT('Ctrl Pts',(-0.103472795328523,0.107486108997575,
2.91294059625231));
#32281=CARTESIAN_POINT('Ctrl Pts',(0.0334351514749053,0.145402797936144,
2.90504336172646));
#32282=CARTESIAN_POINT('Ctrl Pts',(0.140029811715087,0.0514930561329736,
2.89714612720063));
#32283=CARTESIAN_POINT('Ctrl Pts',(0.119669347747977,-0.0891017968949556,
2.88924889267479));
#32284=CARTESIAN_POINT('Ctrl Pts',(-0.00918684813991898,-0.148914354007184,
2.88135165814896));
#32285=CARTESIAN_POINT('Ctrl Pts',(-0.129713978666681,-0.073716800831252,
2.87345442362312));
#32286=CARTESIAN_POINT('Ctrl Pts',(-0.132638621131497,0.0683145605832212,
2.86555718909729));
#32287=CARTESIAN_POINT('Ctrl Pts',(-0.0153092088077737,0.148409942975243,
2.85765995457145));
#32288=CARTESIAN_POINT('Ctrl Pts',(0.11589997974986,0.0939525283576191,
2.84976272004561));
#32289=CARTESIAN_POINT('Ctrl Pts',(0.14203085645546,-0.0456849961183085,
2.84186548551979));
#32290=CARTESIAN_POINT('Ctrl Pts',(0.0393924018242494,-0.143903168728488,
2.83396825099394));
#32291=CARTESIAN_POINT('Ctrl Pts',(-0.0989603541143928,-0.111654514006987,
2.82607101646811));
#32292=CARTESIAN_POINT('Ctrl Pts',(-0.14759276289462,0.0218233815372009,
2.81817378194227));
#32293=CARTESIAN_POINT('Ctrl Pts',(-0.0624132446091692,0.135515576866934,
2.81027654741644));
#32294=CARTESIAN_POINT('Ctrl Pts',(0.0793519279903814,0.126345354605138,
2.8023793128906));
#32295=CARTESIAN_POINT('Ctrl Pts',(0.149174358180394,0.00262679649731067,
2.79448207836477));
#32296=CARTESIAN_POINT('Ctrl Pts',(0.0837508793007237,-0.12347340605925,
2.78658484383893));
#32297=CARTESIAN_POINT('Ctrl Pts',(-0.0576034595552612,-0.137628787005506,
2.7786876093131));
#32298=CARTESIAN_POINT('Ctrl Pts',(-0.146733081304572,-0.0270063046901533,
2.77079037478726));
#32299=CARTESIAN_POINT('Ctrl Pts',(-0.102829689230287,0.108101695072837,
2.76289314026143));
#32300=CARTESIAN_POINT('Ctrl Pts',(0.0343011276704797,0.145199973805224,
2.75499590573559));
#32301=CARTESIAN_POINT('Ctrl Pts',(0.140335424370929,0.0506587128142576,
2.74709867120975));
#32302=CARTESIAN_POINT('Ctrl Pts',(0.11913389087728,-0.0898170012241629,
2.73920143668392));
#32303=CARTESIAN_POINT('Ctrl Pts',(-0.0100709312277202,-0.14885086814231,
2.73130420215808));
#32304=CARTESIAN_POINT('Ctrl Pts',(-0.130158589013459,-0.0729535941759648,
2.72340696763225));
#32305=CARTESIAN_POINT('Ctrl Pts',(-0.132214800612389,0.0691267612890124,
2.71550973310641));
#32306=CARTESIAN_POINT('Ctrl Pts',(-0.0144510241825876,0.148455288920992,
2.70761249858058));
#32307=CARTESIAN_POINT('Ctrl Pts',(0.116510849855331,0.0933444320528056,
2.69971526405474));
#32308=CARTESIAN_POINT('Ctrl Pts',(0.141650318794474,-0.0467072968399595,
2.6918180295289));
#32309=CARTESIAN_POINT('Ctrl Pts',(0.073068805953493,-0.111356443894342,
2.68655320651168));
#32310=CARTESIAN_POINT('Ctrl Pts',(0.0326585063531192,-0.122159831625552,
2.68392079500307));
#32311=CARTESIAN_POINT('Ctrl Pts',(0.102845629995664,0.088579422941069,
3.60535973499898));
#32312=CARTESIAN_POINT('Ctrl Pts',(0.132147577876935,0.0545582339347427,
3.60272732349037));
#32313=CARTESIAN_POINT('Ctrl Pts',(0.153865188751202,-0.0442518916242316,
3.59746250047314));
#32314=CARTESIAN_POINT('Ctrl Pts',(0.046866198411756,-0.153245525906639,
3.58956526594731));
#32315=CARTESIAN_POINT('Ctrl Pts',(-0.102603031970513,-0.122910458459966,
3.58166803142147));
#32316=CARTESIAN_POINT('Ctrl Pts',(-0.159057343031147,0.0186635046949134,
3.57377079689563));
#32317=CARTESIAN_POINT('Ctrl Pts',(-0.0713017197061865,0.143417205646691,
3.5658735623698));
#32318=CARTESIAN_POINT('Ctrl Pts',(0.0810961331079431,0.138092477903117,
3.55797632784396));
#32319=CARTESIAN_POINT('Ctrl Pts',(0.159970893148119,0.00759618358562943,
3.55007909331813));
#32320=CARTESIAN_POINT('Ctrl Pts',(0.0938108239901933,-0.129801122643079,
3.54218185879229));
#32321=CARTESIAN_POINT('Ctrl Pts',(-0.0574006037673195,-0.149509611427338,
3.53428462426646));
#32322=CARTESIAN_POINT('Ctrl Pts',(-0.156571109790821,-0.0336721173108959,
3.52638738974062));
#32323=CARTESIAN_POINT('Ctrl Pts',(-0.113789591426601,0.112695480957047,
3.51849015521479));
#32324=CARTESIAN_POINT('Ctrl Pts',(0.0321568605525351,0.15688903136602,
3.51059292068895));
#32325=CARTESIAN_POINT('Ctrl Pts',(0.148948982281772,0.0588429298027895,
3.50269568616312));
#32326=CARTESIAN_POINT('Ctrl Pts',(0.130699588222345,-0.092552171048525,
3.49479845163728));
#32327=CARTESIAN_POINT('Ctrl Pts',(-0.00604587096381251,-0.160036621554591,
3.48690121711144));
#32328=CARTESIAN_POINT('Ctrl Pts',(-0.137309969504135,-0.0824272636422575,
3.47900398258561));
#32329=CARTESIAN_POINT('Ctrl Pts',(-0.144084830862247,0.0699131020545748,
3.47110674805977));
#32330=CARTESIAN_POINT('Ctrl Pts',(-0.0202281697717358,0.158868183704434,
3.46320951353394));
#32331=CARTESIAN_POINT('Ctrl Pts',(0.121967942260279,0.103788732443176,
3.4553122790081));
#32332=CARTESIAN_POINT('Ctrl Pts',(0.153584349154903,-0.045388625715703,
3.44741504448227));
#32333=CARTESIAN_POINT('Ctrl Pts',(0.0459566917214356,-0.153415325002449,
3.43951780995643));
#32334=CARTESIAN_POINT('Ctrl Pts',(-0.103336647060408,-0.122351203571073,
3.43162057543059));
#32335=CARTESIAN_POINT('Ctrl Pts',(-0.158941958217129,0.0196400994742142,
3.42372334090476));
#32336=CARTESIAN_POINT('Ctrl Pts',(-0.0704458398266582,0.14382511331743,
3.41582610637892));
#32337=CARTESIAN_POINT('Ctrl Pts',(0.0819185380270082,0.137614071672475,
3.40792887185309));
#32338=CARTESIAN_POINT('Ctrl Pts',(0.160013172570483,0.00663808629925336,
3.40003163732726));
#32339=CARTESIAN_POINT('Ctrl Pts',(0.0930351832799072,-0.130356182270652,
3.39213440280141));
#32340=CARTESIAN_POINT('Ctrl Pts',(-0.0582912251492787,-0.149165722128378,
3.38423716827558));
#32341=CARTESIAN_POINT('Ctrl Pts',(-0.15676910340262,-0.0327372540747895,
3.37633993374974));
#32342=CARTESIAN_POINT('Ctrl Pts',(-0.113115525840982,0.11337176632503,
3.36844269922391));
#32343=CARTESIAN_POINT('Ctrl Pts',(0.0330918969246043,0.156694626405347,
3.36054546469807));
#32344=CARTESIAN_POINT('Ctrl Pts',(0.149297237752422,0.0579535536930025,
3.35264823017224));
#32345=CARTESIAN_POINT('Ctrl Pts',(0.130145334771507,-0.0933299063718294,
3.3447509956464));
#32346=CARTESIAN_POINT('Ctrl Pts',(-0.00700013643909911,-0.159997742721738,
3.33685376112057));
#32347=CARTESIAN_POINT('Ctrl Pts',(-0.137799079147585,-0.0816069443874761,
3.32895652659473));
#32348=CARTESIAN_POINT('Ctrl Pts',(-0.143665345045706,0.0707710973426707,
3.3210592920689));
#32349=CARTESIAN_POINT('Ctrl Pts',(-0.019280405838002,0.158985991637365,
3.31316205754306));
#32350=CARTESIAN_POINT('Ctrl Pts',(0.122584713398713,0.103059534382534,
3.30526482301722));
#32351=CARTESIAN_POINT('Ctrl Pts',(0.153310944947138,-0.0463037120067701,
3.29736758849139));
#32352=CARTESIAN_POINT('Ctrl Pts',(0.04504098831306,-0.15368665836036,3.28947035396555));
#32353=CARTESIAN_POINT('Ctrl Pts',(-0.1040644461119,-0.121732783758583,
3.28157311943972));
#32354=CARTESIAN_POINT('Ctrl Pts',(-0.158822009027328,0.0205875941944168,
3.27367588491388));
#32355=CARTESIAN_POINT('Ctrl Pts',(-0.0695868918252512,0.14424265690943,
3.26577865038805));
#32356=CARTESIAN_POINT('Ctrl Pts',(0.0827377374433846,0.137123106692272,
3.25788141586221));
#32357=CARTESIAN_POINT('Ctrl Pts',(0.160049913247329,0.00568373606998795,
3.24998418133638));
#32358=CARTESIAN_POINT('Ctrl Pts',(0.0922561550425197,-0.130908675965198,
3.24208694681054));
#32359=CARTESIAN_POINT('Ctrl Pts',(-0.0591797325073638,-0.148815452311067,
3.2341897122847));
#32360=CARTESIAN_POINT('Ctrl Pts',(-0.156961543115644,-0.0318017856251262,
3.22629247775887));
#32361=CARTESIAN_POINT('Ctrl Pts',(-0.112437426434515,0.114044310348977,
3.21839524323303));
#32362=CARTESIAN_POINT('Ctrl Pts',(0.0340257506890165,0.156494497910436,
3.21049800870719));
#32363=CARTESIAN_POINT('Ctrl Pts',(0.149640186729828,0.0570621950300983,
3.20260077418136));
#32364=CARTESIAN_POINT('Ctrl Pts',(0.129586451385121,-0.094104363361123,
3.19470353965552));
#32365=CARTESIAN_POINT('Ctrl Pts',(-0.00795415215963184,-0.159953152671687,
3.18680630512969));
#32366=CARTESIAN_POINT('Ctrl Pts',(-0.138283288637936,-0.0807837339423469,
3.17890907060385));
#32367=CARTESIAN_POINT('Ctrl Pts',(-0.143240749815163,0.0716265815084065,
3.17101183607802));
#32368=CARTESIAN_POINT('Ctrl Pts',(-0.0183319563451689,0.159098142549652,
3.16311460155218));
#32369=CARTESIAN_POINT('Ctrl Pts',(0.123197125094384,0.10232667274308,3.15521736702635));
#32370=CARTESIAN_POINT('Ctrl Pts',(0.153032088484722,-0.047217152393966,
3.14732013250051));
#32371=CARTESIAN_POINT('Ctrl Pts',(0.0441236831200233,-0.153952525715282,
3.13942289797468));
#32372=CARTESIAN_POINT('Ctrl Pts',(-0.104788544309502,-0.121110034958652,
3.13152566344884));
#32373=CARTESIAN_POINT('Ctrl Pts',(-0.158696411618254,0.021534356867118,
3.123628428923));
#32374=CARTESIAN_POINT('Ctrl Pts',(-0.0687254690952325,0.14465507071593,
3.11573119439717));
#32375=CARTESIAN_POINT('Ctrl Pts',(0.0835539944442463,0.136627265209407,
3.10783395987133));
#32376=CARTESIAN_POINT('Ctrl Pts',(0.160080962040421,0.00472918369319909,
3.0999367253455));
#32377=CARTESIAN_POINT('Ctrl Pts',(0.091473845883615,-0.131456514123307,
3.09203949081966));
#32378=CARTESIAN_POINT('Ctrl Pts',(-0.0600661352464005,-0.148459890147985,
3.08414225629383));
#32379=CARTESIAN_POINT('Ctrl Pts',(-0.157148400777682,-0.0308651862007597,
3.07624502176799));
#32380=CARTESIAN_POINT('Ctrl Pts',(-0.111755328396166,0.114712798593949,
3.06834778724216));
#32381=CARTESIAN_POINT('Ctrl Pts',(0.0349583943897092,0.156288803974834,
3.06045055271632));
#32382=CARTESIAN_POINT('Ctrl Pts',(0.149977814027003,0.0561688070540271,
3.05255331819049));
#32383=CARTESIAN_POINT('Ctrl Pts',(0.129022959493032,-0.0948754737002677,
3.04465608366465));
#32384=CARTESIAN_POINT('Ctrl Pts',(-0.00890788500525998,-0.159902874179684,
3.03675884913881));
#32385=CARTESIAN_POINT('Ctrl Pts',(-0.138762580335427,-0.0799576505710677,
3.02886161461298));
#32386=CARTESIAN_POINT('Ctrl Pts',(-0.142811060488699,0.072479518405434,
3.02096438008714));
#32387=CARTESIAN_POINT('Ctrl Pts',(-0.0173828549097553,0.159204635426789,
3.01306714556131));
#32388=CARTESIAN_POINT('Ctrl Pts',(0.123805155509077,0.101590172042203,
3.00516991103547));
#32389=CARTESIAN_POINT('Ctrl Pts',(0.152747789715287,-0.0481289135892851,
2.99727267650964));
#32390=CARTESIAN_POINT('Ctrl Pts',(0.0432048087487045,-0.154212918029513,
2.9893754419838));
#32391=CARTESIAN_POINT('Ctrl Pts',(-0.105508915893722,-0.120482979101306,
2.98147820745797));
#32392=CARTESIAN_POINT('Ctrl Pts',(-0.158565170460834,0.0224803537097271,
2.97358097293213));
#32393=CARTESIAN_POINT('Ctrl Pts',(-0.067861602269319,0.145062340128731,
2.9656837384063));
#32394=CARTESIAN_POINT('Ctrl Pts',(0.0843672799997867,0.136126564827205,
2.95778650388046));
#32395=CARTESIAN_POINT('Ctrl Pts',(0.160106317846084,0.0037744631314833,
2.94988926935462));
#32396=CARTESIAN_POINT('Ctrl Pts',(0.0906882836244439,-0.131999677270073,
2.94199203482879));
#32397=CARTESIAN_POINT('Ctrl Pts',(-0.0609504018432475,-0.148099048280287,
2.93409480030295));
#32398=CARTESIAN_POINT('Ctrl Pts',(-0.157329669742954,-0.0299274891113821,
2.92619756577712));
#32399=CARTESIAN_POINT('Ctrl Pts',(-0.111069255984644,0.115377207285653,
2.91830033125128));
#32400=CARTESIAN_POINT('Ctrl Pts',(0.0358897948611611,0.156077551916693,
2.91040309672545));
#32401=CARTESIAN_POINT('Ctrl Pts',(0.150310107632486,0.0552734215298454,
2.90250586219961));
#32402=CARTESIAN_POINT('Ctrl Pts',(0.128454879143209,-0.0956432099528824,
2.89460862767377));
#32403=CARTESIAN_POINT('Ctrl Pts',(-0.00986130107440376,-0.159846909059511,
2.88671139314794));
#32404=CARTESIAN_POINT('Ctrl Pts',(-0.139236937163761,-0.079128723602177,
2.8788141586221));
#32405=CARTESIAN_POINT('Ctrl Pts',(-0.142376292407395,0.0733298776050816,
2.87091692409627));
#32406=CARTESIAN_POINT('Ctrl Pts',(-0.0164331351694357,0.159305466665398,
2.86301968957043));
#32407=CARTESIAN_POINT('Ctrl Pts',(0.124408782797267,0.10085005811842,2.85512245504459));
#32408=CARTESIAN_POINT('Ctrl Pts',(0.152458059176653,-0.0490389624868201,
2.84722522051876));
#32409=CARTESIAN_POINT('Ctrl Pts',(0.0422843970550532,-0.154467827352683,
2.83932798599292));
#32410=CARTESIAN_POINT('Ctrl Pts',(-0.106225533663848,-0.11985163596585,
2.83143075146709));
#32411=CARTESIAN_POINT('Ctrl Pts',(-0.158428293266612,0.0234255462289395,
2.82353351694125));
#32412=CARTESIAN_POINT('Ctrl Pts',(-0.0669953162115558,0.145464459997932,
2.81563628241542));
#32413=CARTESIAN_POINT('Ctrl Pts',(0.085177553915074,0.13562100539136,2.80773904788958));
#32414=CARTESIAN_POINT('Ctrl Pts',(0.160126001452633,0.00281964289891892,
2.79984181336375));
#32415=CARTESIAN_POINT('Ctrl Pts',(0.0898994544648863,-0.132538212593453,
2.79194457883791));
#32416=CARTESIAN_POINT('Ctrl Pts',(-0.0618324205375044,-0.147732811568847,
2.78404734431207));
#32417=CARTESIAN_POINT('Ctrl Pts',(-0.157505498107873,-0.028988973955003,
2.77615010978624));
#32418=CARTESIAN_POINT('Ctrl Pts',(-0.110378936218723,0.11603798664468,
2.7682528752604));
#32419=CARTESIAN_POINT('Ctrl Pts',(0.0368193467442185,0.155859837441643,
2.76035564073457));
#32420=CARTESIAN_POINT('Ctrl Pts',(0.150638156857367,0.0543778248529476,
2.75245840620873));
#32421=CARTESIAN_POINT('Ctrl Pts',(0.127880111678472,-0.0964109210451539,
2.7445611716829));
#32422=CARTESIAN_POINT('Ctrl Pts',(-0.0108102891681236,-0.159778762376561,
2.73666393715706));
#32423=CARTESIAN_POINT('Ctrl Pts',(-0.139714188602295,-0.0783094860905571,
2.72876670263123));
#32424=CARTESIAN_POINT('Ctrl Pts',(-0.141921357082812,0.0742017060679738,
2.72086946810539));
#32425=CARTESIAN_POINT('Ctrl Pts',(-0.0155119468753121,0.159354141686116,
2.71297223357956));
#32426=CARTESIAN_POINT('Ctrl Pts',(0.125064499963334,0.100197318391729,
2.70507499905372));
#32427=CARTESIAN_POINT('Ctrl Pts',(0.152049584323474,-0.050136315469175,
2.69717776452788));
#32428=CARTESIAN_POINT('Ctrl Pts',(0.0784331561467309,-0.119531683020366,
2.69191294151066));
#32429=CARTESIAN_POINT('Ctrl Pts',(0.0350561322973247,-0.131128202024318,
2.68928053000205));
#32430=CARTESIAN_POINT('Ctrl Pts',(0.10987964471909,0.0946377159884874,
3.61071946999795));
#32431=CARTESIAN_POINT('Ctrl Pts',(0.14118566737564,0.0582896848558689,
3.60808705848934));
#32432=CARTESIAN_POINT('Ctrl Pts',(0.16438863056535,-0.0472784515007908,
3.60282223547212));
#32433=CARTESIAN_POINT('Ctrl Pts',(0.0500715609504776,-0.163726586556196,
3.59492500094628));
#32434=CARTESIAN_POINT('Ctrl Pts',(-0.109620454466532,-0.131316785248055,
3.58702776642045));
#32435=CARTESIAN_POINT('Ctrl Pts',(-0.169935896575886,0.0199399747483351,
3.57913053189461));
#32436=CARTESIAN_POINT('Ctrl Pts',(-0.0761783230800011,0.153226069048607,
3.57123329736878));
#32437=CARTESIAN_POINT('Ctrl Pts',(0.0866426147068042,0.147537162356952,
3.56333606284294));
#32438=CARTESIAN_POINT('Ctrl Pts',(0.170911927956997,0.00811571627929297,
3.55543882831711));
#32439=CARTESIAN_POINT('Ctrl Pts',(0.100226913008187,-0.138678728894576,
3.54754159379127));
#32440=CARTESIAN_POINT('Ctrl Pts',(-0.0613264554739007,-0.159735158279625,
3.53964435926544));
#32441=CARTESIAN_POINT('Ctrl Pts',(-0.167279620124009,-0.0359750850591977,
3.53174712473959));
#32442=CARTESIAN_POINT('Ctrl Pts',(-0.121572106459094,0.120403165496963,
3.52384989021377));
#32443=CARTESIAN_POINT('Ctrl Pts',(0.0343561939670442,0.167619285598691,
3.51595265568792));
#32444=CARTESIAN_POINT('Ctrl Pts',(0.159136185514944,0.0628674278258929,
3.5080554211621));
#32445=CARTESIAN_POINT('Ctrl Pts',(0.139638644047474,-0.0988821758709744,
3.50015818663625));
#32446=CARTESIAN_POINT('Ctrl Pts',(-0.00645937171612636,-0.170982151786161,
3.49226095211042));
#32447=CARTESIAN_POINT('Ctrl Pts',(-0.146701135149248,-0.0880647864625838,
3.48436371758458));
#32448=CARTESIAN_POINT('Ctrl Pts',(-0.15393935576282,0.074694732438219,
3.47646648305875));
#32449=CARTESIAN_POINT('Ctrl Pts',(-0.0216116533870178,0.169733799903276,
3.46856924853291));
#32450=CARTESIAN_POINT('Ctrl Pts',(0.130309806680585,0.110887249630166,
3.46067201400708));
#32451=CARTESIAN_POINT('Ctrl Pts',(0.164088583251082,-0.0484929312809838,
3.45277477948124));
#32452=CARTESIAN_POINT('Ctrl Pts',(0.0490998495417746,-0.16390799887602,
3.4448775449554));
#32453=CARTESIAN_POINT('Ctrl Pts',(-0.110404244360585,-0.130719280730833,
3.43698031042957));
#32454=CARTESIAN_POINT('Ctrl Pts',(-0.169812620143325,0.0209833626627134,
3.42908307590373));
#32455=CARTESIAN_POINT('Ctrl Pts',(-0.075263906229341,0.153661875119715,
3.4211858413779));
#32456=CARTESIAN_POINT('Ctrl Pts',(0.0875212671135803,0.147026036053807,
3.41328860685206));
#32457=CARTESIAN_POINT('Ctrl Pts',(0.170957099034354,0.00709209097369881,
3.40539137232623));
#32458=CARTESIAN_POINT('Ctrl Pts',(0.0993982231972585,-0.139271751220155,
3.39749413780039));
#32459=CARTESIAN_POINT('Ctrl Pts',(-0.0622779899341693,-0.15936774904703,
3.38959690327456));
#32460=CARTESIAN_POINT('Ctrl Pts',(-0.167491155293001,-0.0349762828714076,
3.38169966874872));
#32461=CARTESIAN_POINT('Ctrl Pts',(-0.120851938892729,0.121125704665286,
3.37380243422289));
#32462=CARTESIAN_POINT('Ctrl Pts',(0.0353551811322426,0.167411584522707,
3.36590519969705));
#32463=CARTESIAN_POINT('Ctrl Pts',(0.15950825953878,0.0619172238068289,
3.35800796517121));
#32464=CARTESIAN_POINT('Ctrl Pts',(0.139046483036208,-0.0997131035536944,
3.35011073064538));
#32465=CARTESIAN_POINT('Ctrl Pts',(-0.00747890313808957,-0.170940613877928,
3.34221349611955));
#32466=CARTESIAN_POINT('Ctrl Pts',(-0.14722369691345,-0.0871883623668259,
3.33431626159371));
#32467=CARTESIAN_POINT('Ctrl Pts',(-0.153491179671254,0.0756114093785092,
3.32641902706787));
#32468=CARTESIAN_POINT('Ctrl Pts',(-0.0205990681724529,0.169859665181325,
3.31852179254204));
#32469=CARTESIAN_POINT('Ctrl Pts',(0.130968761208522,0.110108178863265,
3.3106245580162));
#32470=CARTESIAN_POINT('Ctrl Pts',(0.16379647986064,-0.0494706039011429,
3.30272732349037));
#32471=CARTESIAN_POINT('Ctrl Pts',(0.0481215175972415,-0.16419788978309,
3.29483008896453));
#32472=CARTESIAN_POINT('Ctrl Pts',(-0.111181820434632,-0.130058564769576,
3.2869328544387));
#32473=CARTESIAN_POINT('Ctrl Pts',(-0.169684467159477,0.0219956602511813,
3.27903561991286));
#32474=CARTESIAN_POINT('Ctrl Pts',(-0.0743462114159517,0.154107976150411,
3.27113838538702));
#32475=CARTESIAN_POINT('Ctrl Pts',(0.0883964947808067,0.146501492059118,
3.26324115086119));
#32476=CARTESIAN_POINT('Ctrl Pts',(0.170996352549731,0.00607246900110077,
3.25534391633535));
#32477=CARTESIAN_POINT('Ctrl Pts',(0.0985659141730064,-0.139862032118515,
3.24744668180952));
#32478=CARTESIAN_POINT('Ctrl Pts',(-0.0632272657842059,-0.15899352290749,
3.23954944728368));
#32479=CARTESIAN_POINT('Ctrl Pts',(-0.167696756710366,-0.0339768340771394,
3.23165221275785));
#32480=CARTESIAN_POINT('Ctrl Pts',(-0.120127461616738,0.121844246604426,
3.22375497823201));
#32481=CARTESIAN_POINT('Ctrl Pts',(0.0363529048066224,0.167197768457601,
3.21585774370617));
#32482=CARTESIAN_POINT('Ctrl Pts',(0.159874664137553,0.0609649016400891,
3.20796050918034));
#32483=CARTESIAN_POINT('Ctrl Pts',(0.138449375430002,-0.100540528684324,
3.2000632746545));
#32484=CARTESIAN_POINT('Ctrl Pts',(-0.00849816772359493,-0.170892974140023,
3.19216604012867));
#32485=CARTESIAN_POINT('Ctrl Pts',(-0.147741023383925,-0.0863088493409087,
3.18426880560283));
#32486=CARTESIAN_POINT('Ctrl Pts',(-0.153037544712885,0.0765254034509632,
3.176371571077));
#32487=CARTESIAN_POINT('Ctrl Pts',(-0.0195857505107214,0.169979486532972,
3.16847433655116));
#32488=CARTESIAN_POINT('Ctrl Pts',(0.131623058134361,0.109325193951073,
3.16057710202532));
#32489=CARTESIAN_POINT('Ctrl Pts',(0.163498551314534,-0.0504465180476298,
3.15267986749949));
#32490=CARTESIAN_POINT('Ctrl Pts',(0.0471414743157323,-0.164481940845858,
3.14478263297365));
#32491=CARTESIAN_POINT('Ctrl Pts',(-0.111955442538922,-0.129393223744503,
3.13688539844782));
#32492=CARTESIAN_POINT('Ctrl Pts',(-0.169550279652557,0.0230071757245571,
3.12898816392198));
#32493=CARTESIAN_POINT('Ctrl Pts',(-0.0734258726175858,0.154548596549523,
3.12109092939615));
#32494=CARTESIAN_POINT('Ctrl Pts',(0.0892685787892176,0.145971738038684,
3.11319369487031));
#32495=CARTESIAN_POINT('Ctrl Pts',(0.171029524891172,0.00505263105532012,
3.10529646034447));
#32496=CARTESIAN_POINT('Ctrl Pts',(0.0977300998321875,-0.140447339070101,
3.09739922581864));
#32497=CARTESIAN_POINT('Ctrl Pts',(-0.0641742930720691,-0.158613642457959,
3.0895019912928));
#32498=CARTESIAN_POINT('Ctrl Pts',(-0.167896394298454,-0.0329761769563863,
3.08160475676697));
#32499=CARTESIAN_POINT('Ctrl Pts',(-0.119398712226798,0.122558455374011,
3.07370752224113));
#32500=CARTESIAN_POINT('Ctrl Pts',(0.0373493356562941,0.166978006309557,
3.0658102877153));
#32501=CARTESIAN_POINT('Ctrl Pts',(0.160235383085578,0.0600104113675208,
3.05791305318946));
#32502=CARTESIAN_POINT('Ctrl Pts',(0.13784734412437,-0.101364378274316,
3.05001581866363));
#32503=CARTESIAN_POINT('Ctrl Pts',(-0.00951713008727486,-0.170839256905381,
3.04211858413779));
#32504=CARTESIAN_POINT('Ctrl Pts',(-0.148253095714458,-0.0854262668981903,
3.03422134961195));
#32505=CARTESIAN_POINT('Ctrl Pts',(-0.152578467253459,0.0774366760370435,
3.02632411508612));
#32506=CARTESIAN_POINT('Ctrl Pts',(-0.0185717363175075,0.170093262874324,
3.01842688056029));
#32507=CARTESIAN_POINT('Ctrl Pts',(0.132272674126287,0.10853832108782,3.01052964603445));
#32508=CARTESIAN_POINT('Ctrl Pts',(0.163194808240755,-0.051420638155743,
3.00263241150862));
#32509=CARTESIAN_POINT('Ctrl Pts',(0.0461597545337032,-0.164760142408496,
2.99473517698277));
#32510=CARTESIAN_POINT('Ctrl Pts',(-0.112725083152171,-0.128723281085519,
2.98683794245694));
#32511=CARTESIAN_POINT('Ctrl Pts',(-0.169410062399277,0.024017872989727,
2.9789407079311));
#32512=CARTESIAN_POINT('Ctrl Pts',(-0.0725029225620513,0.154983720709736,
2.97104347340527));
#32513=CARTESIAN_POINT('Ctrl Pts',(0.0901374881235442,0.145436792799793,
2.96314623887944));
#32514=CARTESIAN_POINT('Ctrl Pts',(0.171056614879515,0.00403261342178739,
2.95524900435359));
#32515=CARTESIAN_POINT('Ctrl Pts',(0.0968908098988563,-0.141027651268038,
2.94735176982777));
#32516=CARTESIAN_POINT('Ctrl Pts',(-0.0651190381186268,-0.158228121204172,
2.93945453530192));
#32517=CARTESIAN_POINT('Ctrl Pts',(-0.168090060956955,-0.0319743470970206,
2.93155730077609));
#32518=CARTESIAN_POINT('Ctrl Pts',(-0.118665716640764,0.123268305573731,
2.92366006625025));
#32519=CARTESIAN_POINT('Ctrl Pts',(0.0383444382474168,0.166752305897243,
2.91576283172442));
#32520=CARTESIAN_POINT('Ctrl Pts',(0.160590403549885,0.0590537869267172,
2.90786559719859));
#32521=CARTESIAN_POINT('Ctrl Pts',(0.137240410538441,-0.102184623010809,
2.89996836267275));
#32522=CARTESIAN_POINT('Ctrl Pts',(-0.0105357540088883,-0.170779464111837,
2.89207112814692));
#32523=CARTESIAN_POINT('Ctrl Pts',(-0.14875989566084,-0.0845406463731019,
2.88417389362107));
#32524=CARTESIAN_POINT('Ctrl Pts',(-0.152113963683294,0.0783451946269418,
2.87627665909525));
#32525=CARTESIAN_POINT('Ctrl Pts',(-0.0175570615310977,0.170200990355554,
2.86837942456941));
#32526=CARTESIAN_POINT('Ctrl Pts',(0.132917585844673,0.10774758787922,2.86048219004357));
#32527=CARTESIAN_POINT('Ctrl Pts',(0.162885261897846,-0.0523929288553319,
2.85258495551774));
#32528=CARTESIAN_POINT('Ctrl Pts',(0.0451763922858567,-0.165032485976878,
2.8446877209919));
#32529=CARTESIAN_POINT('Ctrl Pts',(-0.113490713213303,-0.128048757924713,
2.83679048646607));
#32530=CARTESIAN_POINT('Ctrl Pts',(-0.169263823638604,0.0250277109206782,
2.82889325194023));
#32531=CARTESIAN_POINT('Ctrl Pts',(-0.0715773878139425,0.15541334312893,
2.82099601741439));
#32532=CARTESIAN_POINT('Ctrl Pts',(0.0910031798397666,0.144896656177581,
2.81309878288856));
#32533=CARTESIAN_POINT('Ctrl Pts',(0.171077644724872,0.00301248930052715,
2.80520154836272));
#32534=CARTESIAN_POINT('Ctrl Pts',(0.0960480296290492,-0.141603019127657,
2.79730431383689));
#32535=CARTESIAN_POINT('Ctrl Pts',(-0.0660613815197478,-0.157836836132188,
2.78940707931105));
#32536=CARTESIAN_POINT('Ctrl Pts',(-0.168277914911174,-0.0309716432198527,
2.78150984478522));
#32537=CARTESIAN_POINT('Ctrl Pts',(-0.11792818320716,0.123974278216523,
2.77361261025938));
#32538=CARTESIAN_POINT('Ctrl Pts',(0.0393375658179575,0.166519701078062,
2.76571537573355));
#32539=CARTESIAN_POINT('Ctrl Pts',(0.160940889343806,0.0580969368916377,
2.75781814120771));
#32540=CARTESIAN_POINT('Ctrl Pts',(0.136626332479664,-0.103004840866145,
2.74992090668187));
#32541=CARTESIAN_POINT('Ctrl Pts',(-0.011549647108527,-0.170706656610813,
2.74202367215604));
#32542=CARTESIAN_POINT('Ctrl Pts',(-0.149269788191131,-0.0836653780051494,
2.7341264376302));
#32543=CARTESIAN_POINT('Ctrl Pts',(-0.151627913553235,0.0792766508469352,
2.72622920310437));
#32544=CARTESIAN_POINT('Ctrl Pts',(-0.0165728695680367,0.170252994451239,
2.71833196857853));
#32545=CARTESIAN_POINT('Ctrl Pts',(0.133618150071337,0.107050204730652,
2.7104347340527));
#32546=CARTESIAN_POINT('Ctrl Pts',(0.162448849852474,-0.0535653340983903,
2.70253749952686));
#32547=CARTESIAN_POINT('Ctrl Pts',(0.0837975063399687,-0.127706922146391,
2.69727267650963));
#32548=CARTESIAN_POINT('Ctrl Pts',(0.0374537582415302,-0.140096572423083,
2.69464026500102));
#32549=CARTESIAN_POINT('Ctrl Pts',(0.116913659442517,0.100696009035906,
3.61607920499693));
#32550=CARTESIAN_POINT('Ctrl Pts',(0.150223756874345,0.0620211357769951,
3.61344679348832));
#32551=CARTESIAN_POINT('Ctrl Pts',(0.174912072379498,-0.0503050113773498,
3.60818197047109));
#32552=CARTESIAN_POINT('Ctrl Pts',(0.0532769234891989,-0.174207647205754,
3.60028473594526));
#32553=CARTESIAN_POINT('Ctrl Pts',(-0.11663787696255,-0.139723112036145,
3.59238750141943));
#32554=CARTESIAN_POINT('Ctrl Pts',(-0.180814450120624,0.0212164448017569,
3.58449026689359));
#32555=CARTESIAN_POINT('Ctrl Pts',(-0.0810549264538156,0.163034932450524,
3.57659303236775));
#32556=CARTESIAN_POINT('Ctrl Pts',(0.0921890963056651,0.156981846810788,
3.56869579784192));
#32557=CARTESIAN_POINT('Ctrl Pts',(0.181852962765875,0.00863524897295638,
3.56079856331608));
#32558=CARTESIAN_POINT('Ctrl Pts',(0.10664300202618,-0.147556335146073,
3.55290132879024));
#32559=CARTESIAN_POINT('Ctrl Pts',(-0.0652523071804818,-0.169960705131912,
3.54500409426442));
#32560=CARTESIAN_POINT('Ctrl Pts',(-0.177988130457198,-0.0382780528074994,
3.53710685973857));
#32561=CARTESIAN_POINT('Ctrl Pts',(-0.129354621491586,0.128110850036879,
3.52920962521275));
#32562=CARTESIAN_POINT('Ctrl Pts',(0.0365555273815534,0.178349539831362,
3.52131239068689));
#32563=CARTESIAN_POINT('Ctrl Pts',(0.169323388748115,0.0668919258489962,
3.51341515616108));
#32564=CARTESIAN_POINT('Ctrl Pts',(0.148577699872602,-0.105212180693424,
3.50551792163523));
#32565=CARTESIAN_POINT('Ctrl Pts',(-0.00687287246844015,-0.181927682017732,
3.4976206871094));
#32566=CARTESIAN_POINT('Ctrl Pts',(-0.156092300794361,-0.0937023092829102,
3.48972345258356));
#32567=CARTESIAN_POINT('Ctrl Pts',(-0.163793880663394,0.0794763628218631,
3.48182621805772));
#32568=CARTESIAN_POINT('Ctrl Pts',(-0.0229951370022999,0.180599416102118,
3.47392898353189));
#32569=CARTESIAN_POINT('Ctrl Pts',(0.138651671100891,0.117985766817156,
3.46603174900605));
#32570=CARTESIAN_POINT('Ctrl Pts',(0.174592817347261,-0.0515972368462645,
3.45813451448022));
#32571=CARTESIAN_POINT('Ctrl Pts',(0.0522430073621133,-0.174400672749591,
3.45023727995438));
#32572=CARTESIAN_POINT('Ctrl Pts',(-0.117471841660763,-0.139087357890593,
3.44234004542855));
#32573=CARTESIAN_POINT('Ctrl Pts',(-0.180683282069521,0.0223266258512126,
3.43444281090271));
#32574=CARTESIAN_POINT('Ctrl Pts',(-0.0800819726320239,0.163498636922,3.42654557637688));
#32575=CARTESIAN_POINT('Ctrl Pts',(0.0931239962001525,0.156438000435139,
3.41864834185104));
#32576=CARTESIAN_POINT('Ctrl Pts',(0.181901025498224,0.00754609564814438,
3.41075110732521));
#32577=CARTESIAN_POINT('Ctrl Pts',(0.10576126311461,-0.148187320169658,
3.40285387279937));
#32578=CARTESIAN_POINT('Ctrl Pts',(-0.0662647547190597,-0.169569775965683,
3.39495663827354));
#32579=CARTESIAN_POINT('Ctrl Pts',(-0.178213207183381,-0.0372153116680257,
3.3870594037477));
#32580=CARTESIAN_POINT('Ctrl Pts',(-0.128588351944475,0.128879643005541,
3.37916216922186));
#32581=CARTESIAN_POINT('Ctrl Pts',(0.0376184653398806,0.178128542640067,
3.37126493469602));
#32582=CARTESIAN_POINT('Ctrl Pts',(0.169719281325138,0.0658808939206553,
3.36336770017019));
#32583=CARTESIAN_POINT('Ctrl Pts',(0.14794763130091,-0.10609630073556,3.35547046564435));
#32584=CARTESIAN_POINT('Ctrl Pts',(-0.00795766983708003,-0.181883485034118,
3.34757323111852));
#32585=CARTESIAN_POINT('Ctrl Pts',(-0.156648314679315,-0.0927697803461756,
3.33967599659268));
#32586=CARTESIAN_POINT('Ctrl Pts',(-0.163317014296801,0.0804517214143475,
3.33177876206685));
#32587=CARTESIAN_POINT('Ctrl Pts',(-0.0219177305069036,0.180733338725286,
3.32388152754101));
#32588=CARTESIAN_POINT('Ctrl Pts',(0.139352809018331,0.117156823343995,
3.31598429301518));
#32589=CARTESIAN_POINT('Ctrl Pts',(0.174282014774141,-0.0526374957955154,
3.30808705848934));
#32590=CARTESIAN_POINT('Ctrl Pts',(0.0512020468814229,-0.174709121205821,
3.3001898239635));
#32591=CARTESIAN_POINT('Ctrl Pts',(-0.118299194757364,-0.13838434578057,
3.29229258943767));
#32592=CARTESIAN_POINT('Ctrl Pts',(-0.180546925291626,0.0234037263079457,
3.28439535491183));
#32593=CARTESIAN_POINT('Ctrl Pts',(-0.0791055310066521,0.163973295391393,
3.27649812038601));
#32594=CARTESIAN_POINT('Ctrl Pts',(0.0940552521182287,0.155879877425964,
3.26860088586016));
#32595=CARTESIAN_POINT('Ctrl Pts',(0.181942791852133,0.00646120193221371,
3.26070365133433));
#32596=CARTESIAN_POINT('Ctrl Pts',(0.104875673303493,-0.148815388271832,
3.25280641680849));
#32597=CARTESIAN_POINT('Ctrl Pts',(-0.067274799061048,-0.169171593503912,
3.24490918228266));
#32598=CARTESIAN_POINT('Ctrl Pts',(-0.178431970305088,-0.0361518825291525,
3.23701194775682));
#32599=CARTESIAN_POINT('Ctrl Pts',(-0.127817496798961,0.129644182859876,
3.22911471323099));
#32600=CARTESIAN_POINT('Ctrl Pts',(0.0386800589242284,0.177901039004767,
3.22121747870515));
#32601=CARTESIAN_POINT('Ctrl Pts',(0.170109141545278,0.0648676082500797,
3.21332024417931));
#32602=CARTESIAN_POINT('Ctrl Pts',(0.147312299474883,-0.106976694007524,
3.20542300965349));
#32603=CARTESIAN_POINT('Ctrl Pts',(-0.00904218328755787,-0.18183279560836,
3.19752577512764));
#32604=CARTESIAN_POINT('Ctrl Pts',(-0.157198758129913,-0.0918339647394704,
3.18962854060181));
#32605=CARTESIAN_POINT('Ctrl Pts',(-0.162834339610607,0.0814242253935201,
3.18173130607597));
#32606=CARTESIAN_POINT('Ctrl Pts',(-0.0208395446762738,0.180860830516292,
3.17383407155014));
#32607=CARTESIAN_POINT('Ctrl Pts',(0.140048991174337,0.116323715159066,
3.1659368370243));
#32608=CARTESIAN_POINT('Ctrl Pts',(0.173965014144346,-0.0536758837012937,
3.15803960249847));
#32609=CARTESIAN_POINT('Ctrl Pts',(0.050159265511441,-0.175011355976434,
3.15014236797263));
#32610=CARTESIAN_POINT('Ctrl Pts',(-0.119122340768341,-0.137676412530354,
3.14224513344679));
#32611=CARTESIAN_POINT('Ctrl Pts',(-0.180404147686861,0.0244799945819963,
3.13434789892096));
#32612=CARTESIAN_POINT('Ctrl Pts',(-0.0781262761399388,0.164442122383114,
3.12645066439512));
#32613=CARTESIAN_POINT('Ctrl Pts',(0.0949831631341886,0.155316210867962,
3.11855342986929));
#32614=CARTESIAN_POINT('Ctrl Pts',(0.181978087741923,0.00537607841744088,
3.11065619534345));
#32615=CARTESIAN_POINT('Ctrl Pts',(0.10398635378076,-0.149438164016893,
3.10275896081762));
#32616=CARTESIAN_POINT('Ctrl Pts',(-0.0682824508977375,-0.168767394767933,
3.09486172629178));
#32617=CARTESIAN_POINT('Ctrl Pts',(-0.178644387819226,-0.0350871677120128,
3.08696449176594));
#32618=CARTESIAN_POINT('Ctrl Pts',(-0.127042096057429,0.130404112154074,
3.07906725724011));
#32619=CARTESIAN_POINT('Ctrl Pts',(0.039740276922879,0.17766720864428,3.07117002271427));
#32620=CARTESIAN_POINT('Ctrl Pts',(0.170492952144154,0.0638520156810144,
3.06327278818844));
#32621=CARTESIAN_POINT('Ctrl Pts',(0.146671728755708,-0.107853282848364,
3.0553755536626));
#32622=CARTESIAN_POINT('Ctrl Pts',(-0.0101263751692898,-0.181775639631079,
3.04747831913677));
#32623=CARTESIAN_POINT('Ctrl Pts',(-0.15774361109349,-0.0908948832253125,
3.03958108461093));
#32624=CARTESIAN_POINT('Ctrl Pts',(-0.162345874018219,0.0823938336686527,
3.0316838500851));
#32625=CARTESIAN_POINT('Ctrl Pts',(-0.0197606177252597,0.180981890321858,
3.02378661555926));
#32626=CARTESIAN_POINT('Ctrl Pts',(0.140740192743497,0.115486470133437,
3.01588938103343));
#32627=CARTESIAN_POINT('Ctrl Pts',(0.173641826766224,-0.0547123627222005,
3.00799214650759));
#32628=CARTESIAN_POINT('Ctrl Pts',(0.0491147003187017,-0.175307366787479,
3.00009491198175));
#32629=CARTESIAN_POINT('Ctrl Pts',(-0.119941250410619,-0.136963583069732,
2.99219767745592));
#32630=CARTESIAN_POINT('Ctrl Pts',(-0.180254954337721,0.0255553922697266,
2.98430044293008));
#32631=CARTESIAN_POINT('Ctrl Pts',(-0.0771442428547834,0.164905101290741,
2.97640320840425));
#32632=CARTESIAN_POINT('Ctrl Pts',(0.0959076962473017,0.15474702077238,
2.96850597387841));
#32633=CARTESIAN_POINT('Ctrl Pts',(0.182006911912947,0.00429076371209153,
2.96060873935257));
#32634=CARTESIAN_POINT('Ctrl Pts',(0.103093336173269,-0.150055625266004,
2.95271150482674));
#32635=CARTESIAN_POINT('Ctrl Pts',(-0.069287674394006,-0.168357194128057,
2.9448142703009));
#32636=CARTESIAN_POINT('Ctrl Pts',(-0.178850452170956,-0.0340212050826592,
2.93691703577507));
#32637=CARTESIAN_POINT('Ctrl Pts',(-0.126262177296885,0.131159403861809,
2.92901980124923));
#32638=CARTESIAN_POINT('Ctrl Pts',(0.0407990816336726,0.177427059877793,
2.9211225667234));
#32639=CARTESIAN_POINT('Ctrl Pts',(0.170870699467283,0.0628341523235889,
2.91322533219756));
#32640=CARTESIAN_POINT('Ctrl Pts',(0.146025941933673,-0.108726036068736,
2.90532809767173));
#32641=CARTESIAN_POINT('Ctrl Pts',(-0.0112102069433731,-0.181712019164164,
2.89743086314589));
#32642=CARTESIAN_POINT('Ctrl Pts',(-0.158282854157919,-0.0899525691440268,
2.88953362862006));
#32643=CARTESIAN_POINT('Ctrl Pts',(-0.161851634959193,0.0833605116488022,
2.88163639409422));
#32644=CARTESIAN_POINT('Ctrl Pts',(-0.0186809878927599,0.181096514045709,
2.87373915956839));
#32645=CARTESIAN_POINT('Ctrl Pts',(0.14142638889208,0.114645117640021,2.86584192504255));
#32646=CARTESIAN_POINT('Ctrl Pts',(0.173312464619039,-0.0557468952238434,
2.85794469051671));
#32647=CARTESIAN_POINT('Ctrl Pts',(0.0480683875166603,-0.175597144601074,
2.85004745599088));
#32648=CARTESIAN_POINT('Ctrl Pts',(-0.120755892762759,-0.136245879883575,
2.84215022146504));
#32649=CARTESIAN_POINT('Ctrl Pts',(-0.180099354010596,0.0266298756124168,
2.83425298693921));
#32650=CARTESIAN_POINT('Ctrl Pts',(-0.0761594594163292,0.165362226259928,
2.82635575241337));
#32651=CARTESIAN_POINT('Ctrl Pts',(0.0968288057644592,0.154172306963803,
2.81845851788754));
#32652=CARTESIAN_POINT('Ctrl Pts',(0.182029287997112,0.0032053357021354,
2.8105612833617));
#32653=CARTESIAN_POINT('Ctrl Pts',(0.102196604793212,-0.150667825661861,
2.80266404883587));
#32654=CARTESIAN_POINT('Ctrl Pts',(-0.0702903425019912,-0.167940860695529,
2.79476681431002));
#32655=CARTESIAN_POINT('Ctrl Pts',(-0.179050331714475,-0.0329543124847025,
2.7868695797842));
#32656=CARTESIAN_POINT('Ctrl Pts',(-0.125477430195597,0.131910569788365,
2.77897234525835));
#32657=CARTESIAN_POINT('Ctrl Pts',(0.0418557848916964,0.17717956471448,
2.77107511073252));
#32658=CARTESIAN_POINT('Ctrl Pts',(0.171243621830244,0.0618160489303277,
2.76317787620668));
#32659=CARTESIAN_POINT('Ctrl Pts',(0.145372553280857,-0.109598760687136,
2.75528064168085));
#32660=CARTESIAN_POINT('Ctrl Pts',(-0.0122890050489303,-0.181634550845065,
2.74738340715501));
#32661=CARTESIAN_POINT('Ctrl Pts',(-0.158825387779967,-0.0890212699197419,
2.73948617262918));
#32662=CARTESIAN_POINT('Ctrl Pts',(-0.161334470023658,0.0843515956258966,
2.73158893810334));
#32663=CARTESIAN_POINT('Ctrl Pts',(-0.0176337922607613,0.181151847216363,
2.72369170357751));
#32664=CARTESIAN_POINT('Ctrl Pts',(0.14217180017934,0.113903091069576,2.71579446905167));
#32665=CARTESIAN_POINT('Ctrl Pts',(0.172848115381474,-0.0569943527276058,
2.70789723452584));
#32666=CARTESIAN_POINT('Ctrl Pts',(0.0891618565332066,-0.135882161272415,
2.70263241150861));
#32667=CARTESIAN_POINT('Ctrl Pts',(0.0398513841857358,-0.149064942821848,
2.7));
#32668=CARTESIAN_POINT('Ctrl Pts',(0.0958116152722374,0.0825211298936506,
3.6));
#32669=CARTESIAN_POINT('Ctrl Pts',(0.102493614798766,0.0762810303731869,
3.6));
#32670=CARTESIAN_POINT('Ctrl Pts',(0.108396094096263,0.0693090539021388,
3.6));
#32671=CARTESIAN_POINT('Ctrl Pts',(0.113512571306729,0.0617846659987563,
3.6));
#32672=CARTESIAN_POINT('Ctrl Pts',(0.117461600031764,0.0559771498608983,
3.6));
#32673=CARTESIAN_POINT('Ctrl Pts',(0.120942091267611,0.0498392138898472,
3.6));
#32674=CARTESIAN_POINT('Ctrl Pts',(0.123938893544148,0.0434377969520944,
3.6));
#32675=CARTESIAN_POINT('Ctrl Pts',(0.125176287448039,0.0407946214723323,
3.6));
#32676=CARTESIAN_POINT('Ctrl Pts',(0.126329312445263,0.0381097373250835,
3.6));
#32677=CARTESIAN_POINT('Ctrl Pts',(0.12739426777321,0.0353959223183902,
3.6));
#32678=CARTESIAN_POINT('Ctrl Pts',(0.130992400282108,0.0262268372474364,
3.6));
#32679=CARTESIAN_POINT('Ctrl Pts',(0.13360037697833,0.0167048680256365,
3.6));
#32680=CARTESIAN_POINT('Ctrl Pts',(0.135185783736742,0.0070125550480467,
3.6));
#32681=CARTESIAN_POINT('Ctrl Pts',(0.135855615028331,0.00291757154566029,
3.6));
#32682=CARTESIAN_POINT('Ctrl Pts',(0.13634239472836,-0.00120821237992505,
3.6));
#32683=CARTESIAN_POINT('Ctrl Pts',(0.136641151680689,-0.0053522141362822,
3.6));
#32684=CARTESIAN_POINT('Ctrl Pts',(0.136866179264237,-0.00847352962091436,
3.6));
#32685=CARTESIAN_POINT('Ctrl Pts',(0.136984148876184,-0.0116047424016575,
3.6));
#32686=CARTESIAN_POINT('Ctrl Pts',(0.136993305813875,-0.0147266162095009,
3.6));
#32687=CARTESIAN_POINT('Ctrl Pts',(0.1370171880242,-0.0228687756739225,
3.6));
#32688=CARTESIAN_POINT('Ctrl Pts',(0.1363045911537,-0.0309705737407376,
3.6));
#32689=CARTESIAN_POINT('Ctrl Pts',(0.134831565375878,-0.0389361856515032,
3.6));
#32690=CARTESIAN_POINT('Ctrl Pts',(0.133932184221546,-0.043799726631656,
3.6));
#32691=CARTESIAN_POINT('Ctrl Pts',(0.132748938308619,-0.0486126850413777,
3.6));
#32692=CARTESIAN_POINT('Ctrl Pts',(0.131298540463925,-0.0533602760289537,
3.6));
#32693=CARTESIAN_POINT('Ctrl Pts',(0.130441077796828,-0.0561670107778959,
3.6));
#32694=CARTESIAN_POINT('Ctrl Pts',(0.129489770756279,-0.058951963571448,
3.6));
#32695=CARTESIAN_POINT('Ctrl Pts',(0.128448797183808,-0.061708664264176,
3.6));
#32696=CARTESIAN_POINT('Ctrl Pts',(0.124844109667278,-0.0712545786242284,
3.6));
#32697=CARTESIAN_POINT('Ctrl Pts',(0.120197621014249,-0.0803872939153616,
3.6));
#32698=CARTESIAN_POINT('Ctrl Pts',(0.114666430721154,-0.0889848980033025,
3.6));
#32699=CARTESIAN_POINT('Ctrl Pts',(0.111763941762871,-0.0934964858552134,
3.6));
#32700=CARTESIAN_POINT('Ctrl Pts',(0.108616890563154,-0.0978607268708147,
3.6));
#32701=CARTESIAN_POINT('Ctrl Pts',(0.105242483611131,-0.102058774522217,
3.6));
#32702=CARTESIAN_POINT('Ctrl Pts',(0.103051571759935,-0.104784454169668,
3.6));
#32703=CARTESIAN_POINT('Ctrl Pts',(0.100763130867069,-0.107441777418394,
3.6));
#32704=CARTESIAN_POINT('Ctrl Pts',(0.098386472215756,-0.110019467506635,
3.6));
#32705=CARTESIAN_POINT('Ctrl Pts',(0.0926299038901994,-0.116262959438837,
3.6));
#32706=CARTESIAN_POINT('Ctrl Pts',(0.0863771877690887,-0.12201951201926,
3.6));
#32707=CARTESIAN_POINT('Ctrl Pts',(0.0796980248685607,-0.127218319244159,
3.6));
#32708=CARTESIAN_POINT('Ctrl Pts',(0.0749983795646852,-0.130876345006388,
3.6));
#32709=CARTESIAN_POINT('Ctrl Pts',(0.0700820293375014,-0.134260491890013,
3.6));
#32710=CARTESIAN_POINT('Ctrl Pts',(0.064997448628775,-0.137327043702736,
3.6));
#32711=CARTESIAN_POINT('Ctrl Pts',(0.0586168958330981,-0.141175206779031,
3.6));
#32712=CARTESIAN_POINT('Ctrl Pts',(0.0519659322704503,-0.144529310638398,
3.6));
#32713=CARTESIAN_POINT('Ctrl Pts',(0.0450857487477646,-0.147337352418514,
3.6));
#32714=CARTESIAN_POINT('Ctrl Pts',(0.0433856322299594,-0.148031228998597,
3.6));
#32715=CARTESIAN_POINT('Ctrl Pts',(0.0416714833555574,-0.148691718060548,
3.6));
#32716=CARTESIAN_POINT('Ctrl Pts',(0.0399441988940855,-0.149319076597487,
3.6));
#32717=CARTESIAN_POINT('Ctrl Pts',(-0.126474550616365,-0.00011099430647141,
3.51934196736194));
#32718=CARTESIAN_POINT('Ctrl Pts',(-0.126555547962724,-0.00903265450993761,
3.51990386315518));
#32719=CARTESIAN_POINT('Ctrl Pts',(-0.125690900286005,-0.0179387227435883,
3.52046575894841));
#32720=CARTESIAN_POINT('Ctrl Pts',(-0.123822037714229,-0.0266288110680491,
3.52102765474165));
#32721=CARTESIAN_POINT('Ctrl Pts',(-0.115066650325334,-0.0673407879000796,
3.52366006625026));
#32722=CARTESIAN_POINT('Ctrl Pts',(-0.0842707011930362,-0.103312426237565,
3.52629247775887));
#32723=CARTESIAN_POINT('Ctrl Pts',(-0.0453944787880641,-0.118238154042396,
3.52892488926748));
#32724=CARTESIAN_POINT('Ctrl Pts',(-0.00651825638309213,-0.133163881847227,
3.53155730077609));
#32725=CARTESIAN_POINT('Ctrl Pts',(0.0404382392945539,-0.127043699119404,
3.5341897122847));
#32726=CARTESIAN_POINT('Ctrl Pts',(0.0741890076945504,-0.102650246541568,
3.53682212379332));
#32727=CARTESIAN_POINT('Ctrl Pts',(0.107939776094547,-0.0782567939637322,
3.53945453530193));
#32728=CARTESIAN_POINT('Ctrl Pts',(0.128484817216894,-0.0355900715358833,
3.54208694681054));
#32729=CARTESIAN_POINT('Ctrl Pts',(0.126510636639707,0.00600514677092718,
3.54471935831915));
#32730=CARTESIAN_POINT('Ctrl Pts',(0.124536456062521,0.0476003650777378,
3.54735176982776));
#32731=CARTESIAN_POINT('Ctrl Pts',(0.100043053785802,0.0881240792635097,
3.54998418133637));
#32732=CARTESIAN_POINT('Ctrl Pts',(0.0641338913405327,0.109212694488978,
3.55261659284499));
#32733=CARTESIAN_POINT('Ctrl Pts',(0.028224728895264,0.130301309714446,
3.5552490043536));
#32734=CARTESIAN_POINT('Ctrl Pts',(-0.019100193718554,0.13195482597961,
3.55788141586221));
#32735=CARTESIAN_POINT('Ctrl Pts',(-0.0563882672178024,0.113411366178312,
3.56051382737082));
#32736=CARTESIAN_POINT('Ctrl Pts',(-0.0936763407170509,0.0948679063770136,
3.56314623887943));
#32737=CARTESIAN_POINT('Ctrl Pts',(-0.12092756510173,0.0561274705092526,
3.56577865038805));
#32738=CARTESIAN_POINT('Ctrl Pts',(-0.125787647292084,0.0147753915231441,
3.56841106189666));
#32739=CARTESIAN_POINT('Ctrl Pts',(-0.126360541139662,0.00990091600857084,
3.56872136371842));
#32740=CARTESIAN_POINT('Ctrl Pts',(-0.126622308248343,0.0049901515008091,
3.56903166554018));
#32741=CARTESIAN_POINT('Ctrl Pts',(-0.126585968300139,7.56654190205153E-5,
3.56934196736194));
#32742=CARTESIAN_POINT('Ctrl Pts',(-0.0398513841857247,-0.149064942821851,
3.6));
#32743=CARTESIAN_POINT('Ctrl Pts',(-0.0891618565331957,-0.135882161272422,
3.59736758849139));
#32744=CARTESIAN_POINT('Ctrl Pts',(-0.17284812802765,-0.0569944292149041,
3.59210276547417));
#32745=CARTESIAN_POINT('Ctrl Pts',(-0.142171789002704,0.113903133580536,
3.58420553094833));
#32746=CARTESIAN_POINT('Ctrl Pts',(0.0176337902165689,0.181151815132919,
3.5763082964225));
#32747=CARTESIAN_POINT('Ctrl Pts',(0.161334465098627,0.0843516096779105,
3.56841106189666));
#32748=CARTESIAN_POINT('Ctrl Pts',(0.158825384561566,-0.0890212772063117,
3.56051382737082));
#32749=CARTESIAN_POINT('Ctrl Pts',(0.0122890037691484,-0.181634540286447,
3.55261659284499));
#32750=CARTESIAN_POINT('Ctrl Pts',(-0.145372548664834,-0.109598761010981,
3.54471935831915));
#32751=CARTESIAN_POINT('Ctrl Pts',(-0.171243617690229,0.0618160491398297,
3.53682212379332));
#32752=CARTESIAN_POINT('Ctrl Pts',(-0.0418557834629445,0.177179558878914,
3.52892488926748));
#32753=CARTESIAN_POINT('Ctrl Pts',(0.125477426630257,0.13191056683484,3.52102765474164));
#32754=CARTESIAN_POINT('Ctrl Pts',(0.179050327003836,-0.0329543119327003,
3.51313042021581));
#32755=CARTESIAN_POINT('Ctrl Pts',(0.0702903405429243,-0.167940855985405,
3.50523318568997));
#32756=CARTESIAN_POINT('Ctrl Pts',(-0.102196602002365,-0.150667821707605,
3.49733595116413));
#32757=CARTESIAN_POINT('Ctrl Pts',(-0.182029283116568,0.00320533567306586,
3.4894387166383));
#32758=CARTESIAN_POINT('Ctrl Pts',(-0.0968288031440013,0.15417230277993,
3.48154148211247));
#32759=CARTESIAN_POINT('Ctrl Pts',(0.0761594573579975,0.165362221823523,
3.47364424758663));
#32760=CARTESIAN_POINT('Ctrl Pts',(0.180099349163956,0.0266298748857393,
3.46574701306079));
#32761=CARTESIAN_POINT('Ctrl Pts',(0.120755889508211,-0.136245876208876,
3.45784977853496));
#32762=CARTESIAN_POINT('Ctrl Pts',(-0.0480683862207756,-0.175597139874519,
3.44995254400912));
#32763=CARTESIAN_POINT('Ctrl Pts',(-0.173312459951882,-0.0557468937208932,
3.44205530948329));
#32764=CARTESIAN_POINT('Ctrl Pts',(-0.141426385082663,0.114645114551432,
3.43415807495745));
#32765=CARTESIAN_POINT('Ctrl Pts',(0.0186809873893989,0.181096509168673,
3.42626084043161));
#32766=CARTESIAN_POINT('Ctrl Pts',(0.161851630600137,0.0833605094034181,
3.41836360590578));
#32767=CARTESIAN_POINT('Ctrl Pts',(0.158282849894819,-0.0899525667211824,
3.41046637137994));
#32768=CARTESIAN_POINT('Ctrl Pts',(0.0112102066414966,-0.181712014270169,
3.40256913685411));
#32769=CARTESIAN_POINT('Ctrl Pts',(-0.146025938000753,-0.108726033140384,
3.39467190232827));
#32770=CARTESIAN_POINT('Ctrl Pts',(-0.170870694865204,0.0628341506312357,
3.38677466780244));
#32771=CARTESIAN_POINT('Ctrl Pts',(-0.0407990805348497,0.177427055099143,
3.3788774332766));
#32772=CARTESIAN_POINT('Ctrl Pts',(0.126262173896246,0.131159400329288,
3.37098019875077));
#32773=CARTESIAN_POINT('Ctrl Pts',(0.178850447353964,-0.0340212041663437,
3.36308296422493));
#32774=CARTESIAN_POINT('Ctrl Pts',(0.0692876725278909,-0.168357189593675,
3.3551857296991));
#32775=CARTESIAN_POINT('Ctrl Pts',(-0.103093333396635,-0.150055621224551,
3.34728849517326));
#32776=CARTESIAN_POINT('Ctrl Pts',(-0.18200690701094,0.00429076359651101,
3.33939126064742));
#32777=CARTESIAN_POINT('Ctrl Pts',(-0.0959076936642258,0.154747016604558,
3.33149402612159));
#32778=CARTESIAN_POINT('Ctrl Pts',(0.0771442407770374,0.164905096849345,
3.32359679159575));
#32779=CARTESIAN_POINT('Ctrl Pts',(0.180254949482897,0.0255553915814562,
3.31569955706992));
#32780=CARTESIAN_POINT('Ctrl Pts',(0.119941247180243,-0.13696357938087,
3.30780232254408));
#32781=CARTESIAN_POINT('Ctrl Pts',(-0.0491146989958762,-0.175307362065916,
3.29990508801825));
#32782=CARTESIAN_POINT('Ctrl Pts',(-0.173641822089509,-0.0547123612486432,
3.29200785349241));
#32783=CARTESIAN_POINT('Ctrl Pts',(-0.14074018895294,0.115486467023018,
3.28411061896658));
#32784=CARTESIAN_POINT('Ctrl Pts',(0.0197606171930289,0.18098188544746,
3.27621338444074));
#32785=CARTESIAN_POINT('Ctrl Pts',(0.162345869645737,0.0823938314495476,
3.26831614991491));
#32786=CARTESIAN_POINT('Ctrl Pts',(0.157743606844976,-0.0908948807772195,
3.26041891538907));
#32787=CARTESIAN_POINT('Ctrl Pts',(0.0101263748965706,-0.181775634735301,
3.25252168086324));
#32788=CARTESIAN_POINT('Ctrl Pts',(-0.146671724805377,-0.107853279943556,
3.2446244463374));
#32789=CARTESIAN_POINT('Ctrl Pts',(-0.170492947552259,0.0638520139612676,
3.23672721181156));
#32790=CARTESIAN_POINT('Ctrl Pts',(-0.0397402758525677,0.177667203859151,
3.22882997728572));
#32791=CARTESIAN_POINT('Ctrl Pts',(0.127042092635782,0.130404108641901,
3.22093274275989));
#32792=CARTESIAN_POINT('Ctrl Pts',(0.178644383007786,-0.0350871667669908,
3.21303550823405));
#32793=CARTESIAN_POINT('Ctrl Pts',(0.0682824490586963,-0.1687673902225,
3.20513827370822));
#32794=CARTESIAN_POINT('Ctrl Pts',(-0.103986350980073,-0.149438159992073,
3.19724103918238));
#32795=CARTESIAN_POINT('Ctrl Pts',(-0.181978082840693,0.00537607827262928,
3.18934380465655));
#32796=CARTESIAN_POINT('Ctrl Pts',(-0.0949831605760139,0.155316206684809,
3.18144657013072));
#32797=CARTESIAN_POINT('Ctrl Pts',(0.0781262740357409,0.164442117954189,
3.17354933560488));
#32798=CARTESIAN_POINT('Ctrl Pts',(0.180404142828019,0.0244799939226929,
3.16565210107904));
#32799=CARTESIAN_POINT('Ctrl Pts',(0.119122337560023,-0.137676408822293,
3.15775486655321));
#32800=CARTESIAN_POINT('Ctrl Pts',(-0.0501592641604809,-0.175011351262844,
3.14985763202737));
#32801=CARTESIAN_POINT('Ctrl Pts',(-0.173965009458927,-0.0536758822556528,
3.14196039750153));
#32802=CARTESIAN_POINT('Ctrl Pts',(-0.140048987402398,0.116323712026096,
3.1340631629757));
#32803=CARTESIAN_POINT('Ctrl Pts',(0.0208395441149821,0.180860825645154,
3.12616592844986));
#32804=CARTESIAN_POINT('Ctrl Pts',(0.162834335224968,0.0814242232005321,
3.11826869392403));
#32805=CARTESIAN_POINT('Ctrl Pts',(0.157198753896076,-0.0918339622660831,
3.1103714593982));
#32806=CARTESIAN_POINT('Ctrl Pts',(0.00904218304404205,-0.181832790711041,
3.10247422487235));
#32807=CARTESIAN_POINT('Ctrl Pts',(-0.147312295507299,-0.106976691126326,
3.09457699034652));
#32808=CARTESIAN_POINT('Ctrl Pts',(-0.170109136963721,0.0648676065029794,
3.08667975582068));
#32809=CARTESIAN_POINT('Ctrl Pts',(-0.0386800578824722,0.177901034213339,
3.07878252129485));
#32810=CARTESIAN_POINT('Ctrl Pts',(0.127817493356429,0.129644179368171,
3.07088528676902));
#32811=CARTESIAN_POINT('Ctrl Pts',(0.178431965499368,-0.0361518815554529,
3.06298805224317));
#32812=CARTESIAN_POINT('Ctrl Pts',(0.0672747972491473,-0.169171588947593,
3.05509081771735));
#32813=CARTESIAN_POINT('Ctrl Pts',(-0.104875670478854,-0.148815384263785,
3.0471935831915));
#32814=CARTESIAN_POINT('Ctrl Pts',(-0.181942786951853,0.00646120175817659,
3.03929634866568));
#32815=CARTESIAN_POINT('Ctrl Pts',(-0.0940552495850459,0.15587987322763,
3.03139911413983));
#32816=CARTESIAN_POINT('Ctrl Pts',(0.0791055288760802,0.163973290975094,
3.02350187961401));
#32817=CARTESIAN_POINT('Ctrl Pts',(0.180546920428939,0.0234037256776295,
3.01560464508816));
#32818=CARTESIAN_POINT('Ctrl Pts',(0.118299191571216,-0.138384342053441,
3.00770741056233));
#32819=CARTESIAN_POINT('Ctrl Pts',(-0.0512020455023775,-0.174709116500372,
2.99981017603649));
#32820=CARTESIAN_POINT('Ctrl Pts',(-0.174282010080185,-0.0526374943778417,
2.99191294151066));
#32821=CARTESIAN_POINT('Ctrl Pts',(-0.139352805265142,0.117156820188587,
2.98401570698483));
#32822=CARTESIAN_POINT('Ctrl Pts',(0.0219177299165732,0.180733333857582,
2.97611847245899));
#32823=CARTESIAN_POINT('Ctrl Pts',(0.163317009898163,0.0804517192475515,
2.96822123793315));
#32824=CARTESIAN_POINT('Ctrl Pts',(0.156648310460303,-0.0927697778475837,
2.96032400340732));
#32825=CARTESIAN_POINT('Ctrl Pts',(0.00795766962277319,-0.181883480135435,
2.95242676888148));
#32826=CARTESIAN_POINT('Ctrl Pts',(-0.147947627316214,-0.106096297878073,
2.94452953435564));
#32827=CARTESIAN_POINT('Ctrl Pts',(-0.169719276754081,0.0658808921462626,
2.93663229982981));
#32828=CARTESIAN_POINT('Ctrl Pts',(-0.0376184643267171,0.178128537842515,
2.92873506530397));
#32829=CARTESIAN_POINT('Ctrl Pts',(0.128588348481182,0.128879639534425,
2.92083783077814));
#32830=CARTESIAN_POINT('Ctrl Pts',(0.178213202383553,-0.0372153106656781,
2.9129405962523));
#32831=CARTESIAN_POINT('Ctrl Pts',(0.0662647529343645,-0.169569771398652,
2.90504336172647));
#32832=CARTESIAN_POINT('Ctrl Pts',(-0.105761260266122,-0.148187316178505,
2.89714612720063));
#32833=CARTESIAN_POINT('Ctrl Pts',(-0.181901020599063,0.00754609544484455,
2.8892488926748));
#32834=CARTESIAN_POINT('Ctrl Pts',(-0.0931239936920636,0.15643799622185,
2.88135165814895));
#32835=CARTESIAN_POINT('Ctrl Pts',(0.080081970475175,0.163498632518342,
2.87345442362313));
#32836=CARTESIAN_POINT('Ctrl Pts',(0.180683277203119,0.0223266252501708,
2.86555718909729));
#32837=CARTESIAN_POINT('Ctrl Pts',(0.11747183849698,-0.139087354145018,
2.85765995457145));
#32838=CARTESIAN_POINT('Ctrl Pts',(-0.0522430059551858,-0.174400668051551,
2.84976272004562));
#32839=CARTESIAN_POINT('Ctrl Pts',(-0.174592812644639,-0.0515972354582594,
2.84186548551978));
#32840=CARTESIAN_POINT('Ctrl Pts',(-0.138651667367148,0.117985763642445,
2.83396825099395));
#32841=CARTESIAN_POINT('Ctrl Pts',(0.0229951363840201,0.180599411232496,
2.82607101646811));
#32842=CARTESIAN_POINT('Ctrl Pts',(0.163793876249876,0.0794763606914083,
2.81817378194228));
#32843=CARTESIAN_POINT('Ctrl Pts',(0.1560922965942,-0.0937023067775016,
2.81027654741644));
#32844=CARTESIAN_POINT('Ctrl Pts',(0.00687287227597422,-0.181927677084725,
2.8023793128906));
#32845=CARTESIAN_POINT('Ctrl Pts',(-0.148577695856893,-0.105212177919503,
2.79448207836477));
#32846=CARTESIAN_POINT('Ctrl Pts',(-0.169323384214447,0.0668919241546485,
2.78658484383893));
#32847=CARTESIAN_POINT('Ctrl Pts',(-0.0365555263461618,0.178349534836247,
2.7786876093131));
#32848=CARTESIAN_POINT('Ctrl Pts',(0.129354617910885,0.128110846926664,
2.77079037478726));
#32849=CARTESIAN_POINT('Ctrl Pts',(0.177988125847537,-0.0382780523762908,
2.76289314026143));
#32850=CARTESIAN_POINT('Ctrl Pts',(0.0652523050728403,-0.169960699505811,
2.75499590573559));
#32851=CARTESIAN_POINT('Ctrl Pts',(-0.106642998487829,-0.147556332986489,
2.74709867120975));
#32852=CARTESIAN_POINT('Ctrl Pts',(-0.181852959134814,0.00863525184135577,
2.73920143668392));
#32853=CARTESIAN_POINT('Ctrl Pts',(-0.0921890914137533,0.156981837366664,
2.73130420215808));
#32854=CARTESIAN_POINT('Ctrl Pts',(0.081054919689294,0.163034936656946,
2.72340696763225));
#32855=CARTESIAN_POINT('Ctrl Pts',(0.180814453969382,0.0212164304176998,
2.71550973310641));
#32856=CARTESIAN_POINT('Ctrl Pts',(0.116637857196403,-0.139723086682139,
2.70761249858058));
#32857=CARTESIAN_POINT('Ctrl Pts',(-0.0532768903028442,-0.174207676028794,
2.69971526405474));
#32858=CARTESIAN_POINT('Ctrl Pts',(-0.17491212592378,-0.0503049553127666,
2.69181802952891));
#32859=CARTESIAN_POINT('Ctrl Pts',(-0.150223756874352,0.0620211357769783,
2.68655320651168));
#32860=CARTESIAN_POINT('Ctrl Pts',(-0.116913659442528,0.100696009035893,
2.68392079500307));
#32861=CARTESIAN_POINT('Ctrl Pts',(-0.0374537582415199,-0.140096572423086,
3.60535973499898));
#32862=CARTESIAN_POINT('Ctrl Pts',(-0.0837975063399586,-0.127706922146397,
3.60272732349037));
#32863=CARTESIAN_POINT('Ctrl Pts',(-0.162448861737804,-0.0535654059838928,
3.59746250047314));
#32864=CARTESIAN_POINT('Ctrl Pts',(-0.133618139567134,0.107050244683975,
3.5895652659473));
#32865=CARTESIAN_POINT('Ctrl Pts',(0.0165728676468313,0.170252964298069,
3.58166803142147));
#32866=CARTESIAN_POINT('Ctrl Pts',(0.151627908924514,0.0792766640535213,
3.57377079689563));
#32867=CARTESIAN_POINT('Ctrl Pts',(0.149269785166362,-0.0836653848533289,
3.5658735623698));
#32868=CARTESIAN_POINT('Ctrl Pts',(0.0115496459057422,-0.170706646687446,
3.55797632784397));
#32869=CARTESIAN_POINT('Ctrl Pts',(-0.136626328141362,-0.103004841170506,
3.55007909331813));
#32870=CARTESIAN_POINT('Ctrl Pts',(-0.160940885452871,0.0580969370885353,
3.54218185879229));
#32871=CARTESIAN_POINT('Ctrl Pts',(-0.0393375644751653,0.166519695593587,
3.53428462426645));
#32872=CARTESIAN_POINT('Ctrl Pts',(0.117928179856326,0.123974275440694,
3.52638738974062));
#32873=CARTESIAN_POINT('Ctrl Pts',(0.168277910483947,-0.0309716427010613,
3.51849015521478));
#32874=CARTESIAN_POINT('Ctrl Pts',(0.0660613796785464,-0.157836831705444,
3.51059292068895));
#32875=CARTESIAN_POINT('Ctrl Pts',(-0.0960480270061105,-0.141603015411306,
3.50269568616311));
#32876=CARTESIAN_POINT('Ctrl Pts',(-0.171077640137963,0.00301248927320663,
3.49479845163728));
#32877=CARTESIAN_POINT('Ctrl Pts',(-0.0910031773769663,0.144896652245428,
3.48690121711144));
#32878=CARTESIAN_POINT('Ctrl Pts',(0.0715773858794485,0.155413338959437,
3.47900398258561));
#32879=CARTESIAN_POINT('Ctrl Pts',(0.169263819083558,0.0250277102377205,
3.47110674805977));
#32880=CARTESIAN_POINT('Ctrl Pts',(0.113490710154562,-0.128048754471099,
3.46320951353393));
#32881=CARTESIAN_POINT('Ctrl Pts',(-0.0451763910679377,-0.165032481534694,
3.4553122790081));
#32882=CARTESIAN_POINT('Ctrl Pts',(-0.162885257511484,-0.0523929274428053,
3.44741504448226));
#32883=CARTESIAN_POINT('Ctrl Pts',(-0.132917582264447,0.107747584976454,
3.43951780995643));
#32884=CARTESIAN_POINT('Ctrl Pts',(0.0175570610580211,0.17020098577194,
3.43162057543059));
#32885=CARTESIAN_POINT('Ctrl Pts',(0.152113959586497,0.0783451925166497,
3.42372334090476));
#32886=CARTESIAN_POINT('Ctrl Pts',(0.148759891654226,-0.0845406440960262,
3.41582610637892));
#32887=CARTESIAN_POINT('Ctrl Pts',(0.0105357537251741,-0.170779459512285,
3.40792887185309));
#32888=CARTESIAN_POINT('Ctrl Pts',(-0.137240406842142,-0.102184620258639,
3.40003163732725));
#32889=CARTESIAN_POINT('Ctrl Pts',(-0.160590399224686,0.059053785336183,
3.39213440280142));
#32890=CARTESIAN_POINT('Ctrl Pts',(-0.0383444372147038,0.166752301406097,
3.38423716827558));
#32891=CARTESIAN_POINT('Ctrl Pts',(0.118665713444722,0.123268302253741,
3.37633993374974));
#32892=CARTESIAN_POINT('Ctrl Pts',(0.168090056429774,-0.0319743462358346,
3.36844269922391));
#32893=CARTESIAN_POINT('Ctrl Pts',(0.065119036364785,-0.158228116942597,
3.36054546469807));
#32894=CARTESIAN_POINT('Ctrl Pts',(-0.0968908072892766,-0.141027647469737,
3.35264823017224));
#32895=CARTESIAN_POINT('Ctrl Pts',(-0.171056610272434,0.00403261331316083,
3.3447509956464));
#32896=CARTESIAN_POINT('Ctrl Pts',(-0.090137485695877,0.145436788882724,
3.33685376112057));
#32897=CARTESIAN_POINT('Ctrl Pts',(0.0725029206093111,0.154983716535553,
3.32895652659473));
#32898=CARTESIAN_POINT('Ctrl Pts',(0.16941005783654,0.0240178723428656,
3.3210592920689));
#32899=CARTESIAN_POINT('Ctrl Pts',(0.112725080116148,-0.128723277618595,
3.31316205754306));
#32900=CARTESIAN_POINT('Ctrl Pts',(-0.0461597532904643,-0.164760137971002,
3.30526482301723));
#32901=CARTESIAN_POINT('Ctrl Pts',(-0.163194803845412,-0.0514206367708408,
3.29736758849139));
#32902=CARTESIAN_POINT('Ctrl Pts',(-0.132272670563786,0.108538318164536,
3.28947035396555));
#32903=CARTESIAN_POINT('Ctrl Pts',(0.0185717358172978,0.17009325829319,
3.28157311943971));
#32904=CARTESIAN_POINT('Ctrl Pts',(0.152578463144044,0.0774366739514488,
3.27367588491388));
#32905=CARTESIAN_POINT('Ctrl Pts',(0.148253091721553,-0.0854262645973846,
3.26577865038804));
#32906=CARTESIAN_POINT('Ctrl Pts',(0.00951712983096357,-0.170839252304153,
3.25788141586221));
#32907=CARTESIAN_POINT('Ctrl Pts',(-0.137847340411707,-0.101364375544273,
3.24998418133637));
#32908=CARTESIAN_POINT('Ctrl Pts',(-0.160235378769951,0.060010409751241,
3.24208694681054));
#32909=CARTESIAN_POINT('Ctrl Pts',(-0.0373493346503772,0.166978001812321,
3.2341897122847));
#32910=CARTESIAN_POINT('Ctrl Pts',(0.119398709011011,0.122558452073145,
3.22629247775887));
#32911=CARTESIAN_POINT('Ctrl Pts',(0.16789638977649,-0.0329761760682205,
3.21839524323303));
#32912=CARTESIAN_POINT('Ctrl Pts',(0.0641742913436723,-0.158613638185999,
3.2104980087072));
#32913=CARTESIAN_POINT('Ctrl Pts',(-0.0977300972000018,-0.14044733528743,
3.20260077418136));
#32914=CARTESIAN_POINT('Ctrl Pts',(-0.17102952028482,0.00505263091922082,
3.19470353965552));
#32915=CARTESIAN_POINT('Ctrl Pts',(-0.0892685763849535,0.145971734107207,
3.18680630512969));
#32916=CARTESIAN_POINT('Ctrl Pts',(0.0734258706399851,0.15454859238706,
3.17890907060385));
#32917=CARTESIAN_POINT('Ctrl Pts',(0.169550275086044,0.0230071751049201,
3.17101183607802));
#32918=CARTESIAN_POINT('Ctrl Pts',(0.11195543952363,-0.129393220259535,
3.16311460155218));
#32919=CARTESIAN_POINT('Ctrl Pts',(-0.0471414730460515,-0.164481936415857,
3.15521736702635));
#32920=CARTESIAN_POINT('Ctrl Pts',(-0.163498546911009,-0.0504465166889647,
3.14732013250051));
#32921=CARTESIAN_POINT('Ctrl Pts',(-0.131623054589357,0.109325191006596,
3.13942289797468));
#32922=CARTESIAN_POINT('Ctrl Pts',(0.0195857499831994,0.169979481954902,
3.13152566344884));
#32923=CARTESIAN_POINT('Ctrl Pts',(0.153037540591104,0.0765254013899147,
3.123628428923));
#32924=CARTESIAN_POINT('Ctrl Pts',(0.147741019404812,-0.0863088470163307,
3.11573119439717));
#32925=CARTESIAN_POINT('Ctrl Pts',(0.00849816749472986,-0.170892969537348,
3.10783395987133));
#32926=CARTESIAN_POINT('Ctrl Pts',(-0.138449371701125,-0.100540525976471,
3.09993672534551));
#32927=CARTESIAN_POINT('Ctrl Pts',(-0.159874659831641,0.0609648999981013,
3.09203949081965));
#32928=CARTESIAN_POINT('Ctrl Pts',(-0.0363529038275426,0.167197763954447,
3.08414225629384));
#32929=CARTESIAN_POINT('Ctrl Pts',(0.120127458381323,0.121844243322797,
3.07624502176798));
#32930=CARTESIAN_POINT('Ctrl Pts',(0.167696752193779,-0.0339768331620215,
3.06834778724216));
#32931=CARTESIAN_POINT('Ctrl Pts',(0.0632272640813166,-0.158993518625298,
3.06045055271632));
#32932=CARTESIAN_POINT('Ctrl Pts',(-0.0985659115183093,-0.139862028351609,
3.05255331819049));
#32933=CARTESIAN_POINT('Ctrl Pts',(-0.170996347944273,0.0060724688375345,
3.04465608366465));
#32934=CARTESIAN_POINT('Ctrl Pts',(-0.0883964924000305,0.146501488113373,
3.03675884913881));
#32935=CARTESIAN_POINT('Ctrl Pts',(0.0743462094135637,0.154107971999816,
3.02886161461298));
#32936=CARTESIAN_POINT('Ctrl Pts',(0.16968446258935,0.0219956596587875,
3.02096438008714));
#32937=CARTESIAN_POINT('Ctrl Pts',(0.111181817440176,-0.130058561266688,
3.01306714556131));
#32938=CARTESIAN_POINT('Ctrl Pts',(-0.048121516301165,-0.16419788536074,
3.00516991103547));
#32939=CARTESIAN_POINT('Ctrl Pts',(-0.163796475449092,-0.0494706025687624,
2.99727267650963));
#32940=CARTESIAN_POINT('Ctrl Pts',(-0.13096875768114,0.110108175897699,
2.9893754419838));
#32941=CARTESIAN_POINT('Ctrl Pts',(0.020599067617639,0.169859660606483,
2.98147820745796));
#32942=CARTESIAN_POINT('Ctrl Pts',(0.153491175537256,0.0756114073420768,
2.97358097293213));
#32943=CARTESIAN_POINT('Ctrl Pts',(0.147223692948271,-0.0871883600185597,
2.96568373840629));
#32944=CARTESIAN_POINT('Ctrl Pts',(0.00747890293667656,-0.17094060927397,
2.95778650388045));
#32945=CARTESIAN_POINT('Ctrl Pts',(-0.139046479291249,-0.0997131008681262,
2.94988926935462));
#32946=CARTESIAN_POINT('Ctrl Pts',(-0.159508255242737,0.0619172221391909,
2.94199203482878));
#32947=CARTESIAN_POINT('Ctrl Pts',(-0.0353551801800353,0.167411580013796,
2.93409480030295));
#32948=CARTESIAN_POINT('Ctrl Pts',(0.120851935637802,0.121125701403006,
2.92619756577711));
#32949=CARTESIAN_POINT('Ctrl Pts',(0.167491150781951,-0.0349762819293654,
2.91830033125128));
#32950=CARTESIAN_POINT('Ctrl Pts',(0.0622779882568489,-0.159367744754771,
2.91040309672545));
#32951=CARTESIAN_POINT('Ctrl Pts',(-0.0993982205201476,-0.139271747469127,
2.9025058621996));
#32952=CARTESIAN_POINT('Ctrl Pts',(-0.170957094429947,0.0070920907826306,
2.89460862767378));
#32953=CARTESIAN_POINT('Ctrl Pts',(-0.0875212647563887,0.147026032094007,
2.88671139314793));
#32954=CARTESIAN_POINT('Ctrl Pts',(0.0752639042022573,0.153661870981,2.8788141586221));
#32955=CARTESIAN_POINT('Ctrl Pts',(0.169812615569706,0.0209833620978328,
2.87091692409627));
#32956=CARTESIAN_POINT('Ctrl Pts',(0.110404241387148,-0.130719277210608,
2.86301968957043));
#32957=CARTESIAN_POINT('Ctrl Pts',(-0.0490998482194935,-0.163907994460633,
2.8551224550446));
#32958=CARTESIAN_POINT('Ctrl Pts',(-0.164088578831389,-0.0484929299764868,
2.84722522051876));
#32959=CARTESIAN_POINT('Ctrl Pts',(-0.130309803171479,0.110887246646458,
2.83932798599293));
#32960=CARTESIAN_POINT('Ctrl Pts',(0.0216116528059362,0.16973379532663,
2.83143075146709));
#32961=CARTESIAN_POINT('Ctrl Pts',(0.153939351614839,0.0746947304359413,
2.82353351694125));
#32962=CARTESIAN_POINT('Ctrl Pts',(0.146701131201786,-0.0880647841079112,
2.81563628241542));
#32963=CARTESIAN_POINT('Ctrl Pts',(0.00645937153523989,-0.170982147149946,
2.80773904788958));
#32964=CARTESIAN_POINT('Ctrl Pts',(-0.139638640273367,-0.0988821732639446,
2.79984181336375));
#32965=CARTESIAN_POINT('Ctrl Pts',(-0.15913618125404,0.0628674262334842,
2.79194457883791));
#32966=CARTESIAN_POINT('Ctrl Pts',(-0.0343561929939461,0.167619280904103,
2.78404734431207));
#32967=CARTESIAN_POINT('Ctrl Pts',(0.121572103093823,0.120403162573872,
2.77615010978624));
#32968=CARTESIAN_POINT('Ctrl Pts',(0.167279615791685,-0.0359750846539325,
2.7682528752604));
#32969=CARTESIAN_POINT('Ctrl Pts',(0.0613264534930637,-0.159735152992013,
2.76035564073457));
#32970=CARTESIAN_POINT('Ctrl Pts',(-0.100226909682718,-0.138678726864922,
2.75245840620873));
#32971=CARTESIAN_POINT('Ctrl Pts',(-0.170911924544395,0.00811571897511738,
2.74456117168289));
#32972=CARTESIAN_POINT('Ctrl Pts',(-0.0866426101092102,0.147537153481027,
2.73666393715706));
#32973=CARTESIAN_POINT('Ctrl Pts',(0.0761783167224614,0.153226073001953,
2.72876670263122));
#32974=CARTESIAN_POINT('Ctrl Pts',(0.169935900193086,0.0199399612296831,
2.72086946810539));
#32975=CARTESIAN_POINT('Ctrl Pts',(0.109620435889599,-0.131316761419452,
2.71297223357956));
#32976=CARTESIAN_POINT('Ctrl Pts',(-0.0500715297607526,-0.163726613645121,
2.70507499905371));
#32977=CARTESIAN_POINT('Ctrl Pts',(-0.164388680888184,-0.0472783988092873,
2.69717776452789));
#32978=CARTESIAN_POINT('Ctrl Pts',(-0.141185667375647,0.0582896848558531,
2.69191294151066));
#32979=CARTESIAN_POINT('Ctrl Pts',(-0.1098796447191,0.0946377159884756,
2.68928053000205));
#32980=CARTESIAN_POINT('Ctrl Pts',(-0.035056132297315,-0.13112820202432,
3.61071946999795));
#32981=CARTESIAN_POINT('Ctrl Pts',(-0.0784331561467214,-0.119531683020372,
3.60808705848934));
#32982=CARTESIAN_POINT('Ctrl Pts',(-0.152049595447957,-0.0501363827528818,
3.60282223547212));
#32983=CARTESIAN_POINT('Ctrl Pts',(-0.125064490131564,0.100197355787414,
3.59492500094628));
#32984=CARTESIAN_POINT('Ctrl Pts',(0.015511945077094,0.15935411346322,3.58702776642045));
#32985=CARTESIAN_POINT('Ctrl Pts',(0.141921352750402,0.074201718429132,
3.57913053189461));
#32986=CARTESIAN_POINT('Ctrl Pts',(0.139714185771159,-0.078309492500346,
3.57123329736877));
#32987=CARTESIAN_POINT('Ctrl Pts',(0.0108102880423358,-0.159778753088445,
3.56333606284294));
#32988=CARTESIAN_POINT('Ctrl Pts',(-0.127880107617888,-0.0964109213300309,
3.5554388283171));
#32989=CARTESIAN_POINT('Ctrl Pts',(-0.150638153215513,0.0543778250372407,
3.54754159379127));
#32990=CARTESIAN_POINT('Ctrl Pts',(-0.0368193454873861,0.155859832308261,
3.53964435926543));
#32991=CARTESIAN_POINT('Ctrl Pts',(0.110378933082395,0.116037984046548,
3.5317471247396));
#32992=CARTESIAN_POINT('Ctrl Pts',(0.157505493964057,-0.0289889734694223,
3.52384989021376));
#32993=CARTESIAN_POINT('Ctrl Pts',(0.0618324188141689,-0.147732807425485,
3.51595265568793));
#32994=CARTESIAN_POINT('Ctrl Pts',(-0.089899452009857,-0.132538209115007,
3.50805542116209));
#32995=CARTESIAN_POINT('Ctrl Pts',(-0.160125997159357,0.00281964287334723,
3.50015818663625));
#32996=CARTESIAN_POINT('Ctrl Pts',(-0.0851775516099315,0.135621001710926,
3.49226095211042));
#32997=CARTESIAN_POINT('Ctrl Pts',(0.0669953144008998,0.145464456095352,
3.48436371758458));
#32998=CARTESIAN_POINT('Ctrl Pts',(0.15842828900316,0.0234255455897019,
3.47646648305875));
#32999=CARTESIAN_POINT('Ctrl Pts',(0.106225530800914,-0.119851632733321,
3.46856924853291));
#33000=CARTESIAN_POINT('Ctrl Pts',(-0.0422843959151,-0.154467823194868,
3.46067201400708));
#33001=CARTESIAN_POINT('Ctrl Pts',(-0.152458055071087,-0.0490389611647173,
3.45277477948124));
#33002=CARTESIAN_POINT('Ctrl Pts',(-0.124408779446231,0.100850055401476,
3.44487754495541));
#33003=CARTESIAN_POINT('Ctrl Pts',(0.0164331347266433,0.159305462375208,
3.43698031042957));
#33004=CARTESIAN_POINT('Ctrl Pts',(0.142376288572858,0.0733298756298809,
3.42908307590374));
#33005=CARTESIAN_POINT('Ctrl Pts',(0.139236933413632,-0.0791287214708696,
3.4211858413779));
#33006=CARTESIAN_POINT('Ctrl Pts',(0.00986130080885162,-0.159846904754402,
3.41328860685207));
#33007=CARTESIAN_POINT('Ctrl Pts',(-0.128454875683531,-0.0956432073768941,
3.40539137232623));
#33008=CARTESIAN_POINT('Ctrl Pts',(-0.150310103584168,0.0552734200411303,
3.3974941378004));
#33009=CARTESIAN_POINT('Ctrl Pts',(-0.0358897938945578,0.15607754771305,
3.38959690327456));
#33010=CARTESIAN_POINT('Ctrl Pts',(0.111069252993198,0.115377204178194,
3.38169966874872));
#33011=CARTESIAN_POINT('Ctrl Pts',(0.157329665505583,-0.0299274883053255,
3.37380243422289));
#33012=CARTESIAN_POINT('Ctrl Pts',(0.060950400201679,-0.14809904429152,
3.36590519969705));
#33013=CARTESIAN_POINT('Ctrl Pts',(-0.090688281181918,-0.131999673714922,
3.35800796517121));
#33014=CARTESIAN_POINT('Ctrl Pts',(-0.160106313533927,0.00377446302981049,
3.35011073064538));
#33015=CARTESIAN_POINT('Ctrl Pts',(-0.0843672777275282,0.13612656116089,
3.34221349611954));
#33016=CARTESIAN_POINT('Ctrl Pts',(0.0678616004415848,0.145062336221761,
3.33431626159371));
#33017=CARTESIAN_POINT('Ctrl Pts',(0.158565166190183,0.0224803531042752,
3.32641902706787));
#33018=CARTESIAN_POINT('Ctrl Pts',(0.105508913052052,-0.12048297585632,
3.31852179254204));
#33019=CARTESIAN_POINT('Ctrl Pts',(-0.0432048075850524,-0.154212913876088,
3.3106245580162));
#33020=CARTESIAN_POINT('Ctrl Pts',(-0.152747785601314,-0.0481289122930385,
3.30272732349037));
#33021=CARTESIAN_POINT('Ctrl Pts',(-0.123805152174632,0.101590169306055,
3.29483008896453));
#33022=CARTESIAN_POINT('Ctrl Pts',(0.0173828544415669,0.159204631138919,
3.28693285443869));
#33023=CARTESIAN_POINT('Ctrl Pts',(0.142811056642351,0.0724795164533502,
3.27903561991286));
#33024=CARTESIAN_POINT('Ctrl Pts',(0.13876257659813,-0.0799576484175498,
3.27113838538702));
#33025=CARTESIAN_POINT('Ctrl Pts',(0.00890788476535658,-0.159902869873006,
3.26324115086119));
#33026=CARTESIAN_POINT('Ctrl Pts',(-0.129022956018037,-0.0948754711449903,
3.25534391633535));
#33027=CARTESIAN_POINT('Ctrl Pts',(-0.149977809987643,0.0561688055412144,
3.24744668180951));
#33028=CARTESIAN_POINT('Ctrl Pts',(-0.0349583934481866,0.156288799765492,
3.23954944728368));
#33029=CARTESIAN_POINT('Ctrl Pts',(0.111755325386239,0.11471279550439,3.23165221275784));
#33030=CARTESIAN_POINT('Ctrl Pts',(0.157148396545194,-0.0308651853694504,
3.22375497823201));
#33031=CARTESIAN_POINT('Ctrl Pts',(0.0600661336286481,-0.148459886149497,
3.21585774370617));
#33032=CARTESIAN_POINT('Ctrl Pts',(-0.0914738434199304,-0.131456510582787,
3.20796050918034));
#33033=CARTESIAN_POINT('Ctrl Pts',(-0.160080957728948,0.00472918356581254,
3.2000632746545));
#33034=CARTESIAN_POINT('Ctrl Pts',(-0.0835539921938928,0.136627261529605,
3.19216604012867));
#33035=CARTESIAN_POINT('Ctrl Pts',(0.0687254672442293,0.144655066819931,
3.18426880560283));
#33036=CARTESIAN_POINT('Ctrl Pts',(0.158696407344068,0.0215343562871474,
3.176371571077));
#33037=CARTESIAN_POINT('Ctrl Pts',(0.104788541487236,-0.121110031696776,
3.16847433655116));
#33038=CARTESIAN_POINT('Ctrl Pts',(-0.0441236819316221,-0.15395252156887,
3.16057710202533));
#33039=CARTESIAN_POINT('Ctrl Pts',(-0.153032084363091,-0.0472171511222767,
3.15267986749949));
#33040=CARTESIAN_POINT('Ctrl Pts',(-0.123197121776316,0.102326669987095,
3.14478263297366));
#33041=CARTESIAN_POINT('Ctrl Pts',(0.0183319558514166,0.159098138264651,
3.13688539844782));
#33042=CARTESIAN_POINT('Ctrl Pts',(0.143240745957241,0.0716265795792973,
3.12898816392198));
#33043=CARTESIAN_POINT('Ctrl Pts',(0.138283284913549,-0.0807837317665782,
3.12109092939615));
#33044=CARTESIAN_POINT('Ctrl Pts',(0.00795415194541781,-0.159953148363655,
3.11319369487031));
#33045=CARTESIAN_POINT('Ctrl Pts',(-0.12958644789495,-0.0941043608266151,
3.10529646034448));
#33046=CARTESIAN_POINT('Ctrl Pts',(-0.149640182699562,0.0570621934932236,
3.09739922581864));
#33047=CARTESIAN_POINT('Ctrl Pts',(-0.0340257497726133,0.156494493695554,
3.08950199129281));
#33048=CARTESIAN_POINT('Ctrl Pts',(0.112437423406217,0.114044307277423,
3.08160475676696));
#33049=CARTESIAN_POINT('Ctrl Pts',(0.156961538888189,-0.0318017847685902,
3.07370752224114));
#33050=CARTESIAN_POINT('Ctrl Pts',(0.0591797309134862,-0.148815448303003,
3.06581028771529));
#33051=CARTESIAN_POINT('Ctrl Pts',(-0.0922561525577649,-0.130908672439433,
3.05791305318946));
#33052=CARTESIAN_POINT('Ctrl Pts',(-0.160049908936692,0.00568373591689232,
3.05001581866362));
#33053=CARTESIAN_POINT('Ctrl Pts',(-0.0827377352150154,0.137123102999116,
3.04211858413779));
#33054=CARTESIAN_POINT('Ctrl Pts',(0.0695868899510474,0.144242653024537,
3.03422134961195));
#33055=CARTESIAN_POINT('Ctrl Pts',(0.15882200474976,0.0205875936399453,
3.02632411508612));
#33056=CARTESIAN_POINT('Ctrl Pts',(0.104064443309136,-0.121732780479934,
3.01842688056028));
#33057=CARTESIAN_POINT('Ctrl Pts',(-0.0450409870999527,-0.153686654221109,
3.01052964603445));
#33058=CARTESIAN_POINT('Ctrl Pts',(-0.153310940817998,-0.0463037107596828,
3.00263241150861));
#33059=CARTESIAN_POINT('Ctrl Pts',(-0.122584710097139,0.103059531606811,
2.99473517698278));
#33060=CARTESIAN_POINT('Ctrl Pts',(0.019280405318705,0.158985987355384,
2.98683794245694));
#33061=CARTESIAN_POINT('Ctrl Pts',(0.143665341176349,0.0707710954366019,
2.97894070793111));
#33062=CARTESIAN_POINT('Ctrl Pts',(0.13779907543624,-0.0816069421895357,
2.97104347340527));
#33063=CARTESIAN_POINT('Ctrl Pts',(0.00700013625057968,-0.159997738412506,
2.96314623887943));
#33064=CARTESIAN_POINT('Ctrl Pts',(-0.130145331266283,-0.0933299038581796,
2.9552490043536));
#33065=CARTESIAN_POINT('Ctrl Pts',(-0.149297233731393,0.0579535521321195,
2.94735176982776));
#33066=CARTESIAN_POINT('Ctrl Pts',(-0.0330918960333533,0.156694622185077,
2.93945453530193));
#33067=CARTESIAN_POINT('Ctrl Pts',(0.113115522794421,0.113371763271587,
2.93155730077609));
#33068=CARTESIAN_POINT('Ctrl Pts',(0.156769099180348,-0.0327372531930529,
2.92366006625026));
#33069=CARTESIAN_POINT('Ctrl Pts',(0.0582912235793329,-0.14916571811089,
2.91576283172442));
#33070=CARTESIAN_POINT('Ctrl Pts',(-0.0930351807741731,-0.130356178759748,
2.90786559719858));
#33071=CARTESIAN_POINT('Ctrl Pts',(-0.160013168260831,0.00663808612041647,
2.89996836267275));
#33072=CARTESIAN_POINT('Ctrl Pts',(-0.0819185358207136,0.137614067966164,
2.89207112814691));
#33073=CARTESIAN_POINT('Ctrl Pts',(0.0704458379293395,0.143825109443657,
2.88417389362108));
#33074=CARTESIAN_POINT('Ctrl Pts',(0.158941953936293,0.0196400989454948,
2.87627665909524));
#33075=CARTESIAN_POINT('Ctrl Pts',(0.103336644277317,-0.122351200276197,
2.86837942456941));
#33076=CARTESIAN_POINT('Ctrl Pts',(-0.0459566904838012,-0.153415320869716,
2.86048219004357));
#33077=CARTESIAN_POINT('Ctrl Pts',(-0.15358434501814,-0.0453886244947142,
2.85258495551773));
#33078=CARTESIAN_POINT('Ctrl Pts',(-0.12196793897581,0.103788729650472,
2.8446877209919));
#33079=CARTESIAN_POINT('Ctrl Pts',(0.0202281692278525,0.158868179420765,
2.83679048646607));
#33080=CARTESIAN_POINT('Ctrl Pts',(0.144084826979801,0.0699131001804741,
2.82889325194023));
#33081=CARTESIAN_POINT('Ctrl Pts',(0.137309965809371,-0.0824272614383206,
2.8209960174144));
#33082=CARTESIAN_POINT('Ctrl Pts',(0.00604587079450571,-0.160036617215166,
2.81309878288855));
#33083=CARTESIAN_POINT('Ctrl Pts',(-0.13069958468984,-0.0925521686083858,
2.80520154836272));
#33084=CARTESIAN_POINT('Ctrl Pts',(-0.148948978293633,0.0588429283123199,
2.79730431383689));
#33085=CARTESIAN_POINT('Ctrl Pts',(-0.0321568596417307,0.156889026971959,
2.78940707931105));
#33086=CARTESIAN_POINT('Ctrl Pts',(0.113789588276761,0.11269547822108,2.78150984478522));
#33087=CARTESIAN_POINT('Ctrl Pts',(0.156571105735832,-0.0336721169315741,
2.77361261025938));
#33088=CARTESIAN_POINT('Ctrl Pts',(0.0574006019132872,-0.149509606478216,
2.76571537573355));
#33089=CARTESIAN_POINT('Ctrl Pts',(-0.0938108208776064,-0.129801120743354,
2.75781814120771));
#33090=CARTESIAN_POINT('Ctrl Pts',(-0.159970889953977,0.00759618610887905,
2.74992090668187));
#33091=CARTESIAN_POINT('Ctrl Pts',(-0.0810961288046671,0.138092469595389,
2.74202367215604));
#33092=CARTESIAN_POINT('Ctrl Pts',(0.0713017137556289,0.143417209346961,
2.7341264376302));
#33093=CARTESIAN_POINT('Ctrl Pts',(0.15905734641679,0.0186634920416663,
2.72622920310437));
#33094=CARTESIAN_POINT('Ctrl Pts',(0.102603014582794,-0.122910436156766,
2.71833196857853));
#33095=CARTESIAN_POINT('Ctrl Pts',(-0.046866169218661,-0.153245551261449,
2.7104347340527));
#33096=CARTESIAN_POINT('Ctrl Pts',(-0.153865235852588,-0.044251842305808,
2.70253749952686));
#33097=CARTESIAN_POINT('Ctrl Pts',(-0.132147577876941,0.0545582339347279,
2.69727267650964));
#33098=CARTESIAN_POINT('Ctrl Pts',(-0.102845629995673,0.0885794229410579,
2.69464026500102));
#33099=CARTESIAN_POINT('Ctrl Pts',(-0.0326585063531101,-0.122159831625555,
3.61607920499693));
#33100=CARTESIAN_POINT('Ctrl Pts',(-0.0730688059534842,-0.111356443894347,
3.61344679348832));
#33101=CARTESIAN_POINT('Ctrl Pts',(-0.14165032915811,-0.0467073595218706,
3.60818197047109));
#33102=CARTESIAN_POINT('Ctrl Pts',(-0.116510840695994,0.0933444668908538,
3.60028473594526));
#33103=CARTESIAN_POINT('Ctrl Pts',(0.0144510225073566,0.148455262628371,
3.59238750141942));
#33104=CARTESIAN_POINT('Ctrl Pts',(0.132214796576289,0.0691267728047427,
3.58449026689359));
#33105=CARTESIAN_POINT('Ctrl Pts',(0.130158586375956,-0.0729536001473631,
3.57659303236775));
#33106=CARTESIAN_POINT('Ctrl Pts',(0.0100709301789295,-0.148850859489444,
3.56869579784192));
#33107=CARTESIAN_POINT('Ctrl Pts',(-0.119133887094416,-0.0898170014895561,
3.56079856331608));
#33108=CARTESIAN_POINT('Ctrl Pts',(-0.140335420978156,0.0506587129859461,
3.55290132879025));
#33109=CARTESIAN_POINT('Ctrl Pts',(-0.0343011264996069,0.145199969022934,
3.54500409426441));
#33110=CARTESIAN_POINT('Ctrl Pts',(0.102829686308464,0.108101692652402,
3.53710685973857));
#33111=CARTESIAN_POINT('Ctrl Pts',(0.146733077444168,-0.0270063042377832,
3.52920962521274));
#33112=CARTESIAN_POINT('Ctrl Pts',(0.0576034579497911,-0.137628783145524,
3.5213123906869));
#33113=CARTESIAN_POINT('Ctrl Pts',(-0.0837508770136032,-0.123473402818708,
3.51341515616107));
#33114=CARTESIAN_POINT('Ctrl Pts',(-0.149174354180752,0.00262679647348802,
3.50551792163523));
#33115=CARTESIAN_POINT('Ctrl Pts',(-0.0793519258428967,0.126345351176423,
3.4976206871094));
#33116=CARTESIAN_POINT('Ctrl Pts',(0.062413242922351,0.135515573231267,
3.48972345258356));
#33117=CARTESIAN_POINT('Ctrl Pts',(0.147592758922763,0.0218233809416831,
3.48182621805773));
#33118=CARTESIAN_POINT('Ctrl Pts',(0.0989603514472664,-0.111654510995544,
3.47392898353189));
#33119=CARTESIAN_POINT('Ctrl Pts',(-0.0393924007622622,-0.143903164855042,
3.46603174900606));
#33120=CARTESIAN_POINT('Ctrl Pts',(-0.14203085263069,-0.0456849948866295,
3.45813451448022));
#33121=CARTESIAN_POINT('Ctrl Pts',(-0.115899976628015,0.0939525258264977,
3.45023727995438));
#33122=CARTESIAN_POINT('Ctrl Pts',(0.0153092083952656,0.148409938978475,
3.44234004542855));
#33123=CARTESIAN_POINT('Ctrl Pts',(0.132638617559218,0.0683145587431124,
3.43444281090271));
#33124=CARTESIAN_POINT('Ctrl Pts',(0.129713975173039,-0.0737167988457132,
3.42654557637688));
#33125=CARTESIAN_POINT('Ctrl Pts',(0.00918684789252914,-0.148914349996519,
3.41864834185104));
#33126=CARTESIAN_POINT('Ctrl Pts',(-0.11966934452492,-0.0891017944951492,
3.4107511073252));
#33127=CARTESIAN_POINT('Ctrl Pts',(-0.140029807943649,0.0514930547460776,
3.40285387279937));
#33128=CARTESIAN_POINT('Ctrl Pts',(-0.0334351505744119,0.145402794020004,
3.39495663827353));
#33129=CARTESIAN_POINT('Ctrl Pts',(0.103472792541674,0.107486106102647,
3.3870594037477));
#33130=CARTESIAN_POINT('Ctrl Pts',(0.146569274581392,-0.0278806303748164,
3.37916216922186));
#33131=CARTESIAN_POINT('Ctrl Pts',(0.0567817640385731,-0.137969971640442,
3.37126493469603));
#33132=CARTESIAN_POINT('Ctrl Pts',(-0.0844857550745595,-0.122971699960107,
3.36336770017019));
#33133=CARTESIAN_POINT('Ctrl Pts',(-0.14915601679542,0.00351631274646034,
3.35547046564435));
#33134=CARTESIAN_POINT('Ctrl Pts',(-0.0785970697591793,0.126816333439056,
3.34757323111852));
#33135=CARTESIAN_POINT('Ctrl Pts',(0.0632202802738586,0.13514095590797,
3.33967599659268));
#33136=CARTESIAN_POINT('Ctrl Pts',(0.147720274543826,0.0209428338656845,
3.33177876206685));
#33137=CARTESIAN_POINT('Ctrl Pts',(0.0982927459879567,-0.112242674094044,
3.32388152754101));
#33138=CARTESIAN_POINT('Ctrl Pts',(-0.0402498618796406,-0.143665689781173,
3.31598429301518));
#33139=CARTESIAN_POINT('Ctrl Pts',(-0.142300767357216,-0.0448371878152361,
3.30808705848934));
#33140=CARTESIAN_POINT('Ctrl Pts',(-0.115337633785478,0.0946420204475735,
3.30018982396351));
#33141=CARTESIAN_POINT('Ctrl Pts',(0.0161939730658361,0.148316003984649,
3.29229258943767));
#33142=CARTESIAN_POINT('Ctrl Pts',(0.133043650140658,0.0675223589552513,
3.28439535491184));
#33143=CARTESIAN_POINT('Ctrl Pts',(0.129272061474707,-0.0744890322377149,
3.276498120386));
#33144=CARTESIAN_POINT('Ctrl Pts',(0.00829863969974947,-0.148966487441859,
3.26860088586017));
#33145=CARTESIAN_POINT('Ctrl Pts',(-0.120198571624367,-0.0883865667457073,
3.26070365133432));
#33146=CARTESIAN_POINT('Ctrl Pts',(-0.139720241205335,0.0523272013311878,
3.2528064168085));
#33147=CARTESIAN_POINT('Ctrl Pts',(-0.032567452245996,0.145599597718663,
3.24490918228265));
#33148=CARTESIAN_POINT('Ctrl Pts',(0.104111941761468,0.106867138935634,
3.23701194775683));
#33149=CARTESIAN_POINT('Ctrl Pts',(0.146400403313899,-0.0287541946706802,
3.22911471323098));
#33150=CARTESIAN_POINT('Ctrl Pts',(0.0559579759136239,-0.138306134112995,
3.22121747870515));
#33151=CARTESIAN_POINT('Ctrl Pts',(-0.085217589639859,-0.122465685878144,
3.21332024417931));
#33152=CARTESIAN_POINT('Ctrl Pts',(-0.149132395173076,0.00440573621240416,
3.20542300965348));
#33153=CARTESIAN_POINT('Ctrl Pts',(-0.077839408002832,0.127282788952003,
3.19752577512764));
#33154=CARTESIAN_POINT('Ctrl Pts',(0.0640250638484733,0.134761541252801,
3.18962854060181));
#33155=CARTESIAN_POINT('Ctrl Pts',(0.147842539602093,0.0200615374693747,
3.18173130607597));
#33156=CARTESIAN_POINT('Ctrl Pts',(0.0976216434508421,-0.112826843134018,
3.17383407155013));
#33157=CARTESIAN_POINT('Ctrl Pts',(-0.0411058908171925,-0.143423106721883,
3.1659368370243));
#33158=CARTESIAN_POINT('Ctrl Pts',(-0.142565621815174,-0.0439877855555886,
3.15803960249846));
#33159=CARTESIAN_POINT('Ctrl Pts',(-0.114771188963274,0.0953281489675947,
3.15014236797263));
#33160=CARTESIAN_POINT('Ctrl Pts',(0.0170781617196339,0.148216794574399,
3.14224513344679));
#33161=CARTESIAN_POINT('Ctrl Pts',(0.133443951323378,0.0667277577686799,
3.13434789892096));
#33162=CARTESIAN_POINT('Ctrl Pts',(0.128825550422286,-0.0752586165168258,
3.12645066439512));
#33163=CARTESIAN_POINT('Ctrl Pts',(0.00741013639610572,-0.149013327189962,
3.11855342986929));
#33164=CARTESIAN_POINT('Ctrl Pts',(-0.120723524088775,-0.0876681956767594,
3.11065619534345));
#33165=CARTESIAN_POINT('Ctrl Pts',(-0.139405705567482,0.0531594869883457,
3.10275896081762));
#33166=CARTESIAN_POINT('Ctrl Pts',(-0.0316985957176838,0.145791223436661,
3.09486172629178));
#33167=CARTESIAN_POINT('Ctrl Pts',(0.104747388431111,0.106244371232049,
3.08696449176594));
#33168=CARTESIAN_POINT('Ctrl Pts',(0.1462263255826,-0.0296267363751589,
3.07906725724011));
#33169=CARTESIAN_POINT('Ctrl Pts',(0.0551321977456556,-0.138637377980708,
3.07117002271428));
#33170=CARTESIAN_POINT('Ctrl Pts',(-0.0859463935972202,-0.121955316527256,
3.06327278818844));
#33171=CARTESIAN_POINT('Ctrl Pts',(-0.149103469929111,0.00529500299625034,
3.0553755536626));
#33172=CARTESIAN_POINT('Ctrl Pts',(-0.0770789780300003,0.127744717884859,
3.04747831913677));
#33173=CARTESIAN_POINT('Ctrl Pts',(0.064827570488531,0.134377334049259,
3.03958108461093));
#33174=CARTESIAN_POINT('Ctrl Pts',(0.147959546910171,0.0191795276211033,
3.0316838500851));
#33175=CARTESIAN_POINT('Ctrl Pts',(0.096947069178096,-0.11340699969318,
3.02378661555926));
#33176=CARTESIAN_POINT('Ctrl Pts',(-0.0419604578987403,-0.143175423081478,
3.01588938103343));
#33177=CARTESIAN_POINT('Ctrl Pts',(-0.142825406186904,-0.0431368189506033,
3.00799214650759));
#33178=CARTESIAN_POINT('Ctrl Pts',(-0.114200662513138,0.0960108873159227,
3.00009491198175));
#33179=CARTESIAN_POINT('Ctrl Pts',(0.0179617430197712,0.148112314104285,
2.99219767745592));
#33180=CARTESIAN_POINT('Ctrl Pts',(0.133839506815442,0.065930783531127,
2.98430044293008));
#33181=CARTESIAN_POINT('Ctrl Pts',(0.128374457924208,-0.0760255243605117,
2.97640320840425));
#33182=CARTESIAN_POINT('Ctrl Pts',(0.00652136956448273,-0.149054867551042,
2.96850597387841));
#33183=CARTESIAN_POINT('Ctrl Pts',(-0.121244183241318,-0.0869467068482327,
2.96060873935258));
#33184=CARTESIAN_POINT('Ctrl Pts',(-0.139086212220049,0.0539898821250478,
2.95271150482674));
#33185=CARTESIAN_POINT('Ctrl Pts',(-0.0308286118866713,0.145977664356358,
2.9448142703009));
#33186=CARTESIAN_POINT('Ctrl Pts',(0.10537910995104,0.105617825140169,2.93691703577507));
#33187=CARTESIAN_POINT('Ctrl Pts',(0.146047047578745,-0.0304982244567401,
2.92901980124923));
#33188=CARTESIAN_POINT('Ctrl Pts',(0.0543044589018171,-0.138963691467009,
2.9211225667234));
#33189=CARTESIAN_POINT('Ctrl Pts',(-0.0866721410281989,-0.121440610050369,
2.91322533219756));
#33190=CARTESIAN_POINT('Ctrl Pts',(-0.149069242091714,0.0061840814582022,
2.90532809767173));
#33191=CARTESIAN_POINT('Ctrl Pts',(-0.0763158068850386,0.128202103838321,
2.89743086314589));
#33192=CARTESIAN_POINT('Ctrl Pts',(0.0656277716564218,0.133988347906315,
2.88953362862006));
#33193=CARTESIAN_POINT('Ctrl Pts',(0.14807129230288,0.0182968357931569,
2.88163639409422));
#33194=CARTESIAN_POINT('Ctrl Pts',(0.0962690471674858,-0.113983123341786,
2.87373915956838));
#33195=CARTESIAN_POINT('Ctrl Pts',(-0.0428135327481091,-0.142922647278798,
2.86584192504255));
#33196=CARTESIAN_POINT('Ctrl Pts',(-0.14308011120489,-0.0422843190129418,
2.85794469051671));
#33197=CARTESIAN_POINT('Ctrl Pts',(-0.113626074780142,0.0966902126544859,
2.85004745599088));
#33198=CARTESIAN_POINT('Ctrl Pts',(0.0188446856497688,0.1480025635149,2.84215022146504));
#33199=CARTESIAN_POINT('Ctrl Pts',(0.134230302344763,0.0651314699250072,
2.8342529869392));
#33200=CARTESIAN_POINT('Ctrl Pts',(0.127918800416957,-0.0767897387687304,
2.82635575241337));
#33201=CARTESIAN_POINT('Ctrl Pts',(0.00563237005377145,-0.149091087280386,
2.81845851788753));
#33202=CARTESIAN_POINT('Ctrl Pts',(-0.121760529106313,-0.0862221639528271,
2.8105612833617));
#33203=CARTESIAN_POINT('Ctrl Pts',(-0.138761775333226,0.0548184303911556,
2.80266404883586));
#33204=CARTESIAN_POINT('Ctrl Pts',(-0.0299575262895149,0.146158773039815,
2.79476681431003));
#33205=CARTESIAN_POINT('Ctrl Pts',(0.106007073459698,0.104987793868287,
2.7868695797842));
#33206=CARTESIAN_POINT('Ctrl Pts',(0.145862595679981,-0.0313691492092156,
2.77897234525835));
#33207=CARTESIAN_POINT('Ctrl Pts',(0.0534747503335104,-0.139284059964419,
2.77107511073252));
#33208=CARTESIAN_POINT('Ctrl Pts',(-0.0873947320724949,-0.120923514621786,
2.76317787620668));
#33209=CARTESIAN_POINT('Ctrl Pts',(-0.149029855363559,0.00707665324264049,
2.75528064168085));
#33210=CARTESIAN_POINT('Ctrl Pts',(-0.0755496475001239,0.128647785709752,
2.74738340715502));
#33211=CARTESIAN_POINT('Ctrl Pts',(0.0664251107887961,0.133608345691969,
2.73948617262918));
#33212=CARTESIAN_POINT('Ctrl Pts',(0.148178792640495,0.0173870228536497,
2.73158893810334));
#33213=CARTESIAN_POINT('Ctrl Pts',(0.0955855932759896,-0.114504110894079,
2.72369170357751));
#33214=CARTESIAN_POINT('Ctrl Pts',(-0.0436608086765693,-0.142764488877777,
2.71579446905167));
#33215=CARTESIAN_POINT('Ctrl Pts',(-0.143341790816993,-0.0412252858023288,
2.70789723452584));
#33216=CARTESIAN_POINT('Ctrl Pts',(-0.123109488378236,0.0508267830136028,
2.70263241150861));
#33217=CARTESIAN_POINT('Ctrl Pts',(-0.0958116152722464,0.0825211298936403,
2.7));
#33218=CARTESIAN_POINT('Ctrl Pts',(-0.126320239448181,8.84447983197572E-5,
3.55565803263806));
#33219=CARTESIAN_POINT('Ctrl Pts',(-0.126416389705588,0.0147241557759941,
3.55473913135546));
#33220=CARTESIAN_POINT('Ctrl Pts',(-0.124064907197002,0.029329993953288,
3.55382023007285));
#33221=CARTESIAN_POINT('Ctrl Pts',(-0.119129449584441,0.0430029699128602,
3.55290132879025));
#33222=CARTESIAN_POINT('Ctrl Pts',(-0.104990656151973,0.0821724649982754,
3.55026891728164));
#33223=CARTESIAN_POINT('Ctrl Pts',(-0.0696458913257897,0.113686217010605,
3.54763650577302));
#33224=CARTESIAN_POINT('Ctrl Pts',(-0.0291183734446862,0.123260046955014,
3.54500409426441));
#33225=CARTESIAN_POINT('Ctrl Pts',(0.011409144436417,0.132833876899423,
3.5423716827558));
#33226=CARTESIAN_POINT('Ctrl Pts',(0.0571194153724406,0.120467784775912,
3.53973927124719));
#33227=CARTESIAN_POINT('Ctrl Pts',(0.0872917826964029,0.0917667392324598,
3.53710685973857));
#33228=CARTESIAN_POINT('Ctrl Pts',(0.117464150020365,0.0630656936890069,
3.53447444822996));
#33229=CARTESIAN_POINT('Ctrl Pts',(0.132098613732267,0.0180296947256118,
3.53184203672135));
#33230=CARTESIAN_POINT('Ctrl Pts',(0.124560909005821,-0.0229253845740426,
3.52920962521274));
#33231=CARTESIAN_POINT('Ctrl Pts',(0.117023204279375,-0.0638804638736969,
3.52657721370413));
#33232=CARTESIAN_POINT('Ctrl Pts',(0.0873133311145834,-0.100754623509611,
3.52394480219552));
#33233=CARTESIAN_POINT('Ctrl Pts',(0.048899338704955,-0.116832473273098,
3.5213123906869));
#33234=CARTESIAN_POINT('Ctrl Pts',(0.0104853462953266,-0.132910323036586,
3.51867997917829));
#33235=CARTESIAN_POINT('Ctrl Pts',(-0.0366327653591382,-0.128191862927647,
3.51604756766968));
#33236=CARTESIAN_POINT('Ctrl Pts',(-0.0710957340475621,-0.104815932991145,
3.51341515616107));
#33237=CARTESIAN_POINT('Ctrl Pts',(-0.104947268304411,-0.0818547336764444,
3.51082944832006));
#33238=CARTESIAN_POINT('Ctrl Pts',(-0.126588725667586,-0.0408922251827605,
3.50824374047906));
#33239=CARTESIAN_POINT('Ctrl Pts',(-0.12665116202208,1.34725138570783E-5,
3.50565803263806));
#33240=CARTESIAN_POINT('Ctrl Pts',(-0.0398513841857247,-0.149064942821851,
3.6));
#33241=CARTESIAN_POINT('Ctrl Pts',(-0.0498814435786606,-0.145400000402268,
3.6));
#33242=CARTESIAN_POINT('Ctrl Pts',(-0.059436150936811,-0.14063603073288,
3.6));
#33243=CARTESIAN_POINT('Ctrl Pts',(-0.0684043669488933,-0.134923276476459,
3.6));
#33244=CARTESIAN_POINT('Ctrl Pts',(-0.0756266237179617,-0.130322698385691,
3.6));
#33245=CARTESIAN_POINT('Ctrl Pts',(-0.0824683814027756,-0.125105404214097,
3.6));
#33246=CARTESIAN_POINT('Ctrl Pts',(-0.0888542192956036,-0.119334036703677,
3.6));
#33247=CARTESIAN_POINT('Ctrl Pts',(-0.091539386939335,-0.116907246428204,
3.6));
#33248=CARTESIAN_POINT('Ctrl Pts',(-0.0941378270474737,-0.114387469535812,
3.6));
#33249=CARTESIAN_POINT('Ctrl Pts',(-0.0966394276056281,-0.111785621852247,
3.6));
#33250=CARTESIAN_POINT('Ctrl Pts',(-0.103848676908048,-0.104287474901247,
3.6));
#33251=CARTESIAN_POINT('Ctrl Pts',(-0.110272002565724,-0.0960958678941195,
3.6));
#33252=CARTESIAN_POINT('Ctrl Pts',(-0.115776223647425,-0.0873309061633839,
3.6));
#33253=CARTESIAN_POINT('Ctrl Pts',(-0.118162872674894,-0.0835303888731155,
3.6));
#33254=CARTESIAN_POINT('Ctrl Pts',(-0.120376124201495,-0.0796218141710604,
3.6));
#33255=CARTESIAN_POINT('Ctrl Pts',(-0.122402049312502,-0.0756142631648066,
3.6));
#33256=CARTESIAN_POINT('Ctrl Pts',(-0.123825086107396,-0.0727993059344893,
3.6));
#33257=CARTESIAN_POINT('Ctrl Pts',(-0.125154691418473,-0.0699368314187636,
3.6));
#33258=CARTESIAN_POINT('Ctrl Pts',(-0.126381872197889,-0.0670411886576404,
3.6));
#33259=CARTESIAN_POINT('Ctrl Pts',(-0.129549149387792,-0.0595677149679855,
3.6));
#33260=CARTESIAN_POINT('Ctrl Pts',(-0.132046086846552,-0.0518539539453467,
3.6));
#33261=CARTESIAN_POINT('Ctrl Pts',(-0.133799060139059,-0.0439576297154888,
3.6));
#33262=CARTESIAN_POINT('Ctrl Pts',(-0.135388531616607,-0.0367978046374413,
3.6));
#33263=CARTESIAN_POINT('Ctrl Pts',(-0.136365840160023,-0.0294873792206846,
3.6));
#33264=CARTESIAN_POINT('Ctrl Pts',(-0.13674259160829,-0.0221011370783161,
3.6));
#33265=CARTESIAN_POINT('Ctrl Pts',(-0.136915659814306,-0.0187081211187088,
3.6));
#33266=CARTESIAN_POINT('Ctrl Pts',(-0.136961265679344,-0.0153067045798101,
3.6));
#33267=CARTESIAN_POINT('Ctrl Pts',(-0.136881936917631,-0.0119112232715221,
3.6));
#33268=CARTESIAN_POINT('Ctrl Pts',(-0.136684990383263,-0.0034813894794369,
3.6));
#33269=CARTESIAN_POINT('Ctrl Pts',(-0.135720534319688,0.00492632812693493,
3.6));
#33270=CARTESIAN_POINT('Ctrl Pts',(-0.134014244604164,0.0131981027910972,
3.6));
#33271=CARTESIAN_POINT('Ctrl Pts',(-0.133007067351581,0.0180807104774909,
3.6));
#33272=CARTESIAN_POINT('Ctrl Pts',(-0.131740913976379,0.0229158302155836,
3.6));
#33273=CARTESIAN_POINT('Ctrl Pts',(-0.130217237780107,0.0276776331326924,
3.6));
#33274=CARTESIAN_POINT('Ctrl Pts',(-0.129150755329031,0.0310106111361586,
3.6));
#33275=CARTESIAN_POINT('Ctrl Pts',(-0.127957851528495,0.0343071390648417,
3.6));
#33276=CARTESIAN_POINT('Ctrl Pts',(-0.126644351454204,0.0375455932808108,
3.6));
#33277=CARTESIAN_POINT('Ctrl Pts',(-0.12454778430103,0.0427147111736446,
3.6));
#33278=CARTESIAN_POINT('Ctrl Pts',(-0.122141614879321,0.0477447959908898,
3.6));
#33279=CARTESIAN_POINT('Ctrl Pts',(-0.11942949850221,0.0525991124010946,
3.6));
#33280=CARTESIAN_POINT('Ctrl Pts',(-0.116867678035268,0.0571844197417489,
3.6));
#33281=CARTESIAN_POINT('Ctrl Pts',(-0.11402973916396,0.0616160698651957,
3.6));
#33282=CARTESIAN_POINT('Ctrl Pts',(-0.110933547566151,0.0658375038383711,
3.6));
#33283=CARTESIAN_POINT('Ctrl Pts',(-0.107383747559623,0.0706774001665366,
3.6));
#33284=CARTESIAN_POINT('Ctrl Pts',(-0.103491800365401,0.0752476578095535,
3.6));
#33285=CARTESIAN_POINT('Ctrl Pts',(-0.0992594032733973,0.0794964740507377,
3.6));
#33286=CARTESIAN_POINT('Ctrl Pts',(-0.0981916513129811,0.080568368245057,
3.6));
#33287=CARTESIAN_POINT('Ctrl Pts',(-0.0971022039419119,0.081619760070457,
3.6));
#33288=CARTESIAN_POINT('Ctrl Pts',(-0.0959917963302726,0.0826503396631628,
3.6));
#33289=CARTESIAN_POINT('Origin',(0.,0.,3.1));
#33290=CARTESIAN_POINT('Origin',(0.,0.,2.6));
#33291=CARTESIAN_POINT('Origin',(4.61329551933804E-18,0.,1.7));
#33292=CARTESIAN_POINT('Ctrl Pts',(0.163512932725146,-0.0319230454628286,
1.7));
#33293=CARTESIAN_POINT('Ctrl Pts',(0.162868713265022,-0.0402193660776135,
1.7));
#33294=CARTESIAN_POINT('Ctrl Pts',(0.161556142957416,-0.0484298106643142,
1.7));
#33295=CARTESIAN_POINT('Ctrl Pts',(0.159633648446255,-0.0565030284772356,
1.7));
#33296=CARTESIAN_POINT('Ctrl Pts',(0.15857220935963,-0.0609603774536462,
1.7));
#33297=CARTESIAN_POINT('Ctrl Pts',(0.15732455882578,-0.0653759608776499,
1.7));
#33298=CARTESIAN_POINT('Ctrl Pts',(0.155898537051345,-0.0697413060244838,
1.7));
#33299=CARTESIAN_POINT('Ctrl Pts',(0.154359565759251,-0.0744524128122629,
1.7));
#33300=CARTESIAN_POINT('Ctrl Pts',(0.152615240924071,-0.0790971028454583,
1.7));
#33301=CARTESIAN_POINT('Ctrl Pts',(0.150679159438777,-0.0836586618069671,
1.7));
#33302=CARTESIAN_POINT('Ctrl Pts',(0.147458757270998,-0.0912461804520635,
1.7));
#33303=CARTESIAN_POINT('Ctrl Pts',(0.143706663154478,-0.098609365081655,
1.7));
#33304=CARTESIAN_POINT('Ctrl Pts',(0.139465780840256,-0.105699927668597,
1.7));
#33305=CARTESIAN_POINT('Ctrl Pts',(0.137613322919106,-0.108797153164702,
1.7));
#33306=CARTESIAN_POINT('Ctrl Pts',(0.135667748856481,-0.111841429389798,
1.7));
#33307=CARTESIAN_POINT('Ctrl Pts',(0.133638504154441,-0.114820282936825,
1.7));
#33308=CARTESIAN_POINT('Ctrl Pts',(0.126764362615545,-0.124911259587064,
1.7));
#33309=CARTESIAN_POINT('Ctrl Pts',(0.118918297697151,-0.134279562536914,
1.7));
#33310=CARTESIAN_POINT('Ctrl Pts',(0.110233695412878,-0.142776634038112,
1.7));
#33311=CARTESIAN_POINT('Ctrl Pts',(0.1060042704444,-0.146914731004415,1.7));
#33312=CARTESIAN_POINT('Ctrl Pts',(0.101575189643516,-0.150846009251356,
1.7));
#33313=CARTESIAN_POINT('Ctrl Pts',(0.0969579219100265,-0.154551255269456,
1.7));
#33314=CARTESIAN_POINT('Ctrl Pts',(0.0930558717128837,-0.157682556460965,
1.7));
#33315=CARTESIAN_POINT('Ctrl Pts',(0.089014879864356,-0.160654885938173,
1.7));
#33316=CARTESIAN_POINT('Ctrl Pts',(0.084867234382875,-0.163439189909414,
1.7));
#33317=CARTESIAN_POINT('Ctrl Pts',(0.0797924645177416,-0.166845870145637,
1.7));
#33318=CARTESIAN_POINT('Ctrl Pts',(0.0745525511585738,-0.169976381556328,
1.7));
#33319=CARTESIAN_POINT('Ctrl Pts',(0.069162704388918,-0.172812601917057,
1.7));
#33320=CARTESIAN_POINT('Ctrl Pts',(0.0615917910053332,-0.176796533113158,
1.7));
#33321=CARTESIAN_POINT('Ctrl Pts',(0.0537253644412386,-0.180200415745643,
1.7));
#33322=CARTESIAN_POINT('Ctrl Pts',(0.0456302879589726,-0.183039981733068,
1.7));
#33323=CARTESIAN_POINT('Ctrl Pts',(0.039725979220554,-0.185111076961087,
1.7));
#33324=CARTESIAN_POINT('Ctrl Pts',(0.0336998028892366,-0.186881755092485,
1.7));
#33325=CARTESIAN_POINT('Ctrl Pts',(0.027575472779275,-0.188354488495274,
1.7));
#33326=CARTESIAN_POINT('Ctrl Pts',(0.0240503901388611,-0.189202174178265,
1.7));
#33327=CARTESIAN_POINT('Ctrl Pts',(0.0204971902089821,-0.189949869388286,
1.7));
#33328=CARTESIAN_POINT('Ctrl Pts',(0.0169287682122467,-0.190597281499825,
1.7));
#33329=CARTESIAN_POINT('Ctrl Pts',(0.00540716645046445,-0.192687624102725,
1.7));
#33330=CARTESIAN_POINT('Ctrl Pts',(-0.00629626416002409,-0.193741044106324,
1.7));
#33331=CARTESIAN_POINT('Ctrl Pts',(-0.0180243092057446,-0.193790924616578,
1.7));
#33332=CARTESIAN_POINT('Ctrl Pts',(-0.0246815057039127,-0.193819238317361,
1.7));
#33333=CARTESIAN_POINT('Ctrl Pts',(-0.0313470218059255,-0.19352361589825,
1.7));
#33334=CARTESIAN_POINT('Ctrl Pts',(-0.0379937712674718,-0.192905366089908,
1.7));
#33335=CARTESIAN_POINT('Ctrl Pts',(-0.0421040672802865,-0.192523045417697,
1.7));
#33336=CARTESIAN_POINT('Ctrl Pts',(-0.0462092418665425,-0.192016959216387,
1.7));
#33337=CARTESIAN_POINT('Ctrl Pts',(-0.0502964475671879,-0.191387744025229,
1.7));
#33338=CARTESIAN_POINT('Ctrl Pts',(-0.0635557644152557,-0.189346505047739,
1.7));
#33339=CARTESIAN_POINT('Ctrl Pts',(-0.076538642829352,-0.186027878905466,
1.7));
#33340=CARTESIAN_POINT('Ctrl Pts',(-0.0890304894083597,-0.181464562959599,
1.7));
#33341=CARTESIAN_POINT('Ctrl Pts',(-0.0993708472336289,-0.177687193500922,
1.7));
#33342=CARTESIAN_POINT('Ctrl Pts',(-0.109375752092602,-0.173056097632409,
1.7));
#33343=CARTESIAN_POINT('Ctrl Pts',(-0.118921685270779,-0.167562801749516,
1.7));
#33344=CARTESIAN_POINT('Ctrl Pts',(-0.120076087508369,-0.166898490263086,
1.7));
#33345=CARTESIAN_POINT('Ctrl Pts',(-0.121223766120909,-0.16622153952215,
1.7));
#33346=CARTESIAN_POINT('Ctrl Pts',(-0.122364641233049,-0.165532117868825,
1.7));
#33347=CARTESIAN_POINT('Ctrl Pts',(-0.188262750966375,-0.0823232180103074,
1.7));
#33348=CARTESIAN_POINT('Ctrl Pts',(-0.190918693248964,-0.0742705707004131,
1.7));
#33349=CARTESIAN_POINT('Ctrl Pts',(-0.193028471001937,-0.0660604959755095,
1.7));
#33350=CARTESIAN_POINT('Ctrl Pts',(-0.194604369739905,-0.0577442961437627,
1.7));
#33351=CARTESIAN_POINT('Ctrl Pts',(-0.195791431603972,-0.0514800334494749,
1.7));
#33352=CARTESIAN_POINT('Ctrl Pts',(-0.196675380086104,-0.0451554970342283,
1.7));
#33353=CARTESIAN_POINT('Ctrl Pts',(-0.197258353741452,-0.0387928833243269,
1.7));
#33354=CARTESIAN_POINT('Ctrl Pts',(-0.197694864529353,-0.0340287752070089,
1.7));
#33355=CARTESIAN_POINT('Ctrl Pts',(-0.197962173616876,-0.0292446940334784,
1.7));
#33356=CARTESIAN_POINT('Ctrl Pts',(-0.198061149421263,-0.0244622127102265,
1.7));
#33357=CARTESIAN_POINT('Ctrl Pts',(-0.198268317226716,-0.0144519261913088,
1.7));
#33358=CARTESIAN_POINT('Ctrl Pts',(-0.197740578304783,-0.00443368324017007,
1.7));
#33359=CARTESIAN_POINT('Ctrl Pts',(-0.196485470149517,0.00550410801291526,
1.7));
#33360=CARTESIAN_POINT('Ctrl Pts',(-0.19583094903621,0.0106865252950324,
1.7));
#33361=CARTESIAN_POINT('Ctrl Pts',(-0.194977340636945,0.0158499464463904,
1.7));
#33362=CARTESIAN_POINT('Ctrl Pts',(-0.193930228257619,0.0209568152791792,
1.7));
#33363=CARTESIAN_POINT('Ctrl Pts',(-0.191365358848382,0.0334659326431063,
1.7));
#33364=CARTESIAN_POINT('Ctrl Pts',(-0.187640262305008,0.0456682931313192,
1.7));
#33365=CARTESIAN_POINT('Ctrl Pts',(-0.18276823303275,0.0573755743540122,
1.7));
#33366=CARTESIAN_POINT('Ctrl Pts',(-0.180530605205125,0.0627524998168591,
1.7));
#33367=CARTESIAN_POINT('Ctrl Pts',(-0.178050427357818,0.0680246443278264,
1.7));
#33368=CARTESIAN_POINT('Ctrl Pts',(-0.175326059031915,0.0731713030262629,
1.7));
#33369=CARTESIAN_POINT('Ctrl Pts',(-0.173546095954943,0.0765338668785476,
1.7));
#33370=CARTESIAN_POINT('Ctrl Pts',(-0.171660782837765,0.0798445731517242,
1.7));
#33371=CARTESIAN_POINT('Ctrl Pts',(-0.169672721187811,0.0830915804684565,
1.7));
#33372=CARTESIAN_POINT('Ctrl Pts',(-0.165401890376176,0.0900669269795776,
1.7));
#33373=CARTESIAN_POINT('Ctrl Pts',(-0.160674569826176,0.0967219627994757,
1.7));
#33374=CARTESIAN_POINT('Ctrl Pts',(-0.15549277623518,0.103004446710986,
1.7));
#33375=CARTESIAN_POINT('Ctrl Pts',(-0.149788864011586,0.109919955047648,
1.7));
#33376=CARTESIAN_POINT('Ctrl Pts',(-0.143534087392955,0.116384355174537,
1.7));
#33377=CARTESIAN_POINT('Ctrl Pts',(-0.1368007840805,0.122364607652698,1.7));
#33378=CARTESIAN_POINT('Ctrl Pts',(-0.132573081040691,0.126119485519849,
1.7));
#33379=CARTESIAN_POINT('Ctrl Pts',(-0.128156557788873,0.129683253321797,
1.7));
#33380=CARTESIAN_POINT('Ctrl Pts',(-0.123568264594465,0.133044997940945,
1.7));
#33381=CARTESIAN_POINT('Ctrl Pts',(-0.120777285576228,0.135089888774893,
1.7));
#33382=CARTESIAN_POINT('Ctrl Pts',(-0.117925900172203,0.137057490795076,
1.7));
#33383=CARTESIAN_POINT('Ctrl Pts',(-0.115025210475747,0.138941543144738,
1.7));
#33384=CARTESIAN_POINT('Ctrl Pts',(-0.106405133477763,0.144540444792911,
1.7));
#33385=CARTESIAN_POINT('Ctrl Pts',(-0.0973325886051703,0.149416450333531,
1.7));
#33386=CARTESIAN_POINT('Ctrl Pts',(-0.0879171639429846,0.15351829690281,
1.7));
#33387=CARTESIAN_POINT('Ctrl Pts',(-0.0791136675584941,0.157353555825057,
1.7));
#33388=CARTESIAN_POINT('Ctrl Pts',(-0.0700097444331976,0.160511945106675,
1.7));
#33389=CARTESIAN_POINT('Ctrl Pts',(-0.0606944403481407,0.162929898574301,
1.7));
#33390=CARTESIAN_POINT('Ctrl Pts',(-0.0571572012739495,0.163848052121106,
1.7));
#33391=CARTESIAN_POINT('Ctrl Pts',(-0.0535976091548405,0.16465702786045,
1.7));
#33392=CARTESIAN_POINT('Ctrl Pts',(-0.0500249348171965,0.165353504526832,
1.7));
#33393=CARTESIAN_POINT('Ctrl Pts',(-0.0389427731093366,0.16751392171383,
1.7));
#33394=CARTESIAN_POINT('Ctrl Pts',(-0.0277208597802445,0.168598940439913,
1.7));
#33395=CARTESIAN_POINT('Ctrl Pts',(-0.016510036378599,0.168511954471149,
1.7));
#33396=CARTESIAN_POINT('Ctrl Pts',(-0.0103145529256217,0.168463883057408,
1.7));
#33397=CARTESIAN_POINT('Ctrl Pts',(-0.00412256070196868,0.168057036314866,
1.7));
#33398=CARTESIAN_POINT('Ctrl Pts',(0.00203815650313415,0.16726854038896,
1.7));
#33399=CARTESIAN_POINT('Ctrl Pts',(0.00311390584534565,0.167130857722252,
1.7));
#33400=CARTESIAN_POINT('Ctrl Pts',(0.00418869523159273,0.166981526327298,
1.7));
#33401=CARTESIAN_POINT('Ctrl Pts',(0.00526237188779194,0.16682061735739,
1.7));
#33402=CARTESIAN_POINT('Origin',(0.,0.,0.645407471946233));
#33403=CARTESIAN_POINT('Ctrl Pts',(0.205654271051376,0.000148184871923513,
0.820407471946232));
#33404=CARTESIAN_POINT('Ctrl Pts',(0.20573642152142,0.00997667026911825,
0.820941869468311));
#33405=CARTESIAN_POINT('Ctrl Pts',(0.200629007389055,0.0878566204334846,
0.825180863342659));
#33406=CARTESIAN_POINT('Ctrl Pts',(0.101090873180113,0.220844643128561,
0.833124453569275));
#33407=CARTESIAN_POINT('Ctrl Pts',(-0.130696704329673,0.204681987270635,
0.844238242626078));
#33408=CARTESIAN_POINT('Ctrl Pts',(-0.242858579725743,0.00121498249237738,
0.855352031682883));
#33409=CARTESIAN_POINT('Ctrl Pts',(-0.132727951496213,-0.203386773400678,
0.866465820739686));
#33410=CARTESIAN_POINT('Ctrl Pts',(0.0988894015246068,-0.221814471640749,
0.877579609796491));
#33411=CARTESIAN_POINT('Ctrl Pts',(0.200212227802606,-0.0892608439806378,
0.885560160198673));
#33412=CARTESIAN_POINT('Ctrl Pts',(0.205725385245381,-0.0106740336596208,
0.889836114248587));
#33413=CARTESIAN_POINT('Ctrl Pts',(0.205635165348036,-0.000160487501855345,
0.890407471946233));
#33414=CARTESIAN_POINT('Ctrl Pts',(0.205269394176581,-0.000252214316689755,
0.814592528053767));
#33415=CARTESIAN_POINT('Ctrl Pts',(0.204912576919524,0.0467765744646069,
0.817137544740381));
#33416=CARTESIAN_POINT('Ctrl Pts',(0.165648098003252,0.162976258711784,
0.823387157779263));
#33417=CARTESIAN_POINT('Ctrl Pts',(-0.0272119409517698,0.241262826763902,
0.833341367170412));
#33418=CARTESIAN_POINT('Ctrl Pts',(-0.217470922739143,0.108102090643486,
0.844455156227217));
#33419=CARTESIAN_POINT('Ctrl Pts',(-0.208759451561279,-0.124141896006793,
0.85556894528402));
#33420=CARTESIAN_POINT('Ctrl Pts',(-0.00892472216375234,-0.242686445659381,
0.866682734340826));
#33421=CARTESIAN_POINT('Ctrl Pts',(0.172122246966409,-0.152544606240875,
0.87635726193074));
#33422=CARTESIAN_POINT('Ctrl Pts',(0.20498850808804,-0.0417917950361515,
0.882327193168388));
#33423=CARTESIAN_POINT('Ctrl Pts',(0.205205445749305,0.000116004416325009,
0.884592528053768));
#33424=CARTESIAN_POINT('Ctrl Pts',(-0.126907087985236,0.107935865304854,
0.8));
#33425=CARTESIAN_POINT('Ctrl Pts',(-0.162798331100657,0.0657362393039544,
0.803704596352268));
#33426=CARTESIAN_POINT('Ctrl Pts',(-0.188554427056889,-0.0565517713871986,
0.811113789056805));
#33427=CARTESIAN_POINT('Ctrl Pts',(-0.0544936724634594,-0.189356862721456,
0.822227578113607));
#33428=CARTESIAN_POINT('Ctrl Pts',(0.12941144825895,-0.14834225030535,0.833341367170414));
#33429=CARTESIAN_POINT('Ctrl Pts',(0.194879695227305,0.0282018585329969,
0.844455156227216));
#33430=CARTESIAN_POINT('Ctrl Pts',(0.0819649080024663,0.179061771725117,
0.855568945284021));
#33431=CARTESIAN_POINT('Ctrl Pts',(-0.105969441252334,0.165957021921342,
0.866682734340825));
#33432=CARTESIAN_POINT('Ctrl Pts',(-0.196910764727139,0.000985112949166876,
0.877796523397629));
#33433=CARTESIAN_POINT('Ctrl Pts',(-0.107616385055452,-0.164906857031527,
0.888910312454434));
#33434=CARTESIAN_POINT('Ctrl Pts',(0.0801799454629491,-0.179848112789142,
0.900024101511237));
#33435=CARTESIAN_POINT('Ctrl Pts',(0.194586948216313,-0.0301773643334041,
0.911137890568042));
#33436=CARTESIAN_POINT('Ctrl Pts',(0.13088616131906,0.147117686303235,0.922251679624846));
#33437=CARTESIAN_POINT('Ctrl Pts',(-0.0526161354638876,0.18975288262963,
0.93336546868165));
#33438=CARTESIAN_POINT('Ctrl Pts',(-0.187958327447607,0.0587058278606146,
0.944479257738454));
#33439=CARTESIAN_POINT('Ctrl Pts',(-0.151260109468812,-0.126075710016806,
0.955593046795258));
#33440=CARTESIAN_POINT('Ctrl Pts',(0.0238881910101356,-0.195458525846084,
0.966706835852062));
#33441=CARTESIAN_POINT('Ctrl Pts',(0.177171365146215,-0.0859360381031547,
0.977820624908868));
#33442=CARTESIAN_POINT('Ctrl Pts',(0.168287576475019,0.102244733060238,
0.98893441396567));
#33443=CARTESIAN_POINT('Ctrl Pts',(0.00536826212740452,0.196839712751384,
1.00004820302248));
#33444=CARTESIAN_POINT('Ctrl Pts',(-0.162464684252001,0.111265085550637,
1.01116199207928));
#33445=CARTESIAN_POINT('Ctrl Pts',(-0.181591862229106,-0.076151743861926,
1.02227578113608));
#33446=CARTESIAN_POINT('Ctrl Pts',(-0.0345059495415616,-0.193866014541413,
1.03338957019289));
#33447=CARTESIAN_POINT('Ctrl Pts',(0.144163650203206,-0.134132525587662,
1.04450335924969));
#33448=CARTESIAN_POINT('Ctrl Pts',(0.190878625928487,0.0483739862822188,
1.0556171483065));
#33449=CARTESIAN_POINT('Ctrl Pts',(0.062880230662697,0.186603239345861,
1.0667309373633));
#33450=CARTESIAN_POINT('Ctrl Pts',(-0.122673152855754,0.154032431506053,
1.07784472642011));
#33451=CARTESIAN_POINT('Ctrl Pts',(-0.195942408348395,-0.019526007891641,
1.08895851547691));
#33452=CARTESIAN_POINT('Ctrl Pts',(-0.0898633553462809,-0.175212070745787,
1.10007230453371));
#33453=CARTESIAN_POINT('Ctrl Pts',(0.0984686459264395,-0.170524538248248,
1.11118609359052));
#33454=CARTESIAN_POINT('Ctrl Pts',(0.196671178871044,-0.00975396199037572,
1.12229988264732));
#33455=CARTESIAN_POINT('Ctrl Pts',(0.114858351392768,0.159944526283292,
1.13341367170412));
#33456=CARTESIAN_POINT('Ctrl Pts',(-0.0720856276979479,0.183243975761544,
1.14452746076093));
#33457=CARTESIAN_POINT('Ctrl Pts',(-0.193048814249935,0.0388181360941049,
1.15564124981773));
#33458=CARTESIAN_POINT('Ctrl Pts',(-0.13731223179659,-0.141138383766243,
1.16675503887454));
#33459=CARTESIAN_POINT('Ctrl Pts',(0.0441077936468435,-0.191909340348063,
1.17786882793134));
#33460=CARTESIAN_POINT('Ctrl Pts',(0.185155455348894,-0.0670235013089116,
1.18898261698815));
#33461=CARTESIAN_POINT('Ctrl Pts',(0.156728228964436,0.119209708576257,
1.20009640604495));
#33462=CARTESIAN_POINT('Ctrl Pts',(-0.0151541228101832,0.196328920271653,
1.21121019510176));
#33463=CARTESIAN_POINT('Ctrl Pts',(-0.173165734117196,0.0937460447209521,
1.22232398415856));
#33464=CARTESIAN_POINT('Ctrl Pts',(-0.172676785153749,-0.0946436487152594,
1.23343777321536));
#33465=CARTESIAN_POINT('Ctrl Pts',(-0.0141348164511399,-0.196404937150434,
1.24455156227217));
#33466=CARTESIAN_POINT('Ctrl Pts',(0.157344910048918,-0.118394559228326,
1.25566535132897));
#33467=CARTESIAN_POINT('Ctrl Pts',(0.184805055968556,0.0679837014410847,
1.26677914038578));
#33468=CARTESIAN_POINT('Ctrl Pts',(0.0431110383282961,0.192135709193865,
1.27789292944258));
#33469=CARTESIAN_POINT('Ctrl Pts',(-0.138043001606285,0.140423723354349,
1.28900671849938));
#33470=CARTESIAN_POINT('Ctrl Pts',(-0.192844716656512,-0.0398196889847226,
1.30012050755619));
#33471=CARTESIAN_POINT('Ctrl Pts',(-0.0711334755432105,-0.183615688410121,
1.31123429661299));
#33472=CARTESIAN_POINT('Ctrl Pts',(0.115687042443292,-0.159346165890141,
1.32234808566979));
#33473=CARTESIAN_POINT('Ctrl Pts',(0.196617898501115,0.0107747093774004,
1.3334618747266));
#33474=CARTESIAN_POINT('Ctrl Pts',(0.0975821622623196,0.171033370958511,
1.3445756637834));
#33475=CARTESIAN_POINT('Ctrl Pts',(-0.0907716337523168,0.174743248450528,
1.35568945284021));
#33476=CARTESIAN_POINT('Ctrl Pts',(-0.196041123972824,0.0185086489133565,
1.36680324189701));
#33477=CARTESIAN_POINT('Ctrl Pts',(-0.121871950164007,-0.1546671268781,
1.37791703095382));
#33478=CARTESIAN_POINT('Ctrl Pts',(0.0638480017529153,-0.186274327390575,
1.38903082001062));
#33479=CARTESIAN_POINT('Ctrl Pts',(0.191127153577756,-0.0473825235535316,
1.40014460906743));
#33480=CARTESIAN_POINT('Ctrl Pts',(0.143465454207459,0.134879041457197,
1.41125839812423));
#33481=CARTESIAN_POINT('Ctrl Pts',(-0.0355118024153517,0.193684290169161,
1.42237218718103));
#33482=CARTESIAN_POINT('Ctrl Pts',(-0.181984703541769,0.0752081115995363,
1.43348597623784));
#33483=CARTESIAN_POINT('Ctrl Pts',(-0.16188494169705,-0.112106904510744,
1.44459976529464));
#33484=CARTESIAN_POINT('Ctrl Pts',(0.00638994323583646,-0.196809199398823,
1.45571355435144));
#33485=CARTESIAN_POINT('Ctrl Pts',(0.168816040557079,-0.101369802386164,
1.46682734340825));
#33486=CARTESIAN_POINT('Ctrl Pts',(0.17672290164568,0.0868545248928826,
1.47794113246505));
#33487=CARTESIAN_POINT('Ctrl Pts',(0.0228732863137639,0.195579919524334,
1.48905492152186));
#33488=CARTESIAN_POINT('Ctrl Pts',(-0.15191250667306,0.125288797732896,
1.50016871057866));
#33489=CARTESIAN_POINT('Ctrl Pts',(-0.187651060854054,-0.0596805852186566,
1.51128249963547));
#33490=CARTESIAN_POINT('Ctrl Pts',(-0.0516304683294577,-0.190023644566662,
1.52239628869227));
#33491=CARTESIAN_POINT('Ctrl Pts',(0.131648072412201,-0.146435920677088,
1.53351007774908));
#33492=CARTESIAN_POINT('Ctrl Pts',(0.194427649007747,0.0311862882363455,
1.54462386680588));
#33493=CARTESIAN_POINT('Ctrl Pts',(0.0792453752737409,0.180263283819487,
1.55573765586268));
#33494=CARTESIAN_POINT('Ctrl Pts',(-0.108471054243311,0.164343347185408,
1.56685144491949));
#33495=CARTESIAN_POINT('Ctrl Pts',(-0.196902764500876,-0.00200210229874768,
1.57796523397629));
#33496=CARTESIAN_POINT('Ctrl Pts',(-0.105107013422145,-0.16651465373019,
1.5890790230331));
#33497=CARTESIAN_POINT('Ctrl Pts',(0.0828941340502818,-0.178615126425815,
1.6001928120899));
#33498=CARTESIAN_POINT('Ctrl Pts',(0.195021809584276,-0.0272258612485208,
1.61130660114671));
#33499=CARTESIAN_POINT('Ctrl Pts',(0.128642913099457,0.149081079408297,
1.62242039020351));
#33500=CARTESIAN_POINT('Ctrl Pts',(-0.0554825813599488,0.188937135031884,
1.63353417926031));
#33501=CARTESIAN_POINT('Ctrl Pts',(-0.188827531603801,0.0558478560140352,
1.64464796831712));
#33502=CARTESIAN_POINT('Ctrl Pts',(-0.149330198326453,-0.128342305854753,
1.65576175737392));
#33503=CARTESIAN_POINT('Ctrl Pts',(0.0268386909069323,-0.195092411199392,
1.66687554643073));
#33504=CARTESIAN_POINT('Ctrl Pts',(0.178464943022445,-0.0832088009083063,
1.67798933548753));
#33505=CARTESIAN_POINT('Ctrl Pts',(0.166695798680381,0.104715122443915,
1.68910312454433));
#33506=CARTESIAN_POINT('Ctrl Pts',(0.00243441762381693,0.197027042329472,
1.70021691360114));
#33507=CARTESIAN_POINT('Ctrl Pts',(-0.164232046005026,0.108529764925501,
1.71133070265794));
#33508=CARTESIAN_POINT('Ctrl Pts',(-0.174839538171076,-0.0159901738299179,
1.71873989536248));
#33509=CARTESIAN_POINT('Ctrl Pts',(-0.152644235605294,-0.0667480137268189,
1.72244449171475));
#33510=CARTESIAN_POINT('Ctrl Pts',(-0.136778062465881,0.116331236980977,
0.792518502761751));
#33511=CARTESIAN_POINT('Ctrl Pts',(-0.175460966397852,0.0708492771249652,
0.796223099114019));
#33512=CARTESIAN_POINT('Ctrl Pts',(-0.203220400149799,-0.0609504310764289,
0.803632291818556));
#33513=CARTESIAN_POINT('Ctrl Pts',(-0.0587322509288797,-0.204085250153022,
0.814746080875359));
#33514=CARTESIAN_POINT('Ctrl Pts',(0.139477214667647,-0.159880475556692,
0.825859869932165));
#33515=CARTESIAN_POINT('Ctrl Pts',(0.210037654715023,0.0303954304627091,
0.836973658988967));
#33516=CARTESIAN_POINT('Ctrl Pts',(0.0883402297283485,0.192989395526265,
0.848087448045772));
#33517=CARTESIAN_POINT('Ctrl Pts',(-0.114211862278114,0.178865343704439,
0.859201237102576));
#33518=CARTESIAN_POINT('Ctrl Pts',(-0.212226703060007,0.00106173613023704,
0.87031502615938));
#33519=CARTESIAN_POINT('Ctrl Pts',(-0.115986907202372,-0.177733495821244,
0.881428815216186));
#33520=CARTESIAN_POINT('Ctrl Pts',(0.0864164308168349,-0.193836899073011,
0.892542604272987));
#33521=CARTESIAN_POINT('Ctrl Pts',(0.209722137515851,-0.0325245933019137,
0.903656393329794));
#33522=CARTESIAN_POINT('Ctrl Pts',(0.141066632550109,0.158560663604232,
0.914770182386597));
#33523=CARTESIAN_POINT('Ctrl Pts',(-0.0567086770128242,0.204512072930204,
0.925883971443401));
#33524=CARTESIAN_POINT('Ctrl Pts',(-0.20257793524978,0.0632720324586165,
0.936997760500206));
#33525=CARTESIAN_POINT('Ctrl Pts',(-0.163025289051846,-0.135882018994204,
0.948111549557009));
#33526=CARTESIAN_POINT('Ctrl Pts',(0.025746241081202,-0.210661507423248,
0.959225338613814));
#33527=CARTESIAN_POINT('Ctrl Pts',(0.190951951020682,-0.0926202387459321,
0.970339127670618));
#33528=CARTESIAN_POINT('Ctrl Pts',(0.181377171383915,0.110197442139303,
0.981452916727422));
#33529=CARTESIAN_POINT('Ctrl Pts',(0.00578581152757031,0.212150124582537,
0.992566705784226));
#33530=CARTESIAN_POINT('Ctrl Pts',(-0.175101368126144,0.119919407681051,
1.00368049484103));
#33531=CARTESIAN_POINT('Ctrl Pts',(-0.195716279284241,-0.0820749112141317,
1.01479428389783));
#33532=CARTESIAN_POINT('Ctrl Pts',(-0.0371898606828745,-0.208945128817718,
1.02590807295464));
#33533=CARTESIAN_POINT('Ctrl Pts',(0.15537685929014,-0.144565502642925,
1.03702186201144));
#33534=CARTESIAN_POINT('Ctrl Pts',(0.205725377795173,0.0521365687486478,
1.04813565106825));
#33535=CARTESIAN_POINT('Ctrl Pts',(0.0677711249544383,0.201117446888019,
1.05924944012505));
#33536=CARTESIAN_POINT('Ctrl Pts',(-0.132214807152008,0.166013245381199,
1.07036322918185));
#33537=CARTESIAN_POINT('Ctrl Pts',(-0.211183026844882,-0.0210447625070621,
1.08147701823866));
#33538=CARTESIAN_POINT('Ctrl Pts',(-0.0968530270931527,-0.188840260522183,
1.09259080729546));
#33539=CARTESIAN_POINT('Ctrl Pts',(0.106127646747548,-0.183788126532363,
1.10370459635227));
#33540=CARTESIAN_POINT('Ctrl Pts',(0.211968481949499,-0.0105126360047333,
1.11481838540907));
#33541=CARTESIAN_POINT('Ctrl Pts',(0.123792161737694,0.172385189467092,
1.12593217446588));
#33542=CARTESIAN_POINT('Ctrl Pts',(-0.0776925280115889,0.197496896045118,
1.13704596352268));
#33543=CARTESIAN_POINT('Ctrl Pts',(-0.208064365778478,0.0418374539025449,
1.14815975257949));
#33544=CARTESIAN_POINT('Ctrl Pts',(-0.147992529938032,-0.152116284264268,
1.15927354163629));
#33545=CARTESIAN_POINT('Ctrl Pts',(0.0475385469041886,-0.206836262328918,
1.17038733069309));
#33546=CARTESIAN_POINT('Ctrl Pts',(0.199557052641187,-0.0722366638006762,
1.1815011197499));
#33547=CARTESIAN_POINT('Ctrl Pts',(0.168918724964821,0.12848197232356,1.1926149088067));
#33548=CARTESIAN_POINT('Ctrl Pts',(-0.0163328273404871,0.211599602095504,
1.2037286978635));
#33549=CARTESIAN_POINT('Ctrl Pts',(-0.186634757554183,0.101037716366665,
1.21484248692031));
#33550=CARTESIAN_POINT('Ctrl Pts',(-0.18610777759643,-0.102005136998184,
1.22595627597711));
#33551=CARTESIAN_POINT('Ctrl Pts',(-0.0152342381989151,-0.211681531651681,
1.23707006503392));
#33552=CARTESIAN_POINT('Ctrl Pts',(0.169583372190078,-0.127603419752538,
1.24818385409072));
#33553=CARTESIAN_POINT('Ctrl Pts',(0.199179398807247,0.0732715493672994,
1.25929764314753));
#33554=CARTESIAN_POINT('Ctrl Pts',(0.046464262848129,0.207080238395369,
1.27041143220433));
#33555=CARTESIAN_POINT('Ctrl Pts',(-0.148780139836465,0.151346036770516,
1.28152522126114));
#33556=CARTESIAN_POINT('Ctrl Pts',(-0.207844393247192,-0.0429169086911673,
1.29263901031794));
#33557=CARTESIAN_POINT('Ctrl Pts',(-0.0766663164030391,-0.197897520917011,
1.30375279937474));
#33558=CARTESIAN_POINT('Ctrl Pts',(0.124685309300001,-0.171740287936918,
1.31486658843155));
#33559=CARTESIAN_POINT('Ctrl Pts',(0.211911057373125,0.0116127782590458,
1.32598037748835));
#33560=CARTESIAN_POINT('Ctrl Pts',(0.105172211397869,0.184336536816879,
1.33709416654516));
#33561=CARTESIAN_POINT('Ctrl Pts',(-0.0978319524040202,0.188334972707259,
1.34820795560196));
#33562=CARTESIAN_POINT('Ctrl Pts',(-0.211289420680394,0.0199482722156909,
1.35932174465877));
#33563=CARTESIAN_POINT('Ctrl Pts',(-0.131351286023602,-0.166697308065347,
1.37043553371557));
#33564=CARTESIAN_POINT('Ctrl Pts',(0.068814170356646,-0.200762951794954,
1.38154932277237));
#33565=CARTESIAN_POINT('Ctrl Pts',(0.205993236201476,-0.0510679889459757,
1.39266311182918));
#33566=CARTESIAN_POINT('Ctrl Pts',(0.154624356833139,0.14537008334725,1.40377690088598));
#33567=CARTESIAN_POINT('Ctrl Pts',(-0.0382739499121438,0.208749269721634,
1.41489068994279));
#33568=CARTESIAN_POINT('Ctrl Pts',(-0.196139676231217,0.0810578821846344,
1.42600447899959));
#33569=CARTESIAN_POINT('Ctrl Pts',(-0.174476532550337,-0.120826704256352,
1.43711826805639));
#33570=CARTESIAN_POINT('Ctrl Pts',(0.00688696012917997,-0.212117237867469,
1.4482320571132));
#33571=CARTESIAN_POINT('Ctrl Pts',(0.181946739990165,-0.109254458384087,
1.45934584617));
#33572=CARTESIAN_POINT('Ctrl Pts',(0.190468605530186,0.0936101664599312,
1.47045963522681));
#33573=CARTESIAN_POINT('Ctrl Pts',(0.0246523959685209,0.210792343236835,
1.48157342428361));
#33574=CARTESIAN_POINT('Ctrl Pts',(-0.163728430436396,0.135033899797455,
1.49268721334042));
#33575=CARTESIAN_POINT('Ctrl Pts',(-0.202246769118763,-0.0643226075283309,
1.50380100239722));
#33576=CARTESIAN_POINT('Ctrl Pts',(-0.0556463435921781,-0.204803895031906,
1.51491479145403));
#33577=CARTESIAN_POINT('Ctrl Pts',(0.141887805935659,-0.157825869489257,
1.52602858051082));
#33578=CARTESIAN_POINT('Ctrl Pts',(0.209550447837631,0.0336119924283981,
1.53714236956763));
#33579=CARTESIAN_POINT('Ctrl Pts',(0.0854091687186523,0.194284362567952,
1.54825615862443));
#33580=CARTESIAN_POINT('Ctrl Pts',(-0.116908053510435,0.177126155552421,
1.55936994768124));
#33581=CARTESIAN_POINT('Ctrl Pts',(-0.212218080567246,-0.00215782804277307,
1.57048373673804));
#33582=CARTESIAN_POINT('Ctrl Pts',(-0.113282353851889,-0.179466348735714,
1.58159752579485));
#33583=CARTESIAN_POINT('Ctrl Pts',(0.089341732011876,-0.192508009658716,
1.59271131485165));
#33584=CARTESIAN_POINT('Ctrl Pts',(0.210190822884773,-0.0293435190237031,
1.60382510390846));
#33585=CARTESIAN_POINT('Ctrl Pts',(0.138648901988495,0.160676771609172,
1.61493889296526));
#33586=CARTESIAN_POINT('Ctrl Pts',(-0.0597980782594448,0.203632875576831,
1.62605268202207));
#33587=CARTESIAN_POINT('Ctrl Pts',(-0.203514747072184,0.0601917643824736,
1.63716647107887));
#33588=CARTESIAN_POINT('Ctrl Pts',(-0.160945267273914,-0.13832491317789,
1.64828026013567));
#33589=CARTESIAN_POINT('Ctrl Pts',(0.0289262341422404,-0.210266915972054,
1.65939404919248));
#33590=CARTESIAN_POINT('Ctrl Pts',(0.19234614482316,-0.0896808740081667,
1.67050783824928));
#33591=CARTESIAN_POINT('Ctrl Pts',(0.179661583341645,0.112859981157414,
1.68162162730609));
#33592=CARTESIAN_POINT('Ctrl Pts',(0.00262376933475311,0.212352024863603,
1.69273541636289));
#33593=CARTESIAN_POINT('Ctrl Pts',(-0.177006197242412,0.116971330774799,
1.7038492054197));
#33594=CARTESIAN_POINT('Ctrl Pts',(-0.188438751949388,-0.0172339073385976,
1.71125839812423));
#33595=CARTESIAN_POINT('Ctrl Pts',(-0.164517074058987,-0.0719397484879835,
1.7149629944765));
#33596=CARTESIAN_POINT('Ctrl Pts',(-0.146649036946525,0.124726608657099,
0.785037005523502));
#33597=CARTESIAN_POINT('Ctrl Pts',(-0.188123601695047,0.0759623149459762,
0.78874160187577));
#33598=CARTESIAN_POINT('Ctrl Pts',(-0.217886373242709,-0.0653490907656594,
0.796150794580307));
#33599=CARTESIAN_POINT('Ctrl Pts',(-0.0629708293942997,-0.218813637584587,
0.807264583637111));
#33600=CARTESIAN_POINT('Ctrl Pts',(0.149542981076344,-0.171418700808033,
0.818378372693914));
#33601=CARTESIAN_POINT('Ctrl Pts',(0.225195614202741,0.0325890023924215,
0.829492161750719));
#33602=CARTESIAN_POINT('Ctrl Pts',(0.0947155514542305,0.206917019327413,
0.840605950807523));
#33603=CARTESIAN_POINT('Ctrl Pts',(-0.122454283303893,0.191773665487537,
0.851719739864327));
#33604=CARTESIAN_POINT('Ctrl Pts',(-0.227542641392875,0.00113835931130726,
0.862833528921131));
#33605=CARTESIAN_POINT('Ctrl Pts',(-0.124357429349293,-0.190560134610961,
0.873947317977936));
#33606=CARTESIAN_POINT('Ctrl Pts',(0.0926529161707207,-0.20782568535688,
0.885061107034739));
#33607=CARTESIAN_POINT('Ctrl Pts',(0.224857326815389,-0.0348718222704234,
0.896174896091545));
#33608=CARTESIAN_POINT('Ctrl Pts',(0.151247103781158,0.170003640905229,
0.907288685148347));
#33609=CARTESIAN_POINT('Ctrl Pts',(-0.0608012185617612,0.219271263230777,
0.918402474205154));
#33610=CARTESIAN_POINT('Ctrl Pts',(-0.217197543051952,0.0678382370566187,
0.929516263261956));
#33611=CARTESIAN_POINT('Ctrl Pts',(-0.174790468634879,-0.145688327971602,
0.940630052318761));
#33612=CARTESIAN_POINT('Ctrl Pts',(0.0276042911522686,-0.225864489000412,
0.951743841375564));
#33613=CARTESIAN_POINT('Ctrl Pts',(0.20473253689515,-0.0993044393887096,
0.962857630432368));
#33614=CARTESIAN_POINT('Ctrl Pts',(0.194466766292811,0.118150151218368,
0.973971419489174));
#33615=CARTESIAN_POINT('Ctrl Pts',(0.00620336092773602,0.227460536413689,
0.985085208545976));
#33616=CARTESIAN_POINT('Ctrl Pts',(-0.187738052000287,0.128573729811465,
0.996198997602783));
#33617=CARTESIAN_POINT('Ctrl Pts',(-0.209840696339377,-0.0879980785663373,
1.00731278665958));
#33618=CARTESIAN_POINT('Ctrl Pts',(-0.0398737718241875,-0.224024243094024,
1.01842657571639));
#33619=CARTESIAN_POINT('Ctrl Pts',(0.166590068377075,-0.154998479698188,
1.02954036477319));
#33620=CARTESIAN_POINT('Ctrl Pts',(0.22057212966186,0.055899151215077,1.04065415383));
#33621=CARTESIAN_POINT('Ctrl Pts',(0.0726620192461797,0.215631654430176,
1.0517679428868));
#33622=CARTESIAN_POINT('Ctrl Pts',(-0.141756461448261,0.177994059256345,
1.06288173194361));
#33623=CARTESIAN_POINT('Ctrl Pts',(-0.226423645341368,-0.0225635171224834,
1.07399552100041));
#33624=CARTESIAN_POINT('Ctrl Pts',(-0.103842698840025,-0.202468450298578,
1.08510931005722));
#33625=CARTESIAN_POINT('Ctrl Pts',(0.113786647568658,-0.197051714816478,
1.09622309911402));
#33626=CARTESIAN_POINT('Ctrl Pts',(0.227265785027954,-0.0112713100190907,
1.10733688817082));
#33627=CARTESIAN_POINT('Ctrl Pts',(0.132725972082619,0.184825852650891,
1.11845067722763));
#33628=CARTESIAN_POINT('Ctrl Pts',(-0.0832994283252297,0.211749816328691,
1.12956446628443));
#33629=CARTESIAN_POINT('Ctrl Pts',(-0.223079917307022,0.0448567717109849,
1.14067825534124));
#33630=CARTESIAN_POINT('Ctrl Pts',(-0.158672828079473,-0.163094184762292,
1.15179204439804));
#33631=CARTESIAN_POINT('Ctrl Pts',(0.0509693001615336,-0.221763184309772,
1.16290583345485));
#33632=CARTESIAN_POINT('Ctrl Pts',(0.213958649933481,-0.0774498262924409,
1.17401962251165));
#33633=CARTESIAN_POINT('Ctrl Pts',(0.181109220965206,0.137754236070862,
1.18513341156845));
#33634=CARTESIAN_POINT('Ctrl Pts',(-0.0175115318707909,0.226870283919355,
1.19624720062525));
#33635=CARTESIAN_POINT('Ctrl Pts',(-0.20010378099117,0.108329388012377,
1.20736098968206));
#33636=CARTESIAN_POINT('Ctrl Pts',(-0.199538770039111,-0.109366625281109,
1.21847477873886));
#33637=CARTESIAN_POINT('Ctrl Pts',(-0.0163336599466904,-0.226958126152927,
1.22958856779567));
#33638=CARTESIAN_POINT('Ctrl Pts',(0.181821834331238,-0.13681228027675,
1.24070235685247));
#33639=CARTESIAN_POINT('Ctrl Pts',(0.213553741645938,0.0785593972935142,
1.25181614590928));
#33640=CARTESIAN_POINT('Ctrl Pts',(0.0498174873679621,0.222024767596873,
1.26292993496608));
#33641=CARTESIAN_POINT('Ctrl Pts',(-0.159517278066646,0.162268350186683,
1.27404372402289));
#33642=CARTESIAN_POINT('Ctrl Pts',(-0.222844069837872,-0.0460141283976122,
1.28515751307969));
#33643=CARTESIAN_POINT('Ctrl Pts',(-0.0821991572628677,-0.212179353423901,
1.29627130213649));
#33644=CARTESIAN_POINT('Ctrl Pts',(0.13368357615671,-0.184134409983696,
1.3073850911933));
#33645=CARTESIAN_POINT('Ctrl Pts',(0.227204216245135,0.0124508471406916,
1.3184988802501));
#33646=CARTESIAN_POINT('Ctrl Pts',(0.112762260533419,0.197639702675246,
1.32961266930691));
#33647=CARTESIAN_POINT('Ctrl Pts',(-0.104892271055723,0.20192669696399,
1.34072645836371));
#33648=CARTESIAN_POINT('Ctrl Pts',(-0.226537717387964,0.0213878955180253,
1.35184024742052));
#33649=CARTESIAN_POINT('Ctrl Pts',(-0.140830621883197,-0.178727489252595,
1.36295403647732));
#33650=CARTESIAN_POINT('Ctrl Pts',(0.0737803389603765,-0.215251576199333,
1.37406782553412));
#33651=CARTESIAN_POINT('Ctrl Pts',(0.220859318825196,-0.0547534543384197,
1.38518161459093));
#33652=CARTESIAN_POINT('Ctrl Pts',(0.165783259458819,0.155861125237303,
1.39629540364773));
#33653=CARTESIAN_POINT('Ctrl Pts',(-0.0410360974089359,0.223814249274108,
1.40740919270454));
#33654=CARTESIAN_POINT('Ctrl Pts',(-0.210294648920666,0.0869076527697323,
1.41852298176134));
#33655=CARTESIAN_POINT('Ctrl Pts',(-0.187068123403623,-0.129546504001961,
1.42963677081815));
#33656=CARTESIAN_POINT('Ctrl Pts',(0.0073839770225235,-0.227425276336115,
1.44075055987495));
#33657=CARTESIAN_POINT('Ctrl Pts',(0.195077439423252,-0.117139114382011,
1.45186434893176));
#33658=CARTESIAN_POINT('Ctrl Pts',(0.204214309414691,0.10036580802698,1.46297813798855));
#33659=CARTESIAN_POINT('Ctrl Pts',(0.0264315056232782,0.226004766949337,
1.47409192704536));
#33660=CARTESIAN_POINT('Ctrl Pts',(-0.175544354199732,0.144779001862013,
1.48520571610217));
#33661=CARTESIAN_POINT('Ctrl Pts',(-0.216842477383471,-0.0689646298380053,
1.49631950515897));
#33662=CARTESIAN_POINT('Ctrl Pts',(-0.0596622188548986,-0.21958414549715,
1.50743329421577));
#33663=CARTESIAN_POINT('Ctrl Pts',(0.152127539459117,-0.169215818301425,
1.51854708327258));
#33664=CARTESIAN_POINT('Ctrl Pts',(0.224673246667516,0.0360376966204509,
1.52966087232938));
#33665=CARTESIAN_POINT('Ctrl Pts',(0.0915729621635637,0.208305441316416,
1.54077466138618));
#33666=CARTESIAN_POINT('Ctrl Pts',(-0.125345052777559,0.189908963919433,
1.55188845044299));
#33667=CARTESIAN_POINT('Ctrl Pts',(-0.227533396633615,-0.00231355378679829,
1.56300223949979));
#33668=CARTESIAN_POINT('Ctrl Pts',(-0.121457694281633,-0.192418043741239,
1.5741160285566));
#33669=CARTESIAN_POINT('Ctrl Pts',(0.09578932997347,-0.206400892891616,
1.5852298176134));
#33670=CARTESIAN_POINT('Ctrl Pts',(0.225359836185271,-0.0314611767988859,
1.59634360667021));
#33671=CARTESIAN_POINT('Ctrl Pts',(0.148654890877534,0.172272463810048,
1.60745739572701));
#33672=CARTESIAN_POINT('Ctrl Pts',(-0.0641135751589405,0.218328616121778,
1.61857118478381));
#33673=CARTESIAN_POINT('Ctrl Pts',(-0.218201962540567,0.0645356727509123,
1.62968497384062));
#33674=CARTESIAN_POINT('Ctrl Pts',(-0.172560336221374,-0.148307520501026,
1.64079876289742));
#33675=CARTESIAN_POINT('Ctrl Pts',(0.0310137773775485,-0.225441420744716,
1.65191255195423));
#33676=CARTESIAN_POINT('Ctrl Pts',(0.206227346623875,-0.0961529471080275,
1.66302634101103));
#33677=CARTESIAN_POINT('Ctrl Pts',(0.192627368002909,0.121004839870914,
1.67414013006784));
#33678=CARTESIAN_POINT('Ctrl Pts',(0.00281312104568935,0.227677007397733,
1.68525391912464));
#33679=CARTESIAN_POINT('Ctrl Pts',(-0.189780348479797,0.125412896624096,
1.69636770818145));
#33680=CARTESIAN_POINT('Ctrl Pts',(-0.202037965727701,-0.0184776408472769,
1.70377690088598));
#33681=CARTESIAN_POINT('Ctrl Pts',(-0.17638991251268,-0.0771314832491481,
1.70748149723825));
#33682=CARTESIAN_POINT('Ctrl Pts',(-0.156520011427169,0.133121980333222,
0.777555508285253));
#33683=CARTESIAN_POINT('Ctrl Pts',(-0.200786236992242,0.081075352766987,
0.781260104637521));
#33684=CARTESIAN_POINT('Ctrl Pts',(-0.232552346335619,-0.0697477504548899,
0.788669297342057));
#33685=CARTESIAN_POINT('Ctrl Pts',(-0.06720940785972,-0.233542025016153,
0.799783086398862));
#33686=CARTESIAN_POINT('Ctrl Pts',(0.159608747485041,-0.182956926059375,
0.810896875455666));
#33687=CARTESIAN_POINT('Ctrl Pts',(0.240353573690459,0.0347825743221341,
0.82201066451247));
#33688=CARTESIAN_POINT('Ctrl Pts',(0.101090873180113,0.220844643128561,
0.833124453569275));
#33689=CARTESIAN_POINT('Ctrl Pts',(-0.130696704329673,0.204681987270635,
0.844238242626078));
#33690=CARTESIAN_POINT('Ctrl Pts',(-0.242858579725743,0.00121498249237738,
0.855352031682883));
#33691=CARTESIAN_POINT('Ctrl Pts',(-0.132727951496213,-0.203386773400678,
0.866465820739686));
#33692=CARTESIAN_POINT('Ctrl Pts',(0.0988894015246068,-0.221814471640749,
0.877579609796491));
#33693=CARTESIAN_POINT('Ctrl Pts',(0.239992516114928,-0.0372190512389329,
0.888693398853296));
#33694=CARTESIAN_POINT('Ctrl Pts',(0.161427575012208,0.181446618206226,
0.899807187910099));
#33695=CARTESIAN_POINT('Ctrl Pts',(-0.0648937601106981,0.234030453531351,
0.910920976966904));
#33696=CARTESIAN_POINT('Ctrl Pts',(-0.231817150854124,0.0724044416546206,
0.922034766023707));
#33697=CARTESIAN_POINT('Ctrl Pts',(-0.186555648217912,-0.155494636948999,
0.933148555080512));
#33698=CARTESIAN_POINT('Ctrl Pts',(0.029462341223335,-0.241067470577576,
0.944262344137316));
#33699=CARTESIAN_POINT('Ctrl Pts',(0.218513122769618,-0.105988640031487,
0.95537613319412));
#33700=CARTESIAN_POINT('Ctrl Pts',(0.207556361201707,0.126102860297433,
0.966489922250924));
#33701=CARTESIAN_POINT('Ctrl Pts',(0.00662091032790181,0.242770948244842,
0.977603711307729));
#33702=CARTESIAN_POINT('Ctrl Pts',(-0.200374735874429,0.13722805194188,
0.988717500364533));
#33703=CARTESIAN_POINT('Ctrl Pts',(-0.223965113394512,-0.0939212459185429,
0.999831289421336));
#33704=CARTESIAN_POINT('Ctrl Pts',(-0.0425576829655005,-0.239103357370329,
1.01094507847814));
#33705=CARTESIAN_POINT('Ctrl Pts',(0.177803277464009,-0.16543145675345,
1.02205886753495));
#33706=CARTESIAN_POINT('Ctrl Pts',(0.235418881528546,0.0596617336815061,
1.03317265659175));
#33707=CARTESIAN_POINT('Ctrl Pts',(0.0775529135379212,0.230145861972334,
1.04428644564855));
#33708=CARTESIAN_POINT('Ctrl Pts',(-0.151298115744515,0.18997487313149,
1.05540023470536));
#33709=CARTESIAN_POINT('Ctrl Pts',(-0.241664263837854,-0.0240822717379046,
1.06651402376216));
#33710=CARTESIAN_POINT('Ctrl Pts',(-0.110832370586897,-0.216096640074974,
1.07762781281897));
#33711=CARTESIAN_POINT('Ctrl Pts',(0.121445648389767,-0.210315303100593,
1.08874160187577));
#33712=CARTESIAN_POINT('Ctrl Pts',(0.242563088106409,-0.0120299840334481,
1.09985539093258));
#33713=CARTESIAN_POINT('Ctrl Pts',(0.141659782427545,0.197266515834691,
1.11096917998938));
#33714=CARTESIAN_POINT('Ctrl Pts',(-0.0889063286388705,0.226002736612265,
1.12208296904618));
#33715=CARTESIAN_POINT('Ctrl Pts',(-0.238095468835566,0.0478760895194249,
1.13319675810299));
#33716=CARTESIAN_POINT('Ctrl Pts',(-0.169353126220915,-0.174072085260317,
1.14431054715979));
#33717=CARTESIAN_POINT('Ctrl Pts',(0.0544000534188783,-0.236690106290626,
1.1554243362166));
#33718=CARTESIAN_POINT('Ctrl Pts',(0.228360247225775,-0.0826629887842052,
1.1665381252734));
#33719=CARTESIAN_POINT('Ctrl Pts',(0.193299716965591,0.147026499818165,
1.1776519143302));
#33720=CARTESIAN_POINT('Ctrl Pts',(-0.0186902364010947,0.242140965743205,
1.18876570338701));
#33721=CARTESIAN_POINT('Ctrl Pts',(-0.213572804428157,0.115621059658089,
1.19987949244381));
#33722=CARTESIAN_POINT('Ctrl Pts',(-0.212969762481792,-0.116728113564033,
1.21099328150062));
#33723=CARTESIAN_POINT('Ctrl Pts',(-0.0174330816944656,-0.242234720654174,
1.22210707055742));
#33724=CARTESIAN_POINT('Ctrl Pts',(0.194060296472398,-0.146021140800962,
1.23322085961423));
#33725=CARTESIAN_POINT('Ctrl Pts',(0.227928084484629,0.0838472452197288,
1.24433464867103));
#33726=CARTESIAN_POINT('Ctrl Pts',(0.053170711887795,0.236969296798376,
1.25544843772783));
#33727=CARTESIAN_POINT('Ctrl Pts',(-0.170254416296827,0.17319066360285,
1.26656222678464));
#33728=CARTESIAN_POINT('Ctrl Pts',(-0.237843746428552,-0.0491113481040567,
1.27767601584144));
#33729=CARTESIAN_POINT('Ctrl Pts',(-0.0877319981226961,-0.226461185930791,
1.28878980489824));
#33730=CARTESIAN_POINT('Ctrl Pts',(0.142681843013418,-0.196528532030473,
1.29990359395505));
#33731=CARTESIAN_POINT('Ctrl Pts',(0.242497375117146,0.0132889160223372,
1.31101738301185));
#33732=CARTESIAN_POINT('Ctrl Pts',(0.120352309668968,0.210942868533614,
1.32213117206866));
#33733=CARTESIAN_POINT('Ctrl Pts',(-0.111952589707427,0.215518421220722,
1.33324496112546));
#33734=CARTESIAN_POINT('Ctrl Pts',(-0.241786014095534,0.0228275188203595,
1.34435875018226));
#33735=CARTESIAN_POINT('Ctrl Pts',(-0.150309957742793,-0.190757670439842,
1.35547253923907));
#33736=CARTESIAN_POINT('Ctrl Pts',(0.0787465075641072,-0.229740200603712,
1.36658632829588));
#33737=CARTESIAN_POINT('Ctrl Pts',(0.235725401448916,-0.0584389197308638,
1.37770011735268));
#33738=CARTESIAN_POINT('Ctrl Pts',(0.176942162084499,0.166352167127356,
1.38881390640948));
#33739=CARTESIAN_POINT('Ctrl Pts',(-0.0437982449057285,0.238879228826581,
1.39992769546629));
#33740=CARTESIAN_POINT('Ctrl Pts',(-0.224449621610114,0.0927574233548304,
1.41104148452309));
#33741=CARTESIAN_POINT('Ctrl Pts',(-0.199659714256911,-0.13826630374757,
1.42215527357989));
#33742=CARTESIAN_POINT('Ctrl Pts',(0.00788099391586731,-0.242733314804761,
1.4332690626367));
#33743=CARTESIAN_POINT('Ctrl Pts',(0.208208138856338,-0.125023770379934,
1.4443828516935));
#33744=CARTESIAN_POINT('Ctrl Pts',(0.217960013299196,0.107121449594028,
1.45549664075031));
#33745=CARTESIAN_POINT('Ctrl Pts',(0.028210615278035,0.241217190661839,
1.46661042980711));
#33746=CARTESIAN_POINT('Ctrl Pts',(-0.187360277963068,0.154524103926572,
1.47772421886392));
#33747=CARTESIAN_POINT('Ctrl Pts',(-0.23143818564818,-0.0736066521476796,
1.48883800792072));
#33748=CARTESIAN_POINT('Ctrl Pts',(-0.0636780941176189,-0.234364395962394,
1.49995179697753));
#33749=CARTESIAN_POINT('Ctrl Pts',(0.162367272982574,-0.180605767113594,
1.51106558603433));
#33750=CARTESIAN_POINT('Ctrl Pts',(0.2397960454974,0.0384634008125035,1.52217937509113));
#33751=CARTESIAN_POINT('Ctrl Pts',(0.0977367556084749,0.222326520064881,
1.53329316414794));
#33752=CARTESIAN_POINT('Ctrl Pts',(-0.133782052044684,0.202691772286445,
1.54440695320474));
#33753=CARTESIAN_POINT('Ctrl Pts',(-0.242848712699985,-0.00246927953082339,
1.55552074226155));
#33754=CARTESIAN_POINT('Ctrl Pts',(-0.129633034711377,-0.205369738746763,
1.56663453131835));
#33755=CARTESIAN_POINT('Ctrl Pts',(0.102236927935064,-0.220293776124516,
1.57774832037515));
#33756=CARTESIAN_POINT('Ctrl Pts',(0.240528849485768,-0.0335788345740686,
1.58886210943196));
#33757=CARTESIAN_POINT('Ctrl Pts',(0.158660879766572,0.183868156010923,
1.59997589848876));
#33758=CARTESIAN_POINT('Ctrl Pts',(-0.0684290720584363,0.233024356666725,
1.61108968754557));
#33759=CARTESIAN_POINT('Ctrl Pts',(-0.23288917800895,0.0688795811193509,
1.62220347660237));
#33760=CARTESIAN_POINT('Ctrl Pts',(-0.184175405168835,-0.158290127824162,
1.63331726565918));
#33761=CARTESIAN_POINT('Ctrl Pts',(0.0331013206128567,-0.240615925517378,
1.64443105471598));
#33762=CARTESIAN_POINT('Ctrl Pts',(0.220108548424591,-0.102625020207888,
1.65554484377279));
#33763=CARTESIAN_POINT('Ctrl Pts',(0.205593152664173,0.129149698584414,
1.66665863282959));
#33764=CARTESIAN_POINT('Ctrl Pts',(0.00300247275662535,0.243001989931863,
1.67777242188639));
#33765=CARTESIAN_POINT('Ctrl Pts',(-0.202554499717183,0.133854462473394,
1.6888862109432));
#33766=CARTESIAN_POINT('Ctrl Pts',(-0.215637179506013,-0.0197213743559566,
1.69629540364773));
#33767=CARTESIAN_POINT('Ctrl Pts',(-0.188262750966373,-0.0823232180103128,
1.7));
#33768=CARTESIAN_POINT('Ctrl Pts',(-0.126907087985236,0.107935865304854,
0.8));
#33769=CARTESIAN_POINT('Ctrl Pts',(-0.135120815820747,0.100273328983374,
0.8));
#33770=CARTESIAN_POINT('Ctrl Pts',(-0.142440162795362,0.0917707005673423,
0.8));
#33771=CARTESIAN_POINT('Ctrl Pts',(-0.148860420961125,0.0826220371750322,
0.8));
#33772=CARTESIAN_POINT('Ctrl Pts',(-0.153630780718642,0.0758244264629785,
0.8));
#33773=CARTESIAN_POINT('Ctrl Pts',(-0.157904437427575,0.0686688635836137,
0.8));
#33774=CARTESIAN_POINT('Ctrl Pts',(-0.161669292800466,0.0612205436816197,
0.8));
#33775=CARTESIAN_POINT('Ctrl Pts',(-0.163886790527543,0.0568334873893247,
0.8));
#33776=CARTESIAN_POINT('Ctrl Pts',(-0.165929164676721,0.0523396591094527,
0.8));
#33777=CARTESIAN_POINT('Ctrl Pts',(-0.167781485419322,0.0477808011974605,
0.8));
#33778=CARTESIAN_POINT('Ctrl Pts',(-0.172341905336402,0.0365568776388491,
0.8));
#33779=CARTESIAN_POINT('Ctrl Pts',(-0.175769282371032,0.024914892102173,
0.8));
#33780=CARTESIAN_POINT('Ctrl Pts',(-0.178035222124413,0.0130530737274266,
0.8));
#33781=CARTESIAN_POINT('Ctrl Pts',(-0.179475251863618,0.00551475714368376,
0.8));
#33782=CARTESIAN_POINT('Ctrl Pts',(-0.180445476974817,-0.00211322491662525,
0.8));
#33783=CARTESIAN_POINT('Ctrl Pts',(-0.180929041702956,-0.00978511330991493,
0.8));
#33784=CARTESIAN_POINT('Ctrl Pts',(-0.181154762272538,-0.0133662326867636,
0.8));
#33785=CARTESIAN_POINT('Ctrl Pts',(-0.181273901675413,-0.0169534510679824,
0.8));
#33786=CARTESIAN_POINT('Ctrl Pts',(-0.181285306139082,-0.0205319858475477,
0.8));
#33787=CARTESIAN_POINT('Ctrl Pts',(-0.18132084415518,-0.0316832359459324,
0.8));
#33788=CARTESIAN_POINT('Ctrl Pts',(-0.180314596981932,-0.0427772557222799,
0.8));
#33789=CARTESIAN_POINT('Ctrl Pts',(-0.178232649680767,-0.053673233795859,
0.8));
#33790=CARTESIAN_POINT('Ctrl Pts',(-0.177072367625385,-0.0597456294936455,
0.8));
#33791=CARTESIAN_POINT('Ctrl Pts',(-0.175577442236952,-0.0657567536750286,
0.8));
#33792=CARTESIAN_POINT('Ctrl Pts',(-0.173766632602371,-0.0716904360104152,
0.8));
#33793=CARTESIAN_POINT('Ctrl Pts',(-0.17263375533703,-0.0754026615746807,
0.8));
#33794=CARTESIAN_POINT('Ctrl Pts',(-0.171376588698951,-0.0790860937830887,
0.8));
#33795=CARTESIAN_POINT('Ctrl Pts',(-0.17000084111904,-0.0827319119339195,
0.8));
#33796=CARTESIAN_POINT('Ctrl Pts',(-0.165618690539351,-0.0943448882941177,
0.8));
#33797=CARTESIAN_POINT('Ctrl Pts',(-0.160069009775015,-0.105495622492882,
0.8));
#33798=CARTESIAN_POINT('Ctrl Pts',(-0.153517412526831,-0.116061366452211,
0.8));
#33799=CARTESIAN_POINT('Ctrl Pts',(-0.149177021710609,-0.123061103510275,
0.8));
#33800=CARTESIAN_POINT('Ctrl Pts',(-0.144395700078728,-0.129804236115551,
0.8));
#33801=CARTESIAN_POINT('Ctrl Pts',(-0.139210064136084,-0.136252864813496,
0.8));
#33802=CARTESIAN_POINT('Ctrl Pts',(-0.13649895134849,-0.139624285391187,
0.8));
#33803=CARTESIAN_POINT('Ctrl Pts',(-0.133675938748059,-0.142916515743411,
0.8));
#33804=CARTESIAN_POINT('Ctrl Pts',(-0.130749381376745,-0.146119375612755,
0.8));
#33805=CARTESIAN_POINT('Ctrl Pts',(-0.124483125872831,-0.152977241609597,
0.8));
#33806=CARTESIAN_POINT('Ctrl Pts',(-0.117767487241387,-0.159399582279811,
0.8));
#33807=CARTESIAN_POINT('Ctrl Pts',(-0.110656616745505,-0.165335584860524,
0.8));
#33808=CARTESIAN_POINT('Ctrl Pts',(-0.106173937599239,-0.169077629522446,
0.8));
#33809=CARTESIAN_POINT('Ctrl Pts',(-0.10153394483554,-0.172626328540978,
0.8));
#33810=CARTESIAN_POINT('Ctrl Pts',(-0.0967480797506452,-0.175967583788754,
0.8));
#33811=CARTESIAN_POINT('Ctrl Pts',(-0.0926327467056763,-0.178840706597052,
0.8));
#33812=CARTESIAN_POINT('Ctrl Pts',(-0.0884162860091264,-0.181555556620875,
0.8));
#33813=CARTESIAN_POINT('Ctrl Pts',(-0.0841104480426287,-0.184101786598396,
0.8));
#33814=CARTESIAN_POINT('Ctrl Pts',(-0.0753786167196158,-0.189265299681399,
0.8));
#33815=CARTESIAN_POINT('Ctrl Pts',(-0.0662752406232737,-0.193739549767325,
0.8));
#33816=CARTESIAN_POINT('Ctrl Pts',(-0.0568593821206139,-0.197450435399565,
0.8));
#33817=CARTESIAN_POINT('Ctrl Pts',(-0.0556199805901397,-0.197938896152316,
0.8));
#33818=CARTESIAN_POINT('Ctrl Pts',(-0.0543751496950137,-0.198414110578975,
0.8));
#33819=CARTESIAN_POINT('Ctrl Pts',(-0.0531250805644623,-0.198876136975596,
0.8));
#33820=CARTESIAN_POINT('Ctrl Pts',(0.166729862742343,-0.000130123946020723,
0.912851963660979));
#33821=CARTESIAN_POINT('Ctrl Pts',(0.166803013417109,-0.0086545516860567,
0.912280605963333));
#33822=CARTESIAN_POINT('Ctrl Pts',(0.166205714872852,-0.0171686904331816,
0.911709248265688));
#33823=CARTESIAN_POINT('Ctrl Pts',(0.164902316607877,-0.0255733139699205,
0.911137890568042));
#33824=CARTESIAN_POINT('Ctrl Pts',(0.156451280631859,-0.08006761381865,
0.907433294215774));
#33825=CARTESIAN_POINT('Ctrl Pts',(0.118315613047404,-0.129957863303896,
0.903728697863506));
#33826=CARTESIAN_POINT('Ctrl Pts',(0.0679483908354429,-0.152412778753583,
0.900024101511237));
#33827=CARTESIAN_POINT('Ctrl Pts',(0.017581168623482,-0.17486769420327,
0.896319505158969));
#33828=CARTESIAN_POINT('Ctrl Pts',(-0.045017608215985,-0.169887275617398,
0.892614908806701));
#33829=CARTESIAN_POINT('Ctrl Pts',(-0.0911993932476663,-0.139748404661014,
0.888910312454434));
#33830=CARTESIAN_POINT('Ctrl Pts',(-0.137381178279348,-0.109609533704629,
0.885205716102165));
#33831=CARTESIAN_POINT('Ctrl Pts',(-0.167145971503243,-0.0543122103777309,
0.881501119749897));
#33832=CARTESIAN_POINT('Ctrl Pts',(-0.16687148086939,0.000831769447747308,
0.877796523397629));
#33833=CARTESIAN_POINT('Ctrl Pts',(-0.166596990235537,0.0559757492732252,
0.874091927045361));
#33834=CARTESIAN_POINT('Ctrl Pts',(-0.136283215743936,0.110966385597283,
0.870387330693093));
#33835=CARTESIAN_POINT('Ctrl Pts',(-0.0898039369556689,0.140645828726608,
0.866682734340825));
#33836=CARTESIAN_POINT('Ctrl Pts',(-0.0433246581674013,0.170325271855933,
0.862978137988557));
#33837=CARTESIAN_POINT('Ctrl Pts',(0.0193201249175325,0.174693521790525,
0.859273541636289));
#33838=CARTESIAN_POINT('Ctrl Pts',(0.0694616476641393,0.151734327892468,
0.855568945284021));
#33839=CARTESIAN_POINT('Ctrl Pts',(0.119603170410746,0.12877513399441,0.851864348931753));
#33840=CARTESIAN_POINT('Ctrl Pts',(0.157241432819026,0.0784884962637034,
0.848159752579484));
#33841=CARTESIAN_POINT('Ctrl Pts',(0.16514918952844,0.0239211592586256,
0.844455156227216));
#33842=CARTESIAN_POINT('Ctrl Pts',(0.166289903708577,0.0160496809897125,
0.843920758705137));
#33843=CARTESIAN_POINT('Ctrl Pts',(0.16681196167645,0.00808912649634021,
0.843386361183058));
#33844=CARTESIAN_POINT('Ctrl Pts',(0.166745353727506,0.000120148921586877,
0.842851963660979));
#33845=CARTESIAN_POINT('Ctrl Pts',(0.0530170217188587,-0.198517432567173,
0.8));
#33846=CARTESIAN_POINT('Ctrl Pts',(0.119028790974553,-0.18088801151799,
0.803704596352268));
#33847=CARTESIAN_POINT('Ctrl Pts',(0.230942256426658,-0.0749063428374961,
0.811113789056804));
#33848=CARTESIAN_POINT('Ctrl Pts',(0.188114631577322,0.153856547759368,
0.822227578113608));
#33849=CARTESIAN_POINT('Ctrl Pts',(-0.0272119409517698,0.241262826763902,
0.833341367170412));
#33850=CARTESIAN_POINT('Ctrl Pts',(-0.217470922739143,0.108102090643486,
0.844455156227217));
#33851=CARTESIAN_POINT('Ctrl Pts',(-0.208759451561279,-0.124141896006793,
0.85556894528402));
#33852=CARTESIAN_POINT('Ctrl Pts',(-0.00892472216375234,-0.242686445659381,
0.866682734340826));
#33853=CARTESIAN_POINT('Ctrl Pts',(0.199056267666047,-0.139134372529335,
0.877796523397629));
#33854=CARTESIAN_POINT('Ctrl Pts',(0.224850619698646,0.091788306500609,
0.888910312454433));
#33855=CARTESIAN_POINT('Ctrl Pts',(0.0448304764247631,0.238686010114805,
0.900024101511237));
#33856=CARTESIAN_POINT('Ctrl Pts',(-0.176220286722883,0.167116974718297,
0.911137890568042));
#33857=CARTESIAN_POINT('Ctrl Pts',(-0.235976306336092,-0.0574188764093974,
0.922251679624847));
#33858=CARTESIAN_POINT('Ctrl Pts',(-0.0797396575425977,-0.229397140881452,
0.933365468681649));
#33859=CARTESIAN_POINT('Ctrl Pts',(0.14948314505928,-0.19140635164143,0.944479257738454));
#33860=CARTESIAN_POINT('Ctrl Pts',(0.241882569451173,0.0217812340617926,
0.955593046795258));
#33861=CARTESIAN_POINT('Ctrl Pts',(0.112884009708659,0.215032004451281,
0.966706835852063));
#33862=CARTESIAN_POINT('Ctrl Pts',(-0.119438498942156,0.211461649464463,
0.977820624908867));
#33863=CARTESIAN_POINT('Ctrl Pts',(-0.242437629122786,0.0143379927471741,
0.988934413965671));
#33864=CARTESIAN_POINT('Ctrl Pts',(-0.143530830111561,-0.195909362177039,
1.00004820302247));
#33865=CARTESIAN_POINT('Ctrl Pts',(0.086751356142284,-0.226838671363958,
1.01116199207928));
#33866=CARTESIAN_POINT('Ctrl Pts',(0.237629047152892,-0.05013996417456,
1.02227578113608));
#33867=CARTESIAN_POINT('Ctrl Pts',(0.1710021738693,0.172452416697446,1.03338957019289));
#33868=CARTESIAN_POINT('Ctrl Pts',(-0.0521449271278155,0.237197146991165,
1.04450335924969));
#33869=CARTESIAN_POINT('Ctrl Pts',(-0.227563185653378,0.0848326375129703,
1.0556171483065));
#33870=CARTESIAN_POINT('Ctrl Pts',(-0.194690279246867,-0.145180146557101,
1.0667309373633));
#33871=CARTESIAN_POINT('Ctrl Pts',(0.0163848475034698,-0.242307896337387,
1.0778447264201));
#33872=CARTESIAN_POINT('Ctrl Pts',(0.212462737615647,-0.117648480480376,
1.08895851547691));
#33873=CARTESIAN_POINT('Ctrl Pts',(0.214071074445423,0.114695923700636,
1.10007230453371));
#33874=CARTESIAN_POINT('Ctrl Pts',(0.019737729131079,0.242057848222183,
1.11118609359052));
#33875=CARTESIAN_POINT('Ctrl Pts',(-0.192661783512051,0.147861479120299,
1.12229988264732));
#33876=CARTESIAN_POINT('Ctrl Pts',(-0.228715780766039,-0.0816741786716276,
1.13341367170413));
#33877=CARTESIAN_POINT('Ctrl Pts',(-0.0554236300753314,-0.236452534483491,
1.14452746076093));
#33878=CARTESIAN_POINT('Ctrl Pts',(0.168598397772042,-0.174803203925221,
1.15564124981773));
#33879=CARTESIAN_POINT('Ctrl Pts',(0.238300400101745,0.0468454815872605,
1.16675503887454));
#33880=CARTESIAN_POINT('Ctrl Pts',(0.0898833437085198,0.225615966539919,
1.17786882793134));
#33881=CARTESIAN_POINT('Ctrl Pts',(-0.140804956527845,0.197877598659039,
1.18898261698814));
#33882=CARTESIAN_POINT('Ctrl Pts',(-0.242612883217311,-0.0109803793588139,
1.20009640604495));
#33883=CARTESIAN_POINT('Ctrl Pts',(-0.12235448648082,-0.2097878916237,1.21121019510175));
#33884=CARTESIAN_POINT('Ctrl Pts',(0.109896359325859,-0.21657416752884,
1.22232398415856));
#33885=CARTESIAN_POINT('Ctrl Pts',(0.241557821132076,-0.0251276517767584,
1.23343777321536));
#33886=CARTESIAN_POINT('Ctrl Pts',(0.152118669804104,0.189318488613562,
1.24455156227217));
#33887=CARTESIAN_POINT('Ctrl Pts',(-0.0765564251386213,0.230479269358191,
1.25566535132897));
#33888=CARTESIAN_POINT('Ctrl Pts',(-0.23515855594305,0.0606797610465845,
1.26677914038578));
#33889=CARTESIAN_POINT('Ctrl Pts',(-0.178517393613401,-0.164660620706261,
1.27789292944258));
#33890=CARTESIAN_POINT('Ctrl Pts',(0.0415227636155418,-0.239285268948212,
1.28900671849938));
#33891=CARTESIAN_POINT('Ctrl Pts',(0.223556664406995,-0.0948893968423596,
1.30012050755619));
#33892=CARTESIAN_POINT('Ctrl Pts',(0.200966614961749,0.136359816312279,
1.31123429661299));
#33893=CARTESIAN_POINT('Ctrl Pts',(-0.00557045627447471,0.242797343170749,
1.3223480856698));
#33894=CARTESIAN_POINT('Ctrl Pts',(-0.207008825709279,0.126999708315969,
1.3334618747266));
#33895=CARTESIAN_POINT('Ctrl Pts',(-0.218969669332857,-0.105042199835232,
1.3445756637834));
#33896=CARTESIAN_POINT('Ctrl Pts',(-0.0305050913306782,-0.240937791217362,
1.35568945284021));
#33897=CARTESIAN_POINT('Ctrl Pts',(0.185881142716884,-0.15630028987845,
1.36680324189701));
#33898=CARTESIAN_POINT('Ctrl Pts',(0.23212825880178,0.0714006393532108,
1.37791703095382));
#33899=CARTESIAN_POINT('Ctrl Pts',(0.0659057470887793,0.233747753644337,
1.38903082001062));
#33900=CARTESIAN_POINT('Ctrl Pts',(-0.160641042350602,0.182142898149225,
1.40014460906743));
#33901=CARTESIAN_POINT('Ctrl Pts',(-0.240151263944613,-0.0361794176709605,
1.41125839812423));
#33902=CARTESIAN_POINT('Ctrl Pts',(-0.0998483101275995,-0.221386302178844,
1.42237218718103));
#33903=CARTESIAN_POINT('Ctrl Pts',(0.131846934264022,-0.203955793640817,
1.43348597623784));
#33904=CARTESIAN_POINT('Ctrl Pts',(0.242861184558351,0.00015776588975909,
1.44459976529464));
#33905=CARTESIAN_POINT('Ctrl Pts',(0.13158183823911,0.204126920402922,1.45571355435144));
#33906=CARTESIAN_POINT('Ctrl Pts',(-0.10013585656473,0.221256389923926,
1.46682734340825));
#33907=CARTESIAN_POINT('Ctrl Pts',(-0.240198066802314,0.0358673761285168,
1.47794113246505));
#33908=CARTESIAN_POINT('Ctrl Pts',(-0.160404261381875,-0.182351453033287,
1.48905492152186));
#33909=CARTESIAN_POINT('Ctrl Pts',(0.0662093815164626,-0.233661930697804,
1.50016871057866));
#33910=CARTESIAN_POINT('Ctrl Pts',(0.232220830617013,-0.0710989904726924,
1.51128249963547));
#33911=CARTESIAN_POINT('Ctrl Pts',(0.185677912288661,0.156541656658069,
1.52239628869227));
#33912=CARTESIAN_POINT('Ctrl Pts',(-0.0308180903310451,0.240897960470908,
1.53351007774908));
#33913=CARTESIAN_POINT('Ctrl Pts',(-0.219105973246366,0.104757609325286,
1.54462386680588));
#33914=CARTESIAN_POINT('Ctrl Pts',(-0.206843620635952,-0.127268531807556,
1.55573765586268));
#33915=CARTESIAN_POINT('Ctrl Pts',(-0.00525505851706014,-0.242804414954791,
1.56685144491949));
#33916=CARTESIAN_POINT('Ctrl Pts',(0.201143714017778,-0.136098524667356,
1.57796523397629));
#33917=CARTESIAN_POINT('Ctrl Pts',(0.223432989115882,0.0951796228419585,
1.5890790230331));
#33918=CARTESIAN_POINT('Ctrl Pts',(0.041212233239435,0.2393392912824,1.6001928120899));
#33919=CARTESIAN_POINT('Ctrl Pts',(-0.178731921787321,0.164428017156146,
1.6113066011467));
#33920=CARTESIAN_POINT('Ctrl Pts',(-0.235078089364662,-0.0609842187918821,
1.62242039020351));
#33921=CARTESIAN_POINT('Ctrl Pts',(-0.0762596568913861,-0.230580482955351,
1.63353417926032));
#33922=CARTESIAN_POINT('Ctrl Pts',(0.15236975797671,-0.18911696954633,1.64464796831712));
#33923=CARTESIAN_POINT('Ctrl Pts',(0.241514918660579,0.0254343397173533,
1.65576175737392));
#33924=CARTESIAN_POINT('Ctrl Pts',(0.109634140470589,0.216730418270261,
1.66687554643072));
#33925=CARTESIAN_POINT('Ctrl Pts',(-0.122663843019391,0.209602590285094,
1.67798933548753));
#33926=CARTESIAN_POINT('Ctrl Pts',(-0.242556018767321,0.0107153659861808,
1.68910312454434));
#33927=CARTESIAN_POINT('Ctrl Pts',(-0.140685982558438,-0.198157528783211,
1.70021691360114));
#33928=CARTESIAN_POINT('Ctrl Pts',(0.0904627772969653,-0.225303732602113,
1.71133070265794));
#33929=CARTESIAN_POINT('Ctrl Pts',(0.188575434363683,-0.106431345694512,
1.71873989536248));
#33930=CARTESIAN_POINT('Ctrl Pts',(0.201667586144654,-0.0393720754290199,
1.72244449171475));
#33931=CARTESIAN_POINT('Ctrl Pts',(0.0496734897087673,-0.185997880000277,
0.792518502761751));
#33932=CARTESIAN_POINT('Ctrl Pts',(0.111522209883364,-0.169480262890401,
0.796223099114019));
#33933=CARTESIAN_POINT('Ctrl Pts',(0.216377824064917,-0.0701823552026538,
0.803632291818555));
#33934=CARTESIAN_POINT('Ctrl Pts',(0.176251134310715,0.144153545294923,
0.814746080875359));
#33935=CARTESIAN_POINT('Ctrl Pts',(-0.025495812948363,0.226047524998972,
0.825859869932164));
#33936=CARTESIAN_POINT('Ctrl Pts',(-0.203756063475674,0.101284604698293,
0.836973658988968));
#33937=CARTESIAN_POINT('Ctrl Pts',(-0.195593983451704,-0.116312855641356,
0.848087448045772));
#33938=CARTESIAN_POINT('Ctrl Pts',(-0.0083618822819891,-0.227381363005354,
0.859201237102576));
#33939=CARTESIAN_POINT('Ctrl Pts',(0.186502733326074,-0.130359827804384,
0.87031502615938));
#33940=CARTESIAN_POINT('Ctrl Pts',(0.210670357962369,0.0859996535173407,
0.881428815216184));
#33941=CARTESIAN_POINT('Ctrl Pts',(0.0420032309836913,0.223633215949719,
0.892542604272988));
#33942=CARTESIAN_POINT('Ctrl Pts',(-0.16510690935118,0.156577700042264,
0.903656393329793));
#33943=CARTESIAN_POINT('Ctrl Pts',(-0.221094400331606,-0.0537977403094414,
0.914770182386598));
#33944=CARTESIAN_POINT('Ctrl Pts',(-0.0747108556819193,-0.214930151626042,
0.925883971443401));
#33945=CARTESIAN_POINT('Ctrl Pts',(0.140055952352658,-0.179335261208594,
0.936997760500206));
#33946=CARTESIAN_POINT('Ctrl Pts',(0.226628183455449,0.0204075949748767,
0.948111549557009));
#33947=CARTESIAN_POINT('Ctrl Pts',(0.105764950816784,0.201470956192298,
0.959225338613814));
#33948=CARTESIAN_POINT('Ctrl Pts',(-0.111906079513391,0.198125766554245,
0.970339127670618));
#33949=CARTESIAN_POINT('Ctrl Pts',(-0.227148238147163,0.0134337635740443,
0.981452916727423));
#33950=CARTESIAN_POINT('Ctrl Pts',(-0.134479021666759,-0.183554288235144,
0.992566705784226));
#33951=CARTESIAN_POINT('Ctrl Pts',(0.0812803597193106,-0.212533032641853,
1.00368049484103));
#33952=CARTESIAN_POINT('Ctrl Pts',(0.222642910626845,-0.0469778745330203,
1.01479428389783));
#33953=CARTESIAN_POINT('Ctrl Pts',(0.160217878116906,0.161576661010844,
1.02590807295464));
#33954=CARTESIAN_POINT('Ctrl Pts',(-0.0488563939857563,0.222238248359082,
1.03702186201144));
#33955=CARTESIAN_POINT('Ctrl Pts',(-0.21321185525264,0.0794826455702088,
1.04813565106825));
#33956=CARTESIAN_POINT('Ctrl Pts',(-0.182412087081199,-0.136024323549586,
1.05924944012505));
#33957=CARTESIAN_POINT('Ctrl Pts',(0.0153515329125665,-0.227026686992996,
1.07036322918186));
#33958=CARTESIAN_POINT('Ctrl Pts',(0.199063720825595,-0.110228949022901,
1.08147701823866));
#33959=CARTESIAN_POINT('Ctrl Pts',(0.200570627482587,0.107462595990271,
1.09259080729546));
#33960=CARTESIAN_POINT('Ctrl Pts',(0.0184929642043311,0.226792408226016,
1.10370459635227));
#33961=CARTESIAN_POINT('Ctrl Pts',(-0.180511518947779,0.138536557190134,
1.11481838540907));
#33962=CARTESIAN_POINT('Ctrl Pts',(-0.214291761660261,-0.0765233757420587,
1.12593217446588));
#33963=CARTESIAN_POINT('Ctrl Pts',(-0.0519283246948251,-0.221540595029306,
1.13704596352268));
#33964=CARTESIAN_POINT('Ctrl Pts',(0.157965696772913,-0.163779195241938,
1.14815975257948));
#33965=CARTESIAN_POINT('Ctrl Pts',(0.22327192453058,0.0438911593311794,
1.15927354163629));
#33966=CARTESIAN_POINT('Ctrl Pts',(0.0842148276900768,0.211387438009701,
1.17038733069309));
#33967=CARTESIAN_POINT('Ctrl Pts',(-0.131925055996524,0.185398397380911,
1.1815011197499));
#33968=CARTESIAN_POINT('Ctrl Pts',(-0.227312439797474,-0.0102878989312292,
1.1926149088067));
#33969=CARTESIAN_POINT('Ctrl Pts',(-0.114638169553469,-0.196557564679025,
1.20372869786351));
#33970=CARTESIAN_POINT('Ctrl Pts',(0.102965717368131,-0.202915862361653,
1.21484248692031));
#33971=CARTESIAN_POINT('Ctrl Pts',(0.226323915472005,-0.0235429700022985,
1.22595627597712));
#33972=CARTESIAN_POINT('Ctrl Pts',(0.142525267056592,0.177379069795616,
1.23707006503392));
#33973=CARTESIAN_POINT('Ctrl Pts',(-0.071728374642188,0.215944035394125,
1.24818385409072));
#33974=CARTESIAN_POINT('Ctrl Pts',(-0.220328221575874,0.0568529764244717,
1.25929764314753));
#33975=CARTESIAN_POINT('Ctrl Pts',(-0.16725914860919,-0.154276256623111,
1.27041143220433));
#33976=CARTESIAN_POINT('Ctrl Pts',(0.0389041199272518,-0.224194682371805,
1.28152522126113));
#33977=CARTESIAN_POINT('Ctrl Pts',(0.209458006291536,-0.088905172804972,
1.29263901031794));
#33978=CARTESIAN_POINT('Ctrl Pts',(0.188292604081856,0.127760249683509,
1.30375279937474));
#33979=CARTESIAN_POINT('Ctrl Pts',(-0.0052191540273722,0.227485266736855,
1.31486658843155));
#33980=CARTESIAN_POINT('Ctrl Pts',(-0.193953761266,0.118990439287648,1.32598037748835));
#33981=CARTESIAN_POINT('Ctrl Pts',(-0.205160291232821,-0.0984176866850601,
1.33709416654516));
#33982=CARTESIAN_POINT('Ctrl Pts',(-0.028581279957875,-0.225742987902158,
1.34820795560196));
#33983=CARTESIAN_POINT('Ctrl Pts',(0.174158500995476,-0.146443172193371,
1.35932174465876));
#33984=CARTESIAN_POINT('Ctrl Pts',(0.217489030897462,0.0668977398036206,
1.37043553371557));
#33985=CARTESIAN_POINT('Ctrl Pts',(0.0617493843227067,0.219006391884312,
1.38154932277237));
#33986=CARTESIAN_POINT('Ctrl Pts',(-0.150510174002661,0.17065600977586,
1.39266311182918));
#33987=CARTESIAN_POINT('Ctrl Pts',(-0.225006063172667,-0.0338977534588365,
1.40377690088598));
#33988=CARTESIAN_POINT('Ctrl Pts',(-0.0935513509578539,-0.207424518511403,
1.41489068994279));
#33989=CARTESIAN_POINT('Ctrl Pts',(0.123531973693776,-0.191093269444383,
1.42600447899959));
#33990=CARTESIAN_POINT('Ctrl Pts',(0.22754508195105,0.000147816343643338,
1.43711826805639));
#33991=CARTESIAN_POINT('Ctrl Pts',(0.123283596017355,0.191253604053547,
1.4482320571132));
#33992=CARTESIAN_POINT('Ctrl Pts',(-0.0938207632055154,0.207302799206008,
1.45934584617));
#33993=CARTESIAN_POINT('Ctrl Pts',(-0.225049914396199,0.033605390895932,
1.4704596352268));
#33994=CARTESIAN_POINT('Ctrl Pts',(-0.150288325686177,-0.170851412092914,
1.48157342428361));
#33995=CARTESIAN_POINT('Ctrl Pts',(0.0620338699676892,-0.218925981383812,
1.49268721334041));
#33996=CARTESIAN_POINT('Ctrl Pts',(0.217575764647534,-0.066615114486764,
1.50380100239722));
#33997=CARTESIAN_POINT('Ctrl Pts',(0.173968087346094,0.146669317115412,
1.51491479145402));
#33998=CARTESIAN_POINT('Ctrl Pts',(-0.0288745395963744,0.225705669091897,
1.52602858051083));
#33999=CARTESIAN_POINT('Ctrl Pts',(-0.205287999105225,0.0981510439482811,
1.53714236956763));
#34000=CARTESIAN_POINT('Ctrl Pts',(-0.1937989748928,-0.119242309357106,
1.54825615862444));
#34001=CARTESIAN_POINT('Ctrl Pts',(-0.00492364691005069,-0.227491892537031,
1.55936994768124));
#34002=CARTESIAN_POINT('Ctrl Pts',(0.188458534340702,-0.127515436462881,
1.57048373673804));
#34003=CARTESIAN_POINT('Ctrl Pts',(0.209342130614232,0.0891770956278107,
1.58159752579485));
#34004=CARTESIAN_POINT('Ctrl Pts',(0.0386131732285934,0.224245297773695,
1.59271131485165));
#34005=CARTESIAN_POINT('Ctrl Pts',(-0.167460147509052,0.154058322275268,
1.60382510390846));
#34006=CARTESIAN_POINT('Ctrl Pts',(-0.220252829642796,-0.057138233464333,
1.61493889296526));
#34007=CARTESIAN_POINT('Ctrl Pts',(-0.0714503221602304,-0.21603886592994,
1.62605268202207));
#34008=CARTESIAN_POINT('Ctrl Pts',(0.14276052028949,-0.177190259579807,
1.63716647107887));
#34009=CARTESIAN_POINT('Ctrl Pts',(0.226283718655826,0.0238303165896214,
1.64828026013567));
#34010=CARTESIAN_POINT('Ctrl Pts',(0.102720035411913,0.203062259110174,
1.65939404919248));
#34011=CARTESIAN_POINT('Ctrl Pts',(-0.114928016442956,0.196383949416646,
1.67050783824928));
#34012=CARTESIAN_POINT('Ctrl Pts',(-0.227259161518541,0.0100395986945998,
1.68162162730609));
#34013=CARTESIAN_POINT('Ctrl Pts',(-0.131813585150871,-0.185660673640335,
1.69273541636289));
#34014=CARTESIAN_POINT('Ctrl Pts',(0.0847577191513361,-0.211094895184898,
1.70384920541969));
#34015=CARTESIAN_POINT('Ctrl Pts',(0.176682876451709,-0.0997192257060721,
1.71125839812423));
#34016=CARTESIAN_POINT('Ctrl Pts',(0.188949368338152,-0.0368890654402894,
1.7149629944765));
#34017=CARTESIAN_POINT('Ctrl Pts',(0.0463299576986758,-0.173478327433381,
0.785037005523502));
#34018=CARTESIAN_POINT('Ctrl Pts',(0.104015628792176,-0.158072514262811,
0.78874160187577));
#34019=CARTESIAN_POINT('Ctrl Pts',(0.201813391703176,-0.0654583675678116,
0.796150794580307));
#34020=CARTESIAN_POINT('Ctrl Pts',(0.164387637044107,0.134450542830478,
0.80726458363711));
#34021=CARTESIAN_POINT('Ctrl Pts',(-0.0237796849449563,0.210832223234042,
0.818378372693916));
#34022=CARTESIAN_POINT('Ctrl Pts',(-0.190041204212204,0.0944671187531002,
0.829492161750717));
#34023=CARTESIAN_POINT('Ctrl Pts',(-0.182428515342129,-0.10848381527592,
0.840605950807524));
#34024=CARTESIAN_POINT('Ctrl Pts',(-0.00779904240022581,-0.212076280351327,
0.851719739864326));
#34025=CARTESIAN_POINT('Ctrl Pts',(0.173949198986102,-0.121585283079433,
0.862833528921132));
#34026=CARTESIAN_POINT('Ctrl Pts',(0.196490096226091,0.0802110005340724,
0.873947317977935));
#34027=CARTESIAN_POINT('Ctrl Pts',(0.0391759855426195,0.208580421784633,
0.885061107034741));
#34028=CARTESIAN_POINT('Ctrl Pts',(-0.153993531979477,0.146038425366231,
0.896174896091543));
#34029=CARTESIAN_POINT('Ctrl Pts',(-0.206212494327119,-0.0501766042094856,
0.907288685148349));
#34030=CARTESIAN_POINT('Ctrl Pts',(-0.0696820538212414,-0.200463162370631,
0.918402474205152));
#34031=CARTESIAN_POINT('Ctrl Pts',(0.130628759646036,-0.167264170775759,
0.929516263261957));
#34032=CARTESIAN_POINT('Ctrl Pts',(0.211373797459724,0.0190339558879606,
0.94063005231876));
#34033=CARTESIAN_POINT('Ctrl Pts',(0.098645891924909,0.187909907933315,
0.951743841375565));
#34034=CARTESIAN_POINT('Ctrl Pts',(-0.104373660084627,0.184789883644027,
0.962857630432369));
#34035=CARTESIAN_POINT('Ctrl Pts',(-0.21185884717154,0.0125295344009149,
0.973971419489173));
#34036=CARTESIAN_POINT('Ctrl Pts',(-0.125427213221957,-0.17119921429325,
0.985085208545978));
#34037=CARTESIAN_POINT('Ctrl Pts',(0.0758093632963375,-0.198227393919747,
0.996198997602781));
#34038=CARTESIAN_POINT('Ctrl Pts',(0.207656774100798,-0.0438157848914807,
1.00731278665959));
#34039=CARTESIAN_POINT('Ctrl Pts',(0.149433582364513,0.150700905324243,
1.01842657571639));
#34040=CARTESIAN_POINT('Ctrl Pts',(-0.0455678608436973,0.207279349727,1.0295403647732));
#34041=CARTESIAN_POINT('Ctrl Pts',(-0.198860524851901,0.0741326536274474,
1.04065415383));
#34042=CARTESIAN_POINT('Ctrl Pts',(-0.170133894915531,-0.126868500542071,
1.0517679428868));
#34043=CARTESIAN_POINT('Ctrl Pts',(0.0143182183216636,-0.211745477648606,
1.06288173194361));
#34044=CARTESIAN_POINT('Ctrl Pts',(0.185664704035542,-0.102809417565425,
1.07399552100041));
#34045=CARTESIAN_POINT('Ctrl Pts',(0.187070180519752,0.100229268279905,
1.08510931005721));
#34046=CARTESIAN_POINT('Ctrl Pts',(0.017248199277583,0.211526968229848,
1.09622309911402));
#34047=CARTESIAN_POINT('Ctrl Pts',(-0.168361254383508,0.12921163525997,
1.10733688817082));
#34048=CARTESIAN_POINT('Ctrl Pts',(-0.199867742554481,-0.07137257281249,
1.11845067722763));
#34049=CARTESIAN_POINT('Ctrl Pts',(-0.0484330193143192,-0.206628655575122,
1.12956446628443));
#34050=CARTESIAN_POINT('Ctrl Pts',(0.147332995773784,-0.152755186558655,
1.14067825534124));
#34051=CARTESIAN_POINT('Ctrl Pts',(0.208243448959415,0.0409368370750985,
1.15179204439804));
#34052=CARTESIAN_POINT('Ctrl Pts',(0.0785463116716341,0.197158909479484,
1.16290583345485));
#34053=CARTESIAN_POINT('Ctrl Pts',(-0.123045155465202,0.172919196102783,
1.17401962251165));
#34054=CARTESIAN_POINT('Ctrl Pts',(-0.212011996377637,-0.00959541850364452,
1.18513341156845));
#34055=CARTESIAN_POINT('Ctrl Pts',(-0.106921852626119,-0.18332723773435,
1.19624720062526));
#34056=CARTESIAN_POINT('Ctrl Pts',(0.0960350754104022,-0.189257557194465,
1.20736098968206));
#34057=CARTESIAN_POINT('Ctrl Pts',(0.211090009811934,-0.0219582882278384,
1.21847477873886));
#34058=CARTESIAN_POINT('Ctrl Pts',(0.132931864309081,0.16543965097767,1.22958856779567));
#34059=CARTESIAN_POINT('Ctrl Pts',(-0.0669003241457547,0.201408801430058,
1.24070235685247));
#34060=CARTESIAN_POINT('Ctrl Pts',(-0.205497887208699,0.0530261918023587,
1.25181614590928));
#34061=CARTESIAN_POINT('Ctrl Pts',(-0.156000903604979,-0.143891892539961,
1.26292993496608));
#34062=CARTESIAN_POINT('Ctrl Pts',(0.0362854762389619,-0.209104095795397,
1.27404372402289));
#34063=CARTESIAN_POINT('Ctrl Pts',(0.195359348176077,-0.0829209487675844,
1.28515751307969));
#34064=CARTESIAN_POINT('Ctrl Pts',(0.175618593201963,0.119160683054738,
1.2962713021365));
#34065=CARTESIAN_POINT('Ctrl Pts',(-0.00486785178026968,0.212173190302961,
1.3073850911933));
#34066=CARTESIAN_POINT('Ctrl Pts',(-0.180898696822721,0.110981170259326,
1.3184988802501));
#34067=CARTESIAN_POINT('Ctrl Pts',(-0.191350913132785,-0.0917931735348885,
1.32961266930691));
#34068=CARTESIAN_POINT('Ctrl Pts',(-0.026657468585072,-0.210548184586953,
1.34072645836371));
#34069=CARTESIAN_POINT('Ctrl Pts',(0.162435859274068,-0.136586054508292,
1.35184024742051));
#34070=CARTESIAN_POINT('Ctrl Pts',(0.202849802993145,0.0623948402540306,
1.36295403647732));
#34071=CARTESIAN_POINT('Ctrl Pts',(0.057593021556634,0.204265030124287,
1.37406782553412));
#34072=CARTESIAN_POINT('Ctrl Pts',(-0.14037930565472,0.159169121402496,
1.38518161459093));
#34073=CARTESIAN_POINT('Ctrl Pts',(-0.209860862400721,-0.0316160892467124,
1.39629540364773));
#34074=CARTESIAN_POINT('Ctrl Pts',(-0.0872543917881084,-0.193462734843961,
1.40740919270454));
#34075=CARTESIAN_POINT('Ctrl Pts',(0.11521701312353,-0.178230745247949,
1.41852298176134));
#34076=CARTESIAN_POINT('Ctrl Pts',(0.212228979343748,0.000137866797527619,
1.42963677081814));
#34077=CARTESIAN_POINT('Ctrl Pts',(0.1149853537956,0.178380287704172,1.44075055987495));
#34078=CARTESIAN_POINT('Ctrl Pts',(-0.0875056698463009,0.19334920848809,
1.45186434893175));
#34079=CARTESIAN_POINT('Ctrl Pts',(-0.209901761990083,0.0313434056633472,
1.46297813798856));
#34080=CARTESIAN_POINT('Ctrl Pts',(-0.14017238999048,-0.159351371152542,
1.47409192704536));
#34081=CARTESIAN_POINT('Ctrl Pts',(0.0578583584189162,-0.204190032069821,
1.48520571610217));
#34082=CARTESIAN_POINT('Ctrl Pts',(0.202930698678054,-0.0621312385008357,
1.49631950515897));
#34083=CARTESIAN_POINT('Ctrl Pts',(0.162258262403527,0.136796977572755,
1.50743329421577));
#34084=CARTESIAN_POINT('Ctrl Pts',(-0.0269309888617035,0.210513377712887,
1.51854708327258));
#34085=CARTESIAN_POINT('Ctrl Pts',(-0.191470024964085,0.0915444785712757,
1.52966087232938));
#34086=CARTESIAN_POINT('Ctrl Pts',(-0.180754329149647,-0.111216086906656,
1.54077466138619));
#34087=CARTESIAN_POINT('Ctrl Pts',(-0.00459223530304152,-0.212179370119272,
1.55188845044299));
#34088=CARTESIAN_POINT('Ctrl Pts',(0.175773354663627,-0.118932348258406,
1.5630022394998));
#34089=CARTESIAN_POINT('Ctrl Pts',(0.195251272112581,0.0831745684136627,
1.5741160285566));
#34090=CARTESIAN_POINT('Ctrl Pts',(0.0360141132177518,0.20915130426499,
1.5852298176134));
#34091=CARTESIAN_POINT('Ctrl Pts',(-0.156188373230783,0.14368862739439,
1.59634360667021));
#34092=CARTESIAN_POINT('Ctrl Pts',(-0.20542756992093,-0.0532922481367839,
1.60745739572701));
#34093=CARTESIAN_POINT('Ctrl Pts',(-0.0666409874290749,-0.201497248904528,
1.61857118478382));
#34094=CARTESIAN_POINT('Ctrl Pts',(0.13315128260227,-0.165263549613285,
1.62968497384062));
#34095=CARTESIAN_POINT('Ctrl Pts',(0.211052518651072,0.0222262934618894,
1.64079876289742));
#34096=CARTESIAN_POINT('Ctrl Pts',(0.095805930353238,0.189394099950088,
1.65191255195423));
#34097=CARTESIAN_POINT('Ctrl Pts',(-0.107192189866521,0.183165308548198,
1.66302634101103));
#34098=CARTESIAN_POINT('Ctrl Pts',(-0.21196230426976,0.00936383140301889,
1.67414013006784));
#34099=CARTESIAN_POINT('Ctrl Pts',(-0.122941187743304,-0.173163818497459,
1.68525391912464));
#34100=CARTESIAN_POINT('Ctrl Pts',(0.0790526610057068,-0.196886057767682,
1.69636770818145));
#34101=CARTESIAN_POINT('Ctrl Pts',(0.164790318539736,-0.0930071057176319,
1.70377690088598));
#34102=CARTESIAN_POINT('Ctrl Pts',(0.176231150531649,-0.034406055451559,
1.70748149723825));
#34103=CARTESIAN_POINT('Ctrl Pts',(0.0429864256885843,-0.160958774866485,
0.777555508285253));
#34104=CARTESIAN_POINT('Ctrl Pts',(0.0965090477009877,-0.146664765635222,
0.781260104637521));
#34105=CARTESIAN_POINT('Ctrl Pts',(0.187248959341434,-0.0607343799329692,
0.788669297342056));
#34106=CARTESIAN_POINT('Ctrl Pts',(0.1525241397775,0.124747540366033,0.799783086398862));
#34107=CARTESIAN_POINT('Ctrl Pts',(-0.0220635569415495,0.195616921469113,
0.810896875455666));
#34108=CARTESIAN_POINT('Ctrl Pts',(-0.176326344948735,0.0876496328079073,
0.82201066451247));
#34109=CARTESIAN_POINT('Ctrl Pts',(-0.169263047232554,-0.100654774910484,
0.833124453569274));
#34110=CARTESIAN_POINT('Ctrl Pts',(-0.00723620251846265,-0.196771197697301,
0.844238242626078));
#34111=CARTESIAN_POINT('Ctrl Pts',(0.161395664646129,-0.112810738354482,
0.855352031682883));
#34112=CARTESIAN_POINT('Ctrl Pts',(0.182309834489814,0.0744223475508041,
0.866465820739686));
#34113=CARTESIAN_POINT('Ctrl Pts',(0.0363487401015477,0.193527627619547,
0.877579609796491));
#34114=CARTESIAN_POINT('Ctrl Pts',(-0.142880154607774,0.135499150690198,
0.888693398853294));
#34115=CARTESIAN_POINT('Ctrl Pts',(-0.191330588322633,-0.0465554681095297,
0.8998071879101));
#34116=CARTESIAN_POINT('Ctrl Pts',(-0.0646532519605634,-0.185996173115221,
0.910920976966903));
#34117=CARTESIAN_POINT('Ctrl Pts',(0.121201566939414,-0.155193080342923,
0.922034766023707));
#34118=CARTESIAN_POINT('Ctrl Pts',(0.196119411464,0.0176603168010446,0.933148555080512));
#34119=CARTESIAN_POINT('Ctrl Pts',(0.0915268330330338,0.174348859674332,
0.944262344137316));
#34120=CARTESIAN_POINT('Ctrl Pts',(-0.0968412406558618,0.17145400073381,
0.95537613319412));
#34121=CARTESIAN_POINT('Ctrl Pts',(-0.196569456195918,0.0116253052277854,
0.966489922250924));
#34122=CARTESIAN_POINT('Ctrl Pts',(-0.116375404777155,-0.158844140351355,
0.977603711307728));
#34123=CARTESIAN_POINT('Ctrl Pts',(0.0703383668733642,-0.183921755197642,
0.988717500364533));
#34124=CARTESIAN_POINT('Ctrl Pts',(0.19267063757475,-0.0406536952499414,
0.999831289421336));
#34125=CARTESIAN_POINT('Ctrl Pts',(0.13864928661212,0.139825149637642,1.01094507847814));
#34126=CARTESIAN_POINT('Ctrl Pts',(-0.0422793277016381,0.192320451094917,
1.02205886753494));
#34127=CARTESIAN_POINT('Ctrl Pts',(-0.184509194451163,0.0687826616846859,
1.03317265659175));
#34128=CARTESIAN_POINT('Ctrl Pts',(-0.157855702749863,-0.117712677534557,
1.04428644564855));
#34129=CARTESIAN_POINT('Ctrl Pts',(0.0132849037307607,-0.196464268304215,
1.05540023470536));
#34130=CARTESIAN_POINT('Ctrl Pts',(0.172265687245489,-0.0953898861079487,
1.06651402376216));
#34131=CARTESIAN_POINT('Ctrl Pts',(0.173569733556916,0.0929959405695393,
1.07762781281897));
#34132=CARTESIAN_POINT('Ctrl Pts',(0.0160034343508349,0.196261528233681,
1.08874160187577));
#34133=CARTESIAN_POINT('Ctrl Pts',(-0.156210989819237,0.119886713329805,
1.09985539093257));
#34134=CARTESIAN_POINT('Ctrl Pts',(-0.185443723448703,-0.066221769882921,
1.11096917998938));
#34135=CARTESIAN_POINT('Ctrl Pts',(-0.0449377139338128,-0.191716716120937,
1.12208296904618));
#34136=CARTESIAN_POINT('Ctrl Pts',(0.136700294774655,-0.141731177875371,
1.13319675810299));
#34137=CARTESIAN_POINT('Ctrl Pts',(0.193214973388251,0.0379825148190173,
1.14431054715979));
#34138=CARTESIAN_POINT('Ctrl Pts',(0.0728777956531908,0.182930380949266,
1.1554243362166));
#34139=CARTESIAN_POINT('Ctrl Pts',(-0.11416525493388,0.160439994824655,
1.1665381252734));
#34140=CARTESIAN_POINT('Ctrl Pts',(-0.196711552957801,-0.00890293807605981,
1.1776519143302));
#34141=CARTESIAN_POINT('Ctrl Pts',(-0.0992055356987686,-0.170096910789675,
1.18876570338701));
#34142=CARTESIAN_POINT('Ctrl Pts',(0.0891044334526734,-0.175599252027278,
1.19987949244381));
#34143=CARTESIAN_POINT('Ctrl Pts',(0.195856104151863,-0.0203736064533785,
1.21099328150062));
#34144=CARTESIAN_POINT('Ctrl Pts',(0.12333846156157,0.153500232159725,1.22210707055742));
#34145=CARTESIAN_POINT('Ctrl Pts',(-0.0620722736493212,0.186873567465992,
1.23322085961422));
#34146=CARTESIAN_POINT('Ctrl Pts',(-0.190667552841524,0.0491994071802457,
1.24433464867103));
#34147=CARTESIAN_POINT('Ctrl Pts',(-0.144742658600767,-0.13350752845681,
1.25544843772783));
#34148=CARTESIAN_POINT('Ctrl Pts',(0.0336668325506717,-0.194013509218991,
1.26656222678464));
#34149=CARTESIAN_POINT('Ctrl Pts',(0.181260690060617,-0.0769367247301966,
1.27767601584144));
#34150=CARTESIAN_POINT('Ctrl Pts',(0.16294458232207,0.110561116425968,1.28878980489824));
#34151=CARTESIAN_POINT('Ctrl Pts',(-0.00451654953316709,0.196861113869068,
1.29990359395505));
#34152=CARTESIAN_POINT('Ctrl Pts',(-0.167843632379442,0.102971901231004,
1.31101738301185));
#34153=CARTESIAN_POINT('Ctrl Pts',(-0.177541535032749,-0.0851686603847167,
1.32213117206866));
#34154=CARTESIAN_POINT('Ctrl Pts',(-0.0247336572122691,-0.195353381271748,
1.33324496112546));
#34155=CARTESIAN_POINT('Ctrl Pts',(0.15071321755266,-0.126728936823214,
1.34435875018226));
#34156=CARTESIAN_POINT('Ctrl Pts',(0.188210575088826,0.0578919407044404,
1.35547253923907));
#34157=CARTESIAN_POINT('Ctrl Pts',(0.0534366587905616,0.189523668364262,
1.36658632829587));
#34158=CARTESIAN_POINT('Ctrl Pts',(-0.130248437306779,0.147682233029131,
1.37770011735268));
#34159=CARTESIAN_POINT('Ctrl Pts',(-0.194715661628775,-0.0293344250345881,
1.38881390640948));
#34160=CARTESIAN_POINT('Ctrl Pts',(-0.0809574326183627,-0.17950095117652,
1.39992769546629));
#34161=CARTESIAN_POINT('Ctrl Pts',(0.106902052553284,-0.165368221051515,
1.41104148452309));
#34162=CARTESIAN_POINT('Ctrl Pts',(0.196912876736446,0.000127917251411783,
1.4221552735799));
#34163=CARTESIAN_POINT('Ctrl Pts',(0.106687111573845,0.165506971354797,
1.4332690626367));
#34164=CARTESIAN_POINT('Ctrl Pts',(-0.0811905764870862,0.179395617770172,
1.44438285169351));
#34165=CARTESIAN_POINT('Ctrl Pts',(-0.194753609583967,0.0290814204307625,
1.45549664075031));
#34166=CARTESIAN_POINT('Ctrl Pts',(-0.130056454294782,-0.14785133021217,
1.46661042980711));
#34167=CARTESIAN_POINT('Ctrl Pts',(0.053682846870143,-0.189454082755829,
1.47772421886392));
#34168=CARTESIAN_POINT('Ctrl Pts',(0.188285632708575,-0.0576473625149073,
1.48883800792072));
#34169=CARTESIAN_POINT('Ctrl Pts',(0.15054843746096,0.126924638030098,1.49995179697752));
#34170=CARTESIAN_POINT('Ctrl Pts',(-0.024987438127033,0.195321086333876,
1.51106558603433));
#34171=CARTESIAN_POINT('Ctrl Pts',(-0.177652050822945,0.0849379131942705,
1.52217937509113));
#34172=CARTESIAN_POINT('Ctrl Pts',(-0.167709683406495,-0.103189864456206,
1.53329316414794));
#34173=CARTESIAN_POINT('Ctrl Pts',(-0.00426082369603206,-0.196866847701512,
1.54440695320474));
#34174=CARTESIAN_POINT('Ctrl Pts',(0.163088174986552,-0.110349260053931,
1.55552074226154));
#34175=CARTESIAN_POINT('Ctrl Pts',(0.181160413610931,0.0771720411995148,
1.56663453131835));
#34176=CARTESIAN_POINT('Ctrl Pts',(0.03341505320691,0.194057310756286,1.57774832037515));
#34177=CARTESIAN_POINT('Ctrl Pts',(-0.144916598952513,0.133318932513512,
1.58886210943196));
#34178=CARTESIAN_POINT('Ctrl Pts',(-0.190602310199064,-0.049446262809235,
1.59997589848876));
#34179=CARTESIAN_POINT('Ctrl Pts',(-0.0618316526979189,-0.186955631879117,
1.61108968754557));
#34180=CARTESIAN_POINT('Ctrl Pts',(0.12354204491505,-0.153336839646763,
1.62220347660237));
#34181=CARTESIAN_POINT('Ctrl Pts',(0.195821318646319,0.0206222703341576,
1.63331726565918));
#34182=CARTESIAN_POINT('Ctrl Pts',(0.0888918252945621,0.175725940790001,
1.64443105471598));
#34183=CARTESIAN_POINT('Ctrl Pts',(-0.0994563632900866,0.16994666767975,
1.65554484377278));
#34184=CARTESIAN_POINT('Ctrl Pts',(-0.19666544702098,0.008688064111438,
1.66665863282959));
#34185=CARTESIAN_POINT('Ctrl Pts',(-0.114068790335738,-0.160666963354583,
1.67777242188639));
#34186=CARTESIAN_POINT('Ctrl Pts',(0.0733476028600775,-0.182677220350466,
1.6888862109432));
#34187=CARTESIAN_POINT('Ctrl Pts',(0.152897760627763,-0.0862949857291919,
1.69629540364773));
#34188=CARTESIAN_POINT('Ctrl Pts',(0.163512932725146,-0.0319230454628286,
1.7));
#34189=CARTESIAN_POINT('Ctrl Pts',(0.166381444272219,9.40568719243839E-5,
0.86214803633902));
#34190=CARTESIAN_POINT('Ctrl Pts',(0.166493197029431,0.0216823422355625,
0.863587297805909));
#34191=CARTESIAN_POINT('Ctrl Pts',(0.162594223870085,0.0432319486948127,
0.865026559272798));
#34192=CARTESIAN_POINT('Ctrl Pts',(0.154497290451155,0.0630677132447136,
0.866465820739686));
#34193=CARTESIAN_POINT('Ctrl Pts',(0.133656136360392,0.114124107573719,
0.870170417091954));
#34194=CARTESIAN_POINT('Ctrl Pts',(0.0850024382309698,0.153825867596633,
0.873875013444223));
#34195=CARTESIAN_POINT('Ctrl Pts',(0.0308041067147051,0.164005334786532,
0.877579609796491));
#34196=CARTESIAN_POINT('Ctrl Pts',(-0.0233942248015594,0.174184801976431,
0.881284206148759));
#34197=CARTESIAN_POINT('Ctrl Pts',(-0.0831371897046666,0.154841976333314,
0.884988802501027));
#34198=CARTESIAN_POINT('Ctrl Pts',(-0.12108374444203,0.114828127045135,
0.888693398853295));
#34199=CARTESIAN_POINT('Ctrl Pts',(-0.159030299179393,0.0748142777569551,
0.892397995205563));
#34200=CARTESIAN_POINT('Ctrl Pts',(-0.175180443751013,0.0141294048237127,
0.896102591557831));
#34201=CARTESIAN_POINT('Ctrl Pts',(-0.162142626643145,-0.039453149143857,
0.899807187910099));
#34202=CARTESIAN_POINT('Ctrl Pts',(-0.149104809535276,-0.0930357031114267,
0.903511784262367));
#34203=CARTESIAN_POINT('Ctrl Pts',(-0.10687903074792,-0.139515938113324,
0.907216380614635));
#34204=CARTESIAN_POINT('Ctrl Pts',(-0.0547903382042454,-0.157622206818889,
0.910920976966903));
#34205=CARTESIAN_POINT('Ctrl Pts',(-0.00270164566057092,-0.175728475524455,
0.914625573319171));
#34206=CARTESIAN_POINT('Ctrl Pts',(0.0592499606394216,-0.165460777933689,
0.918330169671439));
#34207=CARTESIAN_POINT('Ctrl Pts',(0.102712071210182,-0.131518029614312,
0.922034766023707));
#34208=CARTESIAN_POINT('Ctrl Pts',(0.142261505739626,-0.100630976850939,
0.925405856128812));
#34209=CARTESIAN_POINT('Ctrl Pts',(0.166500629757864,-0.0501396913203886,
0.928776946233916));
#34210=CARTESIAN_POINT('Ctrl Pts',(0.16681765906064,8.64047405809373E-5,
0.93214803633902));
#34211=CARTESIAN_POINT('Ctrl Pts',(0.0530170217188587,-0.198517432567173,
0.8));
#34212=CARTESIAN_POINT('Ctrl Pts',(0.0654219024915668,-0.193924365121538,
0.8));
#34213=CARTESIAN_POINT('Ctrl Pts',(0.0772726753754473,-0.188065368475528,
0.8));
#34214=CARTESIAN_POINT('Ctrl Pts',(0.0884514733522922,-0.181103303150236,
0.8));
#34215=CARTESIAN_POINT('Ctrl Pts',(0.09412650504638,-0.177568939128346,
0.8));
#34216=CARTESIAN_POINT('Ctrl Pts',(0.0996279181736098,-0.173749544851002,
0.8));
#34217=CARTESIAN_POINT('Ctrl Pts',(0.104936837602987,-0.16966283510169,
0.8));
#34218=CARTESIAN_POINT('Ctrl Pts',(0.10962098777257,-0.166057061380704,
0.8));
#34219=CARTESIAN_POINT('Ctrl Pts',(0.114155265023366,-0.162243133727946,
0.8));
#34220=CARTESIAN_POINT('Ctrl Pts',(0.118524756406352,-0.158232269033094,
0.8));
#34221=CARTESIAN_POINT('Ctrl Pts',(0.121396569737292,-0.155596160230106,
0.8));
#34222=CARTESIAN_POINT('Ctrl Pts',(0.124191187364035,-0.152880333162932,
0.8));
#34223=CARTESIAN_POINT('Ctrl Pts',(0.126901910586196,-0.150092210881471,
0.8));
#34224=CARTESIAN_POINT('Ctrl Pts',(0.135875513595552,-0.140862385316535,
0.8));
#34225=CARTESIAN_POINT('Ctrl Pts',(0.143945927205397,-0.130830324459656,
0.8));
#34226=CARTESIAN_POINT('Ctrl Pts',(0.150974563153614,-0.120127060905897,
0.8));
#34227=CARTESIAN_POINT('Ctrl Pts',(0.155531899783608,-0.113187111901085,
0.8));
#34228=CARTESIAN_POINT('Ctrl Pts',(0.159650421905677,-0.105964391211092,
0.8));
#34229=CARTESIAN_POINT('Ctrl Pts',(0.163280590687062,-0.0984918775736134,
0.8));
#34230=CARTESIAN_POINT('Ctrl Pts',(0.165013714615195,-0.0949243321044268,
0.8));
#34231=CARTESIAN_POINT('Ctrl Pts',(0.166631773157808,-0.0913069558365289,
0.8));
#34232=CARTESIAN_POINT('Ctrl Pts',(0.168128066663937,-0.0876495022602451,
0.8));
#34233=CARTESIAN_POINT('Ctrl Pts',(0.172146949722996,-0.0778259762228617,
0.8));
#34234=CARTESIAN_POINT('Ctrl Pts',(0.175295994023174,-0.0677004884915743,
0.8));
#34235=CARTESIAN_POINT('Ctrl Pts',(0.177480263226672,-0.0573468152173212,
0.8));
#34236=CARTESIAN_POINT('Ctrl Pts',(0.179333801272362,-0.048560843554235,
0.8));
#34237=CARTESIAN_POINT('Ctrl Pts',(0.180491858406323,-0.0396100717078052,
0.8));
#34238=CARTESIAN_POINT('Ctrl Pts',(0.18096708784323,-0.0305729202789466,
0.8));
#34239=CARTESIAN_POINT('Ctrl Pts',(0.181136159028966,-0.0273577955642423,
0.8));
#34240=CARTESIAN_POINT('Ctrl Pts',(0.181218443079545,-0.0241331712280784,
0.8));
#34241=CARTESIAN_POINT('Ctrl Pts',(0.181214870924098,-0.0209122942089756,
0.8));
#34242=CARTESIAN_POINT('Ctrl Pts',(0.1812018830209,-0.00920159472786908,
0.8));
#34243=CARTESIAN_POINT('Ctrl Pts',(0.180059445076844,0.00249593154933228,
0.8));
#34244=CARTESIAN_POINT('Ctrl Pts',(0.177833010924532,0.0140076329059244,
0.8));
#34245=CARTESIAN_POINT('Ctrl Pts',(0.176687470499003,0.019930610352574,
0.8));
#34246=CARTESIAN_POINT('Ctrl Pts',(0.17525426981669,0.0258042115192748,
0.8));
#34247=CARTESIAN_POINT('Ctrl Pts',(0.173535645755736,0.0316026384872638,
0.8));
#34248=CARTESIAN_POINT('Ctrl Pts',(0.171850920647243,0.0372866945438873,
0.8));
#34249=CARTESIAN_POINT('Ctrl Pts',(0.169889181319091,0.0429039115259332,
0.8));
#34250=CARTESIAN_POINT('Ctrl Pts',(0.167664346683561,0.0483972355746533,
0.8));
#34251=CARTESIAN_POINT('Ctrl Pts',(0.16420912784319,0.0569284928853236,
0.8));
#34252=CARTESIAN_POINT('Ctrl Pts',(0.160117674787075,0.065174591642692,
0.8));
#34253=CARTESIAN_POINT('Ctrl Pts',(0.155399354804051,0.073039643321633,
0.8));
#34254=CARTESIAN_POINT('Ctrl Pts',(0.15298274940935,0.0770679259275847,
0.8));
#34255=CARTESIAN_POINT('Ctrl Pts',(0.150400765188628,0.0809963604120499,
0.8));
#34256=CARTESIAN_POINT('Ctrl Pts',(0.147663479517856,0.0847983168718068,
0.8));
#34257=CARTESIAN_POINT('Ctrl Pts',(0.142228073022467,0.0923478317277872,
0.8));
#34258=CARTESIAN_POINT('Ctrl Pts',(0.136173701728632,0.0994134091821942,
0.8));
#34259=CARTESIAN_POINT('Ctrl Pts',(0.129505054411736,0.105883695181419,
0.8));
#34260=CARTESIAN_POINT('Ctrl Pts',(0.128726565799248,0.106639027369579,
0.8));
#34261=CARTESIAN_POINT('Ctrl Pts',(0.127939691591626,0.107386221438147,
0.8));
#34262=CARTESIAN_POINT('Ctrl Pts',(0.127144588893496,0.108125211870903,
0.8));
#34263=CARTESIAN_POINT('Origin',(0.,0.,1.3));
#34264=CARTESIAN_POINT('Origin',(0.,0.,1.8));
#34265=CARTESIAN_POINT('Origin',(0.4,0.6,0.8));
#34266=CARTESIAN_POINT('',(0.4,0.6,0.8));
#34267=CARTESIAN_POINT('',(-0.4,0.6,0.8));
#34268=CARTESIAN_POINT('',(0.4,0.6,0.8));
#34269=CARTESIAN_POINT('',(-0.4,0.6,3.6));
#34270=CARTESIAN_POINT('',(-0.4,0.6,0.8));
#34271=CARTESIAN_POINT('',(0.4,0.6,3.6));
#34272=CARTESIAN_POINT('',(0.4,0.6,3.6));
#34273=CARTESIAN_POINT('',(0.4,0.6,0.8));
#34274=CARTESIAN_POINT('Origin',(0.4,-0.6,0.8));
#34275=CARTESIAN_POINT('',(0.4,-0.6,0.8));
#34276=CARTESIAN_POINT('',(0.4,-0.6,0.8));
#34277=CARTESIAN_POINT('',(0.4,-0.6,3.6));
#34278=CARTESIAN_POINT('',(0.4,-0.6,3.6));
#34279=CARTESIAN_POINT('',(0.4,-0.6,0.8));
#34280=CARTESIAN_POINT('Origin',(-0.4,-0.6,0.8));
#34281=CARTESIAN_POINT('',(-0.4,-0.6,0.8));
#34282=CARTESIAN_POINT('',(-0.4,-0.6,0.8));
#34283=CARTESIAN_POINT('',(-0.4,-0.6,3.6));
#34284=CARTESIAN_POINT('',(-0.4,-0.6,3.6));
#34285=CARTESIAN_POINT('',(-0.4,-0.6,0.8));
#34286=CARTESIAN_POINT('Origin',(-0.4,0.6,0.8));
#34287=CARTESIAN_POINT('',(-0.4,0.6,0.8));
#34288=CARTESIAN_POINT('',(-0.4,0.6,3.6));
#34289=CARTESIAN_POINT('Origin',(0.,0.,3.6));
#34290=CARTESIAN_POINT('Origin',(0.,0.,0.8));
#34291=CARTESIAN_POINT('',(0.,0.,0.));
#34292=CARTESIAN_POINT('Origin',(0.,0.,3.7));
#34293=CARTESIAN_POINT('',(-0.126245375007135,3.12536796039931E-5,3.51934196736194));
#34294=CARTESIAN_POINT('',(-0.126365398388193,-0.00016976464794081,3.50565803263806));
#34295=CARTESIAN_POINT('',(-0.12645,1.54856587752183E-17,3.7));
#34296=CARTESIAN_POINT('',(-0.0958116152722475,0.0825211298936389,3.5));
#34297=CARTESIAN_POINT('Ctrl Pts',(-0.126365398388193,-0.00016976464794081,
3.50565803263806));
#34298=CARTESIAN_POINT('Ctrl Pts',(-0.126096583499468,0.0297434857833807,
3.5037720217587));
#34299=CARTESIAN_POINT('Ctrl Pts',(-0.115369380269343,0.0598134784363466,
3.50188601087935));
#34300=CARTESIAN_POINT('Ctrl Pts',(-0.0958116152722475,0.0825211298936389,
3.5));
#34301=CARTESIAN_POINT('',(-0.12645,1.54856587752183E-17,3.5));
#34302=CARTESIAN_POINT('Origin',(0.,0.,3.5));
#34303=CARTESIAN_POINT('',(-0.12645,-1.54856587752183E-17,3.4));
#34304=CARTESIAN_POINT('',(-0.12645,1.54856587752183E-17,3.7));
#34305=CARTESIAN_POINT('Origin',(0.,0.,3.4));
#34306=CARTESIAN_POINT('',(0.095993992990581,0.0826600147079878,3.5));
#34307=CARTESIAN_POINT('Origin',(0.,0.,3.5));
#34308=CARTESIAN_POINT('Ctrl Pts',(0.0959941578858439,0.0826601402795114,
3.5));
#34309=CARTESIAN_POINT('Ctrl Pts',(0.0693049284490514,0.113544181600847,
3.5025799450779));
#34310=CARTESIAN_POINT('Ctrl Pts',(0.0262885066473286,0.130447374694629,
3.5051598901558));
#34311=CARTESIAN_POINT('Ctrl Pts',(-0.0142676563835003,0.125842979166089,
3.5077398352337));
#34312=CARTESIAN_POINT('Ctrl Pts',(-0.0558709915822301,0.121119696778261,
3.51038639525932));
#34313=CARTESIAN_POINT('Ctrl Pts',(-0.0948853785622285,0.0937638222778825,
3.51303295528495));
#34314=CARTESIAN_POINT('Ctrl Pts',(-0.113475688700545,0.0562620506672719,
3.51567951531057));
#34315=CARTESIAN_POINT('Ctrl Pts',(-0.122051112249405,0.0389630614088429,
3.51690033266103));
#34316=CARTESIAN_POINT('Ctrl Pts',(-0.126280629837482,0.0195051929476654,
3.51812115001148));
#34317=CARTESIAN_POINT('Ctrl Pts',(-0.126245375007135,3.12536796039931E-5,
3.51934196736194));
#34318=CARTESIAN_POINT('Origin',(0.,0.,3.7));
#34319=CARTESIAN_POINT('',(-0.126440375727766,-0.00011573372396179,3.56934196736194));
#34320=CARTESIAN_POINT('',(-0.126657922659285,8.80032312977707E-6,3.55565803263806));
#34321=CARTESIAN_POINT('',(-0.12645,1.54856587752183E-17,3.7));
#34322=CARTESIAN_POINT('Ctrl Pts',(-0.126657922659285,8.80032312977707E-6,
3.55565803263806));
#34323=CARTESIAN_POINT('Ctrl Pts',(-0.126658305335383,0.00043204034557634,
3.55563127527141));
#34324=CARTESIAN_POINT('Ctrl Pts',(-0.126656367352663,0.000855276509828617,
3.55560451790477));
#34325=CARTESIAN_POINT('Ctrl Pts',(-0.126652098121077,0.00127848889899514,
3.55557776053813));
#34326=CARTESIAN_POINT('Ctrl Pts',(-0.126229830197349,0.0431382506048763,
3.5529312005125));
#34327=CARTESIAN_POINT('Ctrl Pts',(-0.103000707566798,0.0847654181274417,
3.55028464048688));
#34328=CARTESIAN_POINT('Ctrl Pts',(-0.0675987137490504,0.107109477361251,
3.54763808046125));
#34329=CARTESIAN_POINT('Ctrl Pts',(-0.0321967199313031,0.12945353659506,
3.54499152043563));
#34330=CARTESIAN_POINT('Ctrl Pts',(0.0153781450736419,0.132514487540114,
3.54234496041));
#34331=CARTESIAN_POINT('Ctrl Pts',(0.0533465621421041,0.114879483210429,
3.53969840038438));
#34332=CARTESIAN_POINT('Ctrl Pts',(0.0913149792105665,0.097244478880744,
3.53705184035875));
#34333=CARTESIAN_POINT('Ctrl Pts',(0.119676948342547,0.0589135192763201,
3.53440528033313));
#34334=CARTESIAN_POINT('Ctrl Pts',(0.125448844532432,0.0174567066922002,
3.5317587203075));
#34335=CARTESIAN_POINT('Ctrl Pts',(0.131220740722318,-0.0240001058919198,
3.52911216028188));
#34336=CARTESIAN_POINT('Ctrl Pts',(0.11440256397011,-0.0685827714557354,
3.52646560025625));
#34337=CARTESIAN_POINT('Ctrl Pts',(0.0826932442631274,-0.0959262477461666,
3.52381904023063));
#34338=CARTESIAN_POINT('Ctrl Pts',(0.0509839245561443,-0.123269724036598,
3.521172480205));
#34339=CARTESIAN_POINT('Ctrl Pts',(0.00438346189438567,-0.133374011053645,
3.51852592017938));
#34340=CARTESIAN_POINT('Ctrl Pts',(-0.0357753168513136,-0.121524408044806,
3.51587936015375));
#34341=CARTESIAN_POINT('Ctrl Pts',(-0.0759340955970119,-0.109674805035968,
3.51323280012813));
#34342=CARTESIAN_POINT('Ctrl Pts',(-0.109651190426652,-0.0758713120012468,
3.5105862401025));
#34343=CARTESIAN_POINT('Ctrl Pts',(-0.121481718337573,-0.0357885021759826,
3.50793968007688));
#34344=CARTESIAN_POINT('Ctrl Pts',(-0.124881489291372,-0.0242697961962776,
3.5071791309306));
#34345=CARTESIAN_POINT('Ctrl Pts',(-0.126473800166976,-0.012232524903913,
3.50641858178433));
#34346=CARTESIAN_POINT('Ctrl Pts',(-0.126365398388193,-0.00016976464794081,
3.50565803263806));
#34347=CARTESIAN_POINT('Ctrl Pts',(-0.126245375007135,3.12536796039931E-5,
3.51934196736194));
#34348=CARTESIAN_POINT('Ctrl Pts',(-0.12620420233203,-0.0227115638743483,
3.52076771003711));
#34349=CARTESIAN_POINT('Ctrl Pts',(-0.120346328214258,-0.0454763003201931,
3.52219345271228));
#34350=CARTESIAN_POINT('Ctrl Pts',(-0.108800985171859,-0.06484981090145,
3.52361919538745));
#34351=CARTESIAN_POINT('Ctrl Pts',(-0.0873697382082225,-0.100812232138721,
3.52626575541307));
#34352=CARTESIAN_POINT('Ctrl Pts',(-0.0463410109843132,-0.125089405892421,
3.5289123154387));
#34353=CARTESIAN_POINT('Ctrl Pts',(-0.0045038827259274,-0.126577024986295,
3.53155887546432));
#34354=CARTESIAN_POINT('Ctrl Pts',(0.0373332455324584,-0.128064644080169,
3.53420543548995));
#34355=CARTESIAN_POINT('Ctrl Pts',(0.0799787748253208,-0.106762708514216,
3.53685199551558));
#34356=CARTESIAN_POINT('Ctrl Pts',(0.103913443798274,-0.0724181339568129,
3.5394985555412));
#34357=CARTESIAN_POINT('Ctrl Pts',(0.127848112771228,-0.0380735593994097,
3.54214511556683));
#34358=CARTESIAN_POINT('Ctrl Pts',(0.133071921424273,0.00931365414944368,
3.54479167559245));
#34359=CARTESIAN_POINT('Ctrl Pts',(0.117191739814205,0.0480476856196858,
3.54743823561807));
#34360=CARTESIAN_POINT('Ctrl Pts',(0.101311558204136,0.086781717089928,
3.5500847956437));
#34361=CARTESIAN_POINT('Ctrl Pts',(0.0643273863309551,0.116862566481559,
3.55273135566933));
#34362=CARTESIAN_POINT('Ctrl Pts',(0.0231710436075753,0.124520839933968,
3.55537791569495));
#34363=CARTESIAN_POINT('Ctrl Pts',(-0.0179852991158045,0.132179113386376,
3.55802447572058));
#34364=CARTESIAN_POINT('Ctrl Pts',(-0.0633138126893829,0.117414810899563,
3.5606710357462));
#34365=CARTESIAN_POINT('Ctrl Pts',(-0.0920640726196609,0.0869862082349088,
3.56331759577183));
#34366=CARTESIAN_POINT('Ctrl Pts',(-0.113878836874053,0.0638979719779231,
3.5653257196352));
#34367=CARTESIAN_POINT('Ctrl Pts',(-0.126149033113671,0.0317913564834069,
3.56733384349857));
#34368=CARTESIAN_POINT('Ctrl Pts',(-0.126440375727766,-0.00011573372396179,
3.56934196736194));
#34369=CARTESIAN_POINT('Origin',(0.,0.,3.7));
#34370=CARTESIAN_POINT('',(-0.126640903602401,4.27927297787234E-5,3.61934196736194));
#34371=CARTESIAN_POINT('',(-0.126360536148104,0.000106176725758032,3.60565803263806));
#34372=CARTESIAN_POINT('',(-0.12645,1.54856587752183E-17,3.7));
#34373=CARTESIAN_POINT('Ctrl Pts',(-0.126360536148104,0.000106176725758032,
3.60565803263806));
#34374=CARTESIAN_POINT('Ctrl Pts',(-0.126463554653562,0.0130615819764901,
3.6048439687585));
#34375=CARTESIAN_POINT('Ctrl Pts',(-0.124630630169346,0.0259885352839278,
3.60402990487894));
#34376=CARTESIAN_POINT('Ctrl Pts',(-0.120740583509641,0.0382635675762761,
3.60321584099939));
#34377=CARTESIAN_POINT('Ctrl Pts',(-0.108093858546251,0.0781702758752103,
3.60056928097376));
#34378=CARTESIAN_POINT('Ctrl Pts',(-0.0737047770896513,0.111186630609157,
3.59792272094814));
#34379=CARTESIAN_POINT('Ctrl Pts',(-0.0333162689132352,0.122198227017938,
3.59527616092251));
#34380=CARTESIAN_POINT('Ctrl Pts',(0.00707223926318085,0.133209823426719,
3.59262960089688));
#34381=CARTESIAN_POINT('Ctrl Pts',(0.0534601741594139,0.122216661510335,
3.58998304087126));
#34382=CARTESIAN_POINT('Ctrl Pts',(0.0846116648984234,0.0942510766887394,
3.58733648084563));
#34383=CARTESIAN_POINT('Ctrl Pts',(0.115763155637433,0.0662854918671437,
3.58468992082001));
#34384=CARTESIAN_POINT('Ctrl Pts',(0.131678202219219,0.0213474841403372,
3.58204336079438));
#34385=CARTESIAN_POINT('Ctrl Pts',(0.125071080316048,-0.0199904290876357,
3.57939680076876));
#34386=CARTESIAN_POINT('Ctrl Pts',(0.118463958412876,-0.0613283423156084,
3.57675024074313));
#34387=CARTESIAN_POINT('Ctrl Pts',(0.0893346680247476,-0.0990661610447472,
3.57410368071751));
#34388=CARTESIAN_POINT('Ctrl Pts',(0.0510182611448099,-0.115928737877881,
3.57145712069188));
#34389=CARTESIAN_POINT('Ctrl Pts',(0.0127018542648722,-0.132791314711016,
3.56881056066626));
#34390=CARTESIAN_POINT('Ctrl Pts',(-0.0348016691068745,-0.128778649648146,
3.56616400064063));
#34391=CARTESIAN_POINT('Ctrl Pts',(-0.069745724184294,-0.105726139172113,
3.56351744061501));
#34392=CARTESIAN_POINT('Ctrl Pts',(-0.104336486351438,-0.0829066951932904,
3.56089763795602));
#34393=CARTESIAN_POINT('Ctrl Pts',(-0.126620455001409,-0.0414304545565597,
3.55827783529704));
#34394=CARTESIAN_POINT('Ctrl Pts',(-0.126657922659285,8.80032312977707E-6,
3.55565803263806));
#34395=CARTESIAN_POINT('Ctrl Pts',(-0.126440375727766,-0.00011573372396179,
3.56934196736194));
#34396=CARTESIAN_POINT('Ctrl Pts',(-0.126533001319164,-0.0102598491305144,
3.5699804035242));
#34397=CARTESIAN_POINT('Ctrl Pts',(-0.125414835808849,-0.020383797044434,
3.57061883968645));
#34398=CARTESIAN_POINT('Ctrl Pts',(-0.123007652953296,-0.0301913583035261,
3.5712572758487));
#34399=CARTESIAN_POINT('Ctrl Pts',(-0.113028967069674,-0.0708474193348126,
3.57390383587433));
#34400=CARTESIAN_POINT('Ctrl Pts',(-0.0808995890154535,-0.10606663855489,
3.57655039589995));
#34401=CARTESIAN_POINT('Ctrl Pts',(-0.0413281018804841,-0.119726229337694,
3.57919695592558));
#34402=CARTESIAN_POINT('Ctrl Pts',(-0.00175661474551533,-0.133385820120498,
3.5818435159512));
#34403=CARTESIAN_POINT('Ctrl Pts',(0.0452569814702019,-0.125485782466029,
3.58449007597683));
#34404=CARTESIAN_POINT('Ctrl Pts',(0.0781904578005954,-0.0996425759257176,
3.58713663600245));
#34405=CARTESIAN_POINT('Ctrl Pts',(0.111123934130988,-0.0737993693854069,
3.58978319602808));
#34406=CARTESIAN_POINT('Ctrl Pts',(0.129977290576058,-0.0300129939592548,
3.5924297560537));
#34407=CARTESIAN_POINT('Ctrl Pts',(0.126119643637387,0.0116716003968688,
3.59507631607933));
#34408=CARTESIAN_POINT('Ctrl Pts',(0.122261996698715,0.0533561947529935,
3.59772287610496));
#34409=CARTESIAN_POINT('Ctrl Pts',(0.0956933463762995,0.0929390080390894,
3.60036943613058));
#34410=CARTESIAN_POINT('Ctrl Pts',(0.0585765347711879,0.112299501333378,
3.60301599615621));
#34411=CARTESIAN_POINT('Ctrl Pts',(0.0214597231660768,0.131659994627667,
3.60566255618183));
#34412=CARTESIAN_POINT('Ctrl Pts',(-0.0262052497217305,0.130798167930148,
3.60830911620746));
#34413=CARTESIAN_POINT('Ctrl Pts',(-0.0625979093128853,0.11010854389779,
3.61095567623308));
#34414=CARTESIAN_POINT('Ctrl Pts',(-0.0989905689040401,0.089418919865431,
3.61360223625871));
#34415=CARTESIAN_POINT('Ctrl Pts',(-0.124110915198542,0.048901498498232,
3.61624879628433));
#34416=CARTESIAN_POINT('Ctrl Pts',(-0.12645913501461,0.00710470077718534,
3.61889535630996));
#34417=CARTESIAN_POINT('Ctrl Pts',(-0.126591223576389,0.00475360959731907,
3.61904422666062));
#34418=CARTESIAN_POINT('Ctrl Pts',(-0.126651258400685,0.00239847031733228,
3.61919309701128));
#34419=CARTESIAN_POINT('Ctrl Pts',(-0.126640903602401,4.27927297787234E-5,
3.61934196736194));
#34420=CARTESIAN_POINT('Origin',(0.,0.,3.7));
#34421=CARTESIAN_POINT('',(-0.126313625852874,8.92012377725487E-5,3.66934196736194));
#34422=CARTESIAN_POINT('',(-0.126280524269743,-6.82698929511343E-5,3.65565803263806));
#34423=CARTESIAN_POINT('',(-0.12645,1.54856587752183E-17,3.7));
#34424=CARTESIAN_POINT('Ctrl Pts',(-0.126280524269743,-6.82698929511343E-5,
3.65565803263806));
#34425=CARTESIAN_POINT('Ctrl Pts',(-0.126155459137289,0.0254573418705088,
3.65405666224558));
#34426=CARTESIAN_POINT('Ctrl Pts',(-0.1186500792639,0.0510505822956786,
3.65245529185311));
#34427=CARTESIAN_POINT('Ctrl Pts',(-0.104270310346229,0.0719033403784211,
3.65085392146064));
#34428=CARTESIAN_POINT('Ctrl Pts',(-0.0805050891493468,0.106366370433962,
3.64820736143502));
#34429=CARTESIAN_POINT('Ctrl Pts',(-0.0379633950684185,0.127881407935326,
3.64556080140939));
#34430=CARTESIAN_POINT('Ctrl Pts',(0.00387966794034225,0.126599115215449,
3.64291424138376));
#34431=CARTESIAN_POINT('Ctrl Pts',(0.0457227309491033,0.125316822495572,
3.64026768135814));
#34432=CARTESIAN_POINT('Ctrl Pts',(0.0868671628856968,0.101237199554454,
3.63762112133251));
#34433=CARTESIAN_POINT('Ctrl Pts',(0.108477510477425,0.0653836202783246,
3.63497456130689));
#34434=CARTESIAN_POINT('Ctrl Pts',(0.130087858069152,0.0295300410021955,
3.63232800128126));
#34435=CARTESIAN_POINT('Ctrl Pts',(0.132164121316015,-0.018097494608945,
3.62968144125564));
#34436=CARTESIAN_POINT('Ctrl Pts',(0.113755810560665,-0.0556956347668708,
3.62703488123001));
#34437=CARTESIAN_POINT('Ctrl Pts',(0.0953474998053144,-0.0932937749247968,
3.62438832120439));
#34438=CARTESIAN_POINT('Ctrl Pts',(0.0564546150477511,-0.120862519629508,
3.62174176117876));
#34439=CARTESIAN_POINT('Ctrl Pts',(0.0148818767183724,-0.125781225334577,
3.61909520115314));
#34440=CARTESIAN_POINT('Ctrl Pts',(-0.0266908616110063,-0.130699931039647,
3.61644864112751));
#34441=CARTESIAN_POINT('Ctrl Pts',(-0.0709434535122003,-0.112968597745074,
3.61380208110189));
#34442=CARTESIAN_POINT('Ctrl Pts',(-0.0976175652277067,-0.0807044001658271,
3.61115552107626));
#34443=CARTESIAN_POINT('Ctrl Pts',(-0.116086901439685,-0.0583644505151555,
3.60932302493019));
#34444=CARTESIAN_POINT('Ctrl Pts',(-0.126128636638782,-0.0290570508647223,
3.60749052878412));
#34445=CARTESIAN_POINT('Ctrl Pts',(-0.126360536148104,0.000106176725758032,
3.60565803263806));
#34446=CARTESIAN_POINT('Ctrl Pts',(-0.126640903602401,4.27927297787234E-5,
3.61934196736194));
#34447=CARTESIAN_POINT('Ctrl Pts',(-0.126467174766239,-0.0394798628014113,
3.62183965703691));
#34448=CARTESIAN_POINT('Ctrl Pts',(-0.106479582237496,-0.0791540456794125,
3.62433734671187));
#34449=CARTESIAN_POINT('Ctrl Pts',(-0.0745372494842149,-0.102404041708738,
3.62683503638683));
#34450=CARTESIAN_POINT('Ctrl Pts',(-0.0406910508001211,-0.12703981239872,
3.62948159641246));
#34451=CARTESIAN_POINT('Ctrl Pts',(0.00657743990569856,-0.133235179703789,
3.63212815643808));
#34452=CARTESIAN_POINT('Ctrl Pts',(0.0456292459986054,-0.118153973308938,
3.63477471646371));
#34453=CARTESIAN_POINT('Ctrl Pts',(0.0846810520915122,-0.103072766914087,
3.63742127648934));
#34454=CARTESIAN_POINT('Ctrl Pts',(0.115516173571506,-0.0667149868193161,
3.64006783651496));
#34455=CARTESIAN_POINT('Ctrl Pts',(0.124018641769873,-0.0257248122789798,
3.64271439654059));
#34456=CARTESIAN_POINT('Ctrl Pts',(0.132521109968241,0.0152653622613568,
3.64536095656621));
#34457=CARTESIAN_POINT('Ctrl Pts',(0.11869092488498,0.0608879312472584,
3.64800751659183));
#34458=CARTESIAN_POINT('Ctrl Pts',(0.0888593883296617,0.0902574016134864,
3.65065407661746));
#34459=CARTESIAN_POINT('Ctrl Pts',(0.0590278517743432,0.119626871979714,
3.65330063664309));
#34460=CARTESIAN_POINT('Ctrl Pts',(0.0131949637469664,0.132743243726269,
3.65594719666871));
#34461=CARTESIAN_POINT('Ctrl Pts',(-0.027657500752443,0.123601990750641,
3.65859375669434));
#34462=CARTESIAN_POINT('Ctrl Pts',(-0.0685099652518527,0.114460737775013,
3.66124031671997));
#34463=CARTESIAN_POINT('Ctrl Pts',(-0.104382006223295,0.0830618600772021,
3.66388687674559));
#34464=CARTESIAN_POINT('Ctrl Pts',(-0.118851810998494,0.043779407059542,
3.66653343677121));
#34465=CARTESIAN_POINT('Ctrl Pts',(-0.123970265263591,0.0298838886116103,
3.66746961363479));
#34466=CARTESIAN_POINT('Ctrl Pts',(-0.126410714036168,0.0150019191305398,
3.66840579049837));
#34467=CARTESIAN_POINT('Ctrl Pts',(-0.126313625852874,8.92012377725487E-5,
3.66934196736194));
#34468=CARTESIAN_POINT('Origin',(0.,0.,3.7));
#34469=CARTESIAN_POINT('',(-0.126318202311182,-9.13759226411071E-5,3.71934196736194));
#34470=CARTESIAN_POINT('',(-0.126609590382811,-7.02044759900073E-5,3.70565803263806));
#34471=CARTESIAN_POINT('',(-0.12645,1.54856587752183E-17,3.7));
#34472=CARTESIAN_POINT('Ctrl Pts',(-0.126609590382811,-7.02044759900073E-5,
3.70565803263806));
#34473=CARTESIAN_POINT('Ctrl Pts',(-0.126357411318116,0.0377522139233435,
3.70326935573267));
#34474=CARTESIAN_POINT('Ctrl Pts',(-0.108290467899376,0.0757836426892297,
3.70088067882728));
#34475=CARTESIAN_POINT('Ctrl Pts',(-0.0786816086433086,0.099255188273642,
3.6984920019219));
#34476=CARTESIAN_POINT('Ctrl Pts',(-0.0458761575859702,0.125260737263231,
3.69584544189627));
#34477=CARTESIAN_POINT('Ctrl Pts',(0.00109788169852634,0.133392911300054,
3.69319888187064));
#34478=CARTESIAN_POINT('Ctrl Pts',(0.0407363279886946,0.119928893584969,
3.69055232184502));
#34479=CARTESIAN_POINT('Ctrl Pts',(0.0803747742788628,0.106464875869883,
3.68790576181939));
#34480=CARTESIAN_POINT('Ctrl Pts',(0.112677627574703,0.071404666402888,
3.68525920179377));
#34481=CARTESIAN_POINT('Ctrl Pts',(0.122857008829439,0.0307984304737455,
3.68261264176814));
#34482=CARTESIAN_POINT('Ctrl Pts',(0.133036390084175,-0.00980780545539708,
3.67996608174252));
#34483=CARTESIAN_POINT('Ctrl Pts',(0.121092299297808,-0.0559600678466875,
3.67731952171689));
#34484=CARTESIAN_POINT('Ctrl Pts',(0.0924926054626293,-0.08653037546552,
3.67467296169127));
#34485=CARTESIAN_POINT('Ctrl Pts',(0.0638929116274508,-0.117100683084353,
3.67202640166564));
#34486=CARTESIAN_POINT('Ctrl Pts',(0.0186376147434612,-0.132089035930727,
3.66937984164002));
#34487=CARTESIAN_POINT('Ctrl Pts',(-0.0225559247032424,-0.124633936707157,
3.66673328161439));
#34488=CARTESIAN_POINT('Ctrl Pts',(-0.063749464149946,-0.117178837483586,
3.66408672158877));
#34489=CARTESIAN_POINT('Ctrl Pts',(-0.100881246159364,-0.0872802861900701,
3.66144016156314));
#34490=CARTESIAN_POINT('Ctrl Pts',(-0.116952763007655,-0.0486254992384533,
3.65879360153752));
#34491=CARTESIAN_POINT('Ctrl Pts',(-0.123299788065177,-0.0333598025596003,
3.65774841190436));
#34492=CARTESIAN_POINT('Ctrl Pts',(-0.126362152343126,-0.016728441031668,
3.65670322227121));
#34493=CARTESIAN_POINT('Ctrl Pts',(-0.126280524269743,-6.82698929511343E-5,
3.65565803263806));
#34494=CARTESIAN_POINT('Ctrl Pts',(-0.126313625852874,8.92012377725487E-5,
3.66934196736194));
#34495=CARTESIAN_POINT('Ctrl Pts',(-0.126136246983132,-0.027156143714207,
3.67105235052399));
#34496=CARTESIAN_POINT('Ctrl Pts',(-0.117488868450918,-0.0545041232450019,
3.67276273368604));
#34497=CARTESIAN_POINT('Ctrl Pts',(-0.101228105076468,-0.0761266063810683,
3.67447311684809));
#34498=CARTESIAN_POINT('Ctrl Pts',(-0.0760670258002872,-0.10958413846651,
3.67711967687372));
#34499=CARTESIAN_POINT('Ctrl Pts',(-0.0326772986689716,-0.129333174299883,
3.67976623689934));
#34500=CARTESIAN_POINT('Ctrl Pts',(0.00907775247578101,-0.126332829739009,
3.68241279692497));
#34501=CARTESIAN_POINT('Ctrl Pts',(0.050832803620533,-0.123332485178135,
3.68505935695059));
#34502=CARTESIAN_POINT('Ctrl Pts',(0.0909531787787221,-0.0975827602230137,
3.68770591697622));
#34503=CARTESIAN_POINT('Ctrl Pts',(0.11107222624856,-0.0608715862708329,
3.69035247700184));
#34504=CARTESIAN_POINT('Ctrl Pts',(0.131191273718398,-0.0241604123186516,
3.69299903702747));
#34505=CARTESIAN_POINT('Ctrl Pts',(0.131308993499885,0.0235122106305895,
3.69564559705309));
#34506=CARTESIAN_POINT('Ctrl Pts',(0.111371494820412,0.0603222977018694,
3.69829215707872));
#34507=CARTESIAN_POINT('Ctrl Pts',(0.0914339961409399,0.097132384773149,
3.70093871710434));
#34508=CARTESIAN_POINT('Ctrl Pts',(0.0514412790005074,0.123079935966467,
3.70358527712997));
#34509=CARTESIAN_POINT('Ctrl Pts',(0.00970155469863815,0.126286457292336,
3.70623183715559));
#34510=CARTESIAN_POINT('Ctrl Pts',(-0.0320381696032317,0.129492978618205,
3.70887839718122));
#34511=CARTESIAN_POINT('Ctrl Pts',(-0.0755249010665388,0.109958470076624,
3.71152495720684));
#34512=CARTESIAN_POINT('Ctrl Pts',(-0.100850908347825,0.0766256076274997,
3.71417151723247));
#34513=CARTESIAN_POINT('Ctrl Pts',(-0.117343620441844,0.0549186998809637,
3.71589500060896));
#34514=CARTESIAN_POINT('Ctrl Pts',(-0.126134681028771,0.0273601470071565,
3.71761848398545));
#34515=CARTESIAN_POINT('Ctrl Pts',(-0.126318202311182,-9.13759226411071E-5,
3.71934196736194));
#34516=CARTESIAN_POINT('Origin',(0.,0.,3.7));
#34517=CARTESIAN_POINT('',(-0.126643738265873,-3.92119282522094E-5,3.76934196736194));
#34518=CARTESIAN_POINT('',(-0.126492921331233,0.000111898061355794,3.75565803263806));
#34519=CARTESIAN_POINT('',(-0.12645,1.54856587752183E-17,3.7));
#34520=CARTESIAN_POINT('Ctrl Pts',(-0.126492921331233,0.000111898061355794,
3.75565803263806));
#34521=CARTESIAN_POINT('Ctrl Pts',(-0.12657025228906,0.00851493641555574,
3.75512860924538));
#34522=CARTESIAN_POINT('Ctrl Pts',(-0.125804504023154,0.0169039539351017,
3.7545991858527));
#34523=CARTESIAN_POINT('Ctrl Pts',(-0.12414416907011,0.0251120135156184,
3.75406976246003));
#34524=CARTESIAN_POINT('Ctrl Pts',(-0.115844240928182,0.06614367678216,
3.7514232024344));
#34525=CARTESIAN_POINT('Ctrl Pts',(-0.0851890554053168,0.102653294996741,
3.74877664240878));
#34526=CARTESIAN_POINT('Ctrl Pts',(-0.0462122079706087,0.117927179951992,
3.74613008238315));
#34527=CARTESIAN_POINT('Ctrl Pts',(-0.00723536053590029,0.133201064907244,
3.74348352235752));
#34528=CARTESIAN_POINT('Ctrl Pts',(0.0400631488106516,0.127239216603166,
3.7408369623319));
#34529=CARTESIAN_POINT('Ctrl Pts',(0.0740306001411793,0.102770901424588,
3.73819040230627));
#34530=CARTESIAN_POINT('Ctrl Pts',(0.107998051471707,0.0783025862460102,
3.73554384228065));
#34531=CARTESIAN_POINT('Ctrl Pts',(0.12863444478621,0.0353278041929325,
3.73289728225502));
#34532=CARTESIAN_POINT('Ctrl Pts',(0.126492673803057,-0.00648007801438488,
3.7302507222294));
#34533=CARTESIAN_POINT('Ctrl Pts',(0.124350902819903,-0.0482879602217022,
3.72760416220377));
#34534=CARTESIAN_POINT('Ctrl Pts',(0.0994309675390923,-0.0889289425832592,
3.72495760217815));
#34535=CARTESIAN_POINT('Ctrl Pts',(0.063140931062625,-0.109798045345167,
3.72231104215252));
#34536=CARTESIAN_POINT('Ctrl Pts',(0.0268508945861577,-0.130667148107075,
3.7196644821269));
#34537=CARTESIAN_POINT('Ctrl Pts',(-0.020809243085966,-0.131764371269333,
3.71701792210127));
#34538=CARTESIAN_POINT('Ctrl Pts',(-0.0580212126891809,-0.112587418545307,
3.71437136207565));
#34539=CARTESIAN_POINT('Ctrl Pts',(-0.0952331822923957,-0.0934104658212808,
3.71172480205002));
#34540=CARTESIAN_POINT('Ctrl Pts',(-0.121996983826702,-0.0539593372109697,
3.7090782420244));
#34541=CARTESIAN_POINT('Ctrl Pts',(-0.126060453178764,-0.0122943109346363,
3.70643168199877));
#34542=CARTESIAN_POINT('Ctrl Pts',(-0.126456401181211,-0.00823443438662399,
3.70617379887853));
#34543=CARTESIAN_POINT('Ctrl Pts',(-0.126636815799491,-0.0041535374917583,
3.70591591575829));
#34544=CARTESIAN_POINT('Ctrl Pts',(-0.126609590382811,-7.02044759900073E-5,
3.70565803263806));
#34545=CARTESIAN_POINT('Ctrl Pts',(-0.126318202311182,-9.13759226411071E-5,
3.71934196736194));
#34546=CARTESIAN_POINT('Ctrl Pts',(-0.126416494068865,-0.0147940763636936,
3.72026504401107));
#34547=CARTESIAN_POINT('Ctrl Pts',(-0.12404567634908,-0.0294660748073717,
3.72118812066021));
#34548=CARTESIAN_POINT('Ctrl Pts',(-0.119066572492589,-0.0431919063448052,
3.72211119730934));
#34549=CARTESIAN_POINT('Ctrl Pts',(-0.104790946256804,-0.0825453415113195,
3.72475775733497));
#34550=CARTESIAN_POINT('Ctrl Pts',(-0.0690744106859675,-0.11412099548768,
3.7274043173606));
#34551=CARTESIAN_POINT('Ctrl Pts',(-0.0282675897675097,-0.123463892809314,
3.73005087738622));
#34552=CARTESIAN_POINT('Ctrl Pts',(0.0125392311509478,-0.132806790130948,
3.73269743741185));
#34553=CARTESIAN_POINT('Ctrl Pts',(0.0584363374170267,-0.119916930797855,
3.73534399743747));
#34554=CARTESIAN_POINT('Ctrl Pts',(0.0884125555029259,-0.0906951458916328,
3.7379905574631));
#34555=CARTESIAN_POINT('Ctrl Pts',(0.118388773588825,-0.0614733609854108,
3.74063711748872));
#34556=CARTESIAN_POINT('Ctrl Pts',(0.132444103494545,-0.0159196505060593,
3.74328367751435));
#34557=CARTESIAN_POINT('Ctrl Pts',(0.124144174958903,0.0251120147068241,
3.74593023753997));
#34558=CARTESIAN_POINT('Ctrl Pts',(0.115844246423262,0.0661436799197074,
3.7485767975656));
#34559=CARTESIAN_POINT('Ctrl Pts',(0.0851890594462595,0.102653299866123,
3.75122335759122));
#34560=CARTESIAN_POINT('Ctrl Pts',(0.0462122101626772,0.117927185545889,
3.75386991761685));
#34561=CARTESIAN_POINT('Ctrl Pts',(0.00723536087909469,0.133201071225655,
3.75651647764247));
#34562=CARTESIAN_POINT('Ctrl Pts',(-0.0400631507110678,0.127239222638772,
3.7591630376681));
#34563=CARTESIAN_POINT('Ctrl Pts',(-0.0740306036528435,0.102770906299531,
3.76180959769372));
#34564=CARTESIAN_POINT('Ctrl Pts',(-0.106255505634774,0.0795578294448588,
3.76432038758313));
#34565=CARTESIAN_POINT('Ctrl Pts',(-0.12648204772981,0.0396883664632768,
3.76683117747254));
#34566=CARTESIAN_POINT('Ctrl Pts',(-0.126643738265873,-3.92119282522094E-5,
3.76934196736194));
#34567=CARTESIAN_POINT('Origin',(0.,0.,3.7));
#34568=CARTESIAN_POINT('',(-0.12643411897368,0.000115681837355761,3.81934196736194));
#34569=CARTESIAN_POINT('',(-0.126243465328102,1.71616150689059E-6,3.80565803263806));
#34570=CARTESIAN_POINT('',(-0.12645,1.54856587752183E-17,3.7));
#34571=CARTESIAN_POINT('Ctrl Pts',(-0.126243465328102,1.71616150689059E-6,
3.80565803263806));
#34572=CARTESIAN_POINT('Ctrl Pts',(-0.126246007062352,0.0210055997219054,
3.80434130273247));
#34573=CARTESIAN_POINT('Ctrl Pts',(-0.121290894068088,0.0420083553470164,
3.80302457282688));
#34574=CARTESIAN_POINT('Ctrl Pts',(-0.111371489537494,0.0603222948404575,
3.80170784292128));
#34575=CARTESIAN_POINT('Ctrl Pts',(-0.0914339918037617,0.0971323801656441,
3.79906128289566));
#34576=CARTESIAN_POINT('Ctrl Pts',(-0.0514412765603963,0.123079930128149,
3.79641472287003));
#34577=CARTESIAN_POINT('Ctrl Pts',(-0.00970155423845781,0.126286451301922,
3.79376816284441));
#34578=CARTESIAN_POINT('Ctrl Pts',(0.0320381680834807,0.129492972475696,
3.79112160281878));
#34579=CARTESIAN_POINT('Ctrl Pts',(0.0755248974839926,0.109958464860738,
3.78847504279316));
#34580=CARTESIAN_POINT('Ctrl Pts',(0.10085090356394,0.0766256039927644,
3.78582848276753));
#34581=CARTESIAN_POINT('Ctrl Pts',(0.126176909643887,0.0432927431247909,
3.78318192274191));
#34582=CARTESIAN_POINT('Ctrl Pts',(0.13334219240327,-0.00383847099619805,
3.78053536271628));
#34583=CARTESIAN_POINT('Ctrl Pts',(0.119066566844655,-0.0431919042959778,
3.77788880269065));
#34584=CARTESIAN_POINT('Ctrl Pts',(0.10479094128604,-0.0825453375957573,
3.77524224266503));
#34585=CARTESIAN_POINT('Ctrl Pts',(0.0690744074094266,-0.114120990074327,
3.7725956826394));
#34586=CARTESIAN_POINT('Ctrl Pts',(0.0282675884266474,-0.123463886952785,
3.76994912261378));
#34587=CARTESIAN_POINT('Ctrl Pts',(-0.0125392305561318,-0.132806783831242,
3.76730256258815));
#34588=CARTESIAN_POINT('Ctrl Pts',(-0.0584363346450773,-0.119916925109586,
3.76465600256253));
#34589=CARTESIAN_POINT('Ctrl Pts',(-0.088412551309054,-0.0906951415895065,
3.7620094425369));
#34590=CARTESIAN_POINT('Ctrl Pts',(-0.112392263011044,-0.0673189446502994,
3.75989230590395));
#34591=CARTESIAN_POINT('Ctrl Pts',(-0.126183678849807,-0.0334914156074963,
3.75777516927101));
#34592=CARTESIAN_POINT('Ctrl Pts',(-0.126492921331233,0.000111898061355794,
3.75565803263806));
#34593=CARTESIAN_POINT('Ctrl Pts',(-0.126643738265873,-3.92119282522094E-5,
3.76934196736194));
#34594=CARTESIAN_POINT('Ctrl Pts',(-0.12665248162835,-0.00218746764357669,
3.76947773749816));
#34595=CARTESIAN_POINT('Ctrl Pts',(-0.126602553960315,-0.00433530847842783,
3.76961350763438));
#34596=CARTESIAN_POINT('Ctrl Pts',(-0.126492679803253,-0.0064800783217853,
3.7697492777706));
#34597=CARTESIAN_POINT('Ctrl Pts',(-0.124350908718499,-0.0482879625122638,
3.77239583779623));
#34598=CARTESIAN_POINT('Ctrl Pts',(-0.0994309722556023,-0.0889289468016232,
3.77504239782185));
#34599=CARTESIAN_POINT('Ctrl Pts',(-0.0631409340577098,-0.109798050553457,
3.77768895784748));
#34600=CARTESIAN_POINT('Ctrl Pts',(-0.0268508958598173,-0.130667154305292,
3.7803355178731));
#34601=CARTESIAN_POINT('Ctrl Pts',(0.0208092440730706,-0.131764377519601,
3.78298207789873));
#34602=CARTESIAN_POINT('Ctrl Pts',(0.0580212154414384,-0.112587423885904,
3.78562863792435));
#34603=CARTESIAN_POINT('Ctrl Pts',(0.0952331868098064,-0.0934104702522078,
3.78827519794998));
#34604=CARTESIAN_POINT('Ctrl Pts',(0.121996989613654,-0.0539593397705055,
3.7909217579756));
#34605=CARTESIAN_POINT('Ctrl Pts',(0.126060459158462,-0.0122943115177929,
3.79356831800123));
#34606=CARTESIAN_POINT('Ctrl Pts',(0.130123928703269,0.0293707167349194,
3.79621487802685));
#34607=CARTESIAN_POINT('Ctrl Pts',(0.111487064989038,0.073249642758642,
3.79886143805248));
#34608=CARTESIAN_POINT('Ctrl Pts',(0.0786816123755665,0.0992551929818185,
3.8015079980781));
#34609=CARTESIAN_POINT('Ctrl Pts',(0.0458761597620954,0.125260743204995,
3.80415455810373));
#34610=CARTESIAN_POINT('Ctrl Pts',(-0.00109788175061491,0.133392917627625,
3.80680111812935));
#34611=CARTESIAN_POINT('Ctrl Pts',(-0.0407363299210399,0.119928899273839,
3.80944767815498));
#34612=CARTESIAN_POINT('Ctrl Pts',(-0.0803747780914649,0.106464880920053,
3.81209423818061));
#34613=CARTESIAN_POINT('Ctrl Pts',(-0.112677632919605,0.071404669789851,
3.81474079820623));
#34614=CARTESIAN_POINT('Ctrl Pts',(-0.122857014657189,0.030798431934596,
3.81738735823185));
#34615=CARTESIAN_POINT('Ctrl Pts',(-0.125362998814015,0.0208018927186779,
3.81803889460855));
#34616=CARTESIAN_POINT('Ctrl Pts',(-0.126528173261855,0.0104692323861157,
3.81869043098525));
#34617=CARTESIAN_POINT('Ctrl Pts',(-0.12643411897368,0.000115681837355761,
3.81934196736194));
#34618=CARTESIAN_POINT('Origin',(0.,0.,3.7));
#34619=CARTESIAN_POINT('',(-0.126249985800877,-2.99474503126992E-5,3.86934196736194));
#34620=CARTESIAN_POINT('',(-0.126486618721746,-0.000112766438119152,3.85565803263806));
#34621=CARTESIAN_POINT('',(-0.12645,1.54856587752183E-17,3.7));
#34622=CARTESIAN_POINT('Ctrl Pts',(-0.126486618721746,-0.000112766438119152,
3.85565803263806));
#34623=CARTESIAN_POINT('Ctrl Pts',(-0.126178545401481,0.0332869000256312,
3.85355399621955));
#34624=CARTESIAN_POINT('Ctrl Pts',(-0.112575693492532,0.0669084342579941,
3.85144995980104));
#34625=CARTESIAN_POINT('Ctrl Pts',(-0.0888593841145145,0.0902573973319142,
3.84934592338254));
#34626=CARTESIAN_POINT('Ctrl Pts',(-0.0590278489741825,0.119626866304839,
3.84669936335691));
#34627=CARTESIAN_POINT('Ctrl Pts',(-0.0131949631210826,0.13274323742959,
3.84405280333129));
#34628=CARTESIAN_POINT('Ctrl Pts',(0.0276574994404428,0.123601984887668,
3.84140624330566));
#34629=CARTESIAN_POINT('Ctrl Pts',(0.0685099620019675,0.114460732345747,
3.83875968328004));
#34630=CARTESIAN_POINT('Ctrl Pts',(0.104382001271918,0.0830618561371527,
3.83611312325441));
#34631=CARTESIAN_POINT('Ctrl Pts',(0.118851805360766,0.0437794049828168,
3.83346656322878));
#34632=CARTESIAN_POINT('Ctrl Pts',(0.133321609449615,0.00449695382848087,
3.83082000320316));
#34633=CARTESIAN_POINT('Ctrl Pts',(0.126389178357361,-0.0426690722715969,
3.82817344317753));
#34634=CARTESIAN_POINT('Ctrl Pts',(0.101228100274691,-0.0761266027699533,
3.82552688315191));
#34635=CARTESIAN_POINT('Ctrl Pts',(0.0760670221920212,-0.10958413326831,
3.82288032312628));
#34636=CARTESIAN_POINT('Ctrl Pts',(0.0326772971189339,-0.129333168164945,
3.82023376310066));
#34637=CARTESIAN_POINT('Ctrl Pts',(-0.0090777520451555,-0.12633282374641,
3.81758720307503));
#34638=CARTESIAN_POINT('Ctrl Pts',(-0.0508328012092449,-0.123332479327876,
3.81494064304941));
#34639=CARTESIAN_POINT('Ctrl Pts',(-0.0909531744643365,-0.097582755594171,
3.81229408302378));
#34640=CARTESIAN_POINT('Ctrl Pts',(-0.111072220979832,-0.0608715833833843,
3.80964752299816));
#34641=CARTESIAN_POINT('Ctrl Pts',(-0.121181537898249,-0.0424251389139816,
3.80831769287812));
#34642=CARTESIAN_POINT('Ctrl Pts',(-0.126240898306005,-0.021211136130883,
3.80698786275809));
#34643=CARTESIAN_POINT('Ctrl Pts',(-0.126243465328102,1.71616150689059E-6,
3.80565803263806));
#34644=CARTESIAN_POINT('Ctrl Pts',(-0.12643411897368,0.000115681837355761,
3.81934196736194));
#34645=CARTESIAN_POINT('Ctrl Pts',(-0.126146121962456,-0.0315871960586303,
3.82133699101087));
#34646=CARTESIAN_POINT('Ctrl Pts',(-0.114051564760291,-0.0634859411452914,
3.8233320146598));
#34647=CARTESIAN_POINT('Ctrl Pts',(-0.0924926098500027,-0.0865303795699984,
3.82532703830873));
#34648=CARTESIAN_POINT('Ctrl Pts',(-0.0638929146582029,-0.117100688639029,
3.82797359833436));
#34649=CARTESIAN_POINT('Ctrl Pts',(-0.018637615627574,-0.132089042196783,
3.83062015835998));
#34650=CARTESIAN_POINT('Ctrl Pts',(0.0225559257731756,-0.124633942619396,
3.83326671838561));
#34651=CARTESIAN_POINT('Ctrl Pts',(0.0637494671739252,-0.117178843042008,
3.83591327841123));
#34652=CARTESIAN_POINT('Ctrl Pts',(0.100881250944795,-0.0872802903294789,
3.83855983843686));
#34653=CARTESIAN_POINT('Ctrl Pts',(0.116952768555385,-0.048625501544595,
3.84120639846248));
#34654=CARTESIAN_POINT('Ctrl Pts',(0.133024286165975,-0.00997071275971127,
3.84385295848811));
#34655=CARTESIAN_POINT('Ctrl Pts',(0.128035537616284,0.0374403120975275,
3.84649951851373));
#34656=CARTESIAN_POINT('Ctrl Pts',(0.10427031529219,0.0719033437884345,
3.84914607853936));
#34657=CARTESIAN_POINT('Ctrl Pts',(0.080505092968096,0.106366375479342,
3.85179263856498));
#34658=CARTESIAN_POINT('Ctrl Pts',(0.037963396869598,0.127881414003918,
3.85443919859061));
#34659=CARTESIAN_POINT('Ctrl Pts',(-0.003879668124188,0.126599121222081,
3.85708575861623));
#34660=CARTESIAN_POINT('Ctrl Pts',(-0.0457227331179738,0.125316828440245,
3.85973231864186));
#34661=CARTESIAN_POINT('Ctrl Pts',(-0.0868671670070475,0.101237204351996,
3.86237887866749));
#34662=CARTESIAN_POINT('Ctrl Pts',(-0.108477515623481,0.0653836233772192,
3.86502543869311));
#34663=CARTESIAN_POINT('Ctrl Pts',(-0.120226312608128,0.0458912749879413,
3.86646428158272));
#34664=CARTESIAN_POINT('Ctrl Pts',(-0.126201381437229,0.0229188749131541,
3.86790312447233));
#34665=CARTESIAN_POINT('Ctrl Pts',(-0.126249985800877,-2.99474503126992E-5,
3.86934196736194));
#34666=CARTESIAN_POINT('Origin',(0.,0.,3.7));
#34667=CARTESIAN_POINT('',(-0.126543984365092,-0.000100563349596846,3.91934196736194));
#34668=CARTESIAN_POINT('',(-0.126614009842867,6.71750503076223E-5,3.90565803263806));
#34669=CARTESIAN_POINT('',(-0.12645,1.54856587752183E-17,3.7));
#34670=CARTESIAN_POINT('Ctrl Pts',(-0.126614009842867,6.71750503076223E-5,
3.90565803263806));
#34671=CARTESIAN_POINT('Ctrl Pts',(-0.126638949568151,0.00394272317787337,
3.90541324973226));
#34672=CARTESIAN_POINT('Ctrl Pts',(-0.126476435154099,0.00781615144459198,
3.90516846682647));
#34673=CARTESIAN_POINT('Ctrl Pts',(-0.126119637661472,0.0116715998582211,
3.90492368392067));
#34674=CARTESIAN_POINT('Ctrl Pts',(-0.122261990910541,0.0533561922490439,
3.90227712389504));
#34675=CARTESIAN_POINT('Ctrl Pts',(-0.0956933418361204,0.0929390036289487,
3.89963056386942));
#34676=CARTESIAN_POINT('Ctrl Pts',(-0.0585765319889427,0.112299495998321,
3.89698400384379));
#34677=CARTESIAN_POINT('Ctrl Pts',(-0.0214597221417651,0.131659988367694,
3.89433744381817));
#34678=CARTESIAN_POINT('Ctrl Pts',(0.0262052484781696,0.130798161726534,
3.89169088379254));
#34679=CARTESIAN_POINT('Ctrl Pts',(0.0625979063415064,0.110108538679153,
3.88904432376692));
#34680=CARTESIAN_POINT('Ctrl Pts',(0.0989905642048431,0.089418915631772,
3.88639776374129));
#34681=CARTESIAN_POINT('Ctrl Pts',(0.124110909311582,0.04890149617817,3.88375120371567));
#34682=CARTESIAN_POINT('Ctrl Pts',(0.12645912901712,0.0071047004378325,
3.88110464369004));
#34683=CARTESIAN_POINT('Ctrl Pts',(0.128807348722658,-0.0346920953025048,
3.87845808366442));
#34684=CARTESIAN_POINT('Ctrl Pts',(0.108383443026996,-0.0777682673295779,
3.87581152363879));
#34685=CARTESIAN_POINT('Ctrl Pts',(0.0745372459479278,-0.102404036849921,
3.87316496361316));
#34686=CARTESIAN_POINT('Ctrl Pts',(0.0406910488688595,-0.127039806370264,
3.87051840358754));
#34687=CARTESIAN_POINT('Ctrl Pts',(-0.00657743959361464,-0.133235173383876,
3.86787184356191));
#34688=CARTESIAN_POINT('Ctrl Pts',(-0.0456292438338329,-0.118153967704968,
3.86522528353629));
#34689=CARTESIAN_POINT('Ctrl Pts',(-0.0846810480740508,-0.10307276202606,
3.86257872351066));
#34690=CARTESIAN_POINT('Ctrl Pts',(-0.115516168092013,-0.0667149836546316,
3.85993216348504));
#34691=CARTESIAN_POINT('Ctrl Pts',(-0.124018635887212,-0.0257248110583692,
3.85728560345941));
#34692=CARTESIAN_POINT('Ctrl Pts',(-0.125761573683066,-0.0173221539948553,
3.85674307985229));
#34693=CARTESIAN_POINT('Ctrl Pts',(-0.126566055107683,-0.00872483577640936,
3.85620055624518));
#34694=CARTESIAN_POINT('Ctrl Pts',(-0.126486618721746,-0.000112766438119152,
3.85565803263806));
#34695=CARTESIAN_POINT('Ctrl Pts',(-0.126249985800877,-2.99474503126992E-5,
3.86934196736194));
#34696=CARTESIAN_POINT('Ctrl Pts',(-0.126290782696275,-0.01929242997697,
3.87054968449796));
#34697=CARTESIAN_POINT('Ctrl Pts',(-0.12215616704665,-0.0385383011374065,
3.87175740163397));
#34698=CARTESIAN_POINT('Ctrl Pts',(-0.113755815955893,-0.0556956374040618,
3.87296511876998));
#34699=CARTESIAN_POINT('Ctrl Pts',(-0.0953475043280787,-0.0932937793492606,
3.87561167879561));
#34700=CARTESIAN_POINT('Ctrl Pts',(-0.0564546177286578,-0.120862525378353,
3.87825823882124));
#34701=CARTESIAN_POINT('Ctrl Pts',(-0.0148818774258165,-0.125781231309797,
3.88090479884686));
#34702=CARTESIAN_POINT('Ctrl Pts',(0.0266908628770249,-0.13069993724124,
3.88355135887249));
#34703=CARTESIAN_POINT('Ctrl Pts',(0.0709434568832867,-0.112968603075036,
3.88619791889811));
#34704=CARTESIAN_POINT('Ctrl Pts',(0.0976175698612337,-0.0807044039779288,
3.88884447892374));
#34705=CARTESIAN_POINT('Ctrl Pts',(0.124291682839181,-0.0484402048808214,
3.89149103894936));
#34706=CARTESIAN_POINT('Ctrl Pts',(0.133387314788813,-0.00164314085281106,
3.89413759897499));
#34707=CARTESIAN_POINT('Ctrl Pts',(0.120740589231085,0.0382635693618544,
3.89678415900061));
#34708=CARTESIAN_POINT('Ctrl Pts',(0.108093863673357,0.0781702795765198,
3.89943071902624));
#34709=CARTESIAN_POINT('Ctrl Pts',(0.0737047806082696,0.11118663597784,
3.90207727905187));
#34710=CARTESIAN_POINT('Ctrl Pts',(0.0333162705051194,0.122198232868137,
3.90472383907749));
#34711=CARTESIAN_POINT('Ctrl Pts',(-0.00707223959803082,0.133209829758434,
3.90737039910312));
#34712=CARTESIAN_POINT('Ctrl Pts',(-0.0534601767392434,0.122216667137707,
3.91001695912874));
#34713=CARTESIAN_POINT('Ctrl Pts',(-0.0846116689345932,0.0942510810621984,
3.91266351915437));
#34714=CARTESIAN_POINT('Ctrl Pts',(-0.110814692885301,0.0707278765512593,
3.91488966855689));
#34715=CARTESIAN_POINT('Ctrl Pts',(-0.126237468513852,0.0351961661111841,
3.91711581795942));
#34716=CARTESIAN_POINT('Ctrl Pts',(-0.126543984365092,-0.000100563349596846,
3.91934196736194));
#34717=CARTESIAN_POINT('Origin',(0.,0.,3.7));
#34718=CARTESIAN_POINT('',(-0.126567406925801,8.9117089303592E-5,3.96934196736194));
#34719=CARTESIAN_POINT('',(-0.126283770505697,7.06948412972308E-5,3.95565803263806));
#34720=CARTESIAN_POINT('',(-0.12645,1.54856587752183E-17,3.7));
#34721=CARTESIAN_POINT('',(0.0958116152722338,0.0825211298936549,4.));
#34722=CARTESIAN_POINT('Ctrl Pts',(-0.126567406925801,8.9117089303592E-5,
3.96934196736194));
#34723=CARTESIAN_POINT('Ctrl Pts',(-0.126271512495954,-0.03602989561222,
3.97162163149775));
#34724=CARTESIAN_POINT('Ctrl Pts',(-0.11000667585855,-0.0723734458913716,
3.97390129563356));
#34725=CARTESIAN_POINT('Ctrl Pts',(-0.0826932529987204,-0.0959262598695684,
3.97618095976937));
#34726=CARTESIAN_POINT('Ctrl Pts',(-0.0509839270641226,-0.123269733404333,
3.978827519795));
#34727=CARTESIAN_POINT('Ctrl Pts',(-0.0043834430999392,-0.133373998977298,
3.98147407982063));
#34728=CARTESIAN_POINT('Ctrl Pts',(0.0357753280219188,-0.121524403040669,
3.98412063984625));
#34729=CARTESIAN_POINT('Ctrl Pts',(0.0759340991437768,-0.109674807104039,
3.98676719987188));
#34730=CARTESIAN_POINT('Ctrl Pts',(0.109651157423309,-0.0758713496578151,
3.9894137598975));
#34731=CARTESIAN_POINT('Ctrl Pts',(0.121481684447537,-0.0357885393155276,
3.99206031992312));
#34732=CARTESIAN_POINT('Ctrl Pts',(0.133312211471764,0.00429427102675994,
3.99470687994875));
#34733=CARTESIAN_POINT('Ctrl Pts',(0.123256207240687,0.0506564342651108,
3.99735343997437));
#34734=CARTESIAN_POINT('Ctrl Pts',(0.095811615272233,0.0825211298936557,
4.));
#34735=CARTESIAN_POINT('',(-0.0959939867336434,0.082660026050108,4.));
#34736=CARTESIAN_POINT('Origin',(0.,0.,4.));
#34737=CARTESIAN_POINT('Ctrl Pts',(-0.095994151316856,0.0826601513985344,
4.));
#34738=CARTESIAN_POINT('Ctrl Pts',(-0.0693049200029063,0.113544200686508,
3.9974200549221));
#34739=CARTESIAN_POINT('Ctrl Pts',(-0.0262885035315151,0.130447365396717,
3.9948401098442));
#34740=CARTESIAN_POINT('Ctrl Pts',(0.0142676559974625,0.125842964228272,
3.9922601647663));
#34741=CARTESIAN_POINT('Ctrl Pts',(0.0558709876039151,0.121119676054917,
3.98961360474068));
#34742=CARTESIAN_POINT('Ctrl Pts',(0.0948853729157606,0.0937638197023474,
3.98696704471505));
#34743=CARTESIAN_POINT('Ctrl Pts',(0.113475682659087,0.0562620533584955,
3.98432048468943));
#34744=CARTESIAN_POINT('Ctrl Pts',(0.132065992402412,0.0187602870146438,
3.9816739246638));
#34745=CARTESIAN_POINT('Ctrl Pts',(0.130232226577219,-0.0288873893204904,
3.97902736463818));
#34746=CARTESIAN_POINT('Ctrl Pts',(0.108800980591427,-0.0648498109281795,
3.97638080461255));
#34747=CARTESIAN_POINT('Ctrl Pts',(0.0873697346056348,-0.100812232535869,
3.97373424458693));
#34748=CARTESIAN_POINT('Ctrl Pts',(0.046341008459244,-0.125089399416112,
3.9710876845613));
#34749=CARTESIAN_POINT('Ctrl Pts',(0.00450388209284308,-0.126577017215687,
3.96844112453568));
#34750=CARTESIAN_POINT('Ctrl Pts',(-0.0373332442735578,-0.128064635015261,
3.96579456451005));
#34751=CARTESIAN_POINT('Ctrl Pts',(-0.0799787708599689,-0.106762703734165,
3.96314800448442));
#34752=CARTESIAN_POINT('Ctrl Pts',(-0.103913438592044,-0.0724181315163075,
3.9605014444588));
#34753=CARTESIAN_POINT('Ctrl Pts',(-0.118514209844363,-0.0514670471592998,
3.95888697385188));
#34754=CARTESIAN_POINT('Ctrl Pts',(-0.126152075437054,-0.0256623813017284,
3.95727250324497));
#34755=CARTESIAN_POINT('Ctrl Pts',(-0.126283770505697,7.06948412972308E-5,
3.95565803263806));
#34756=CARTESIAN_POINT('Origin',(0.,0.,4.11042117235887));
#34757=CARTESIAN_POINT('',(-0.154553716617854,1.07385516829317E-5,3.53957882764113));
#34758=CARTESIAN_POINT('',(-0.154050307343621,3.81371511608408E-5,3.53542117235887));
#34759=CARTESIAN_POINT('',(-0.1543,7.47606542906876E-15,4.11042117235887));
#34760=CARTESIAN_POINT('',(0.0398513841857357,-0.149064942821848,3.5));
#34761=CARTESIAN_POINT('Ctrl Pts',(-0.154050307343621,3.81371511608431E-5,
3.53542117235887));
#34762=CARTESIAN_POINT('Ctrl Pts',(-0.154093326879583,0.0238011172149125,
3.53420035500841));
#34763=CARTESIAN_POINT('Ctrl Pts',(-0.137743852801688,0.0990167675561842,
3.53033297763233));
#34764=CARTESIAN_POINT('Ctrl Pts',(-0.0205691901156568,0.181176596665036,
3.52381904023063));
#34765=CARTESIAN_POINT('Ctrl Pts',(0.141207069227503,0.115615351338242,
3.51587936015375));
#34766=CARTESIAN_POINT('Ctrl Pts',(0.173454096992073,-0.0561631599472297,
3.50793968007688));
#34767=CARTESIAN_POINT('Ctrl Pts',(0.089426887306191,-0.135811307301286,
3.50264656002563));
#34768=CARTESIAN_POINT('Ctrl Pts',(0.0398513841857336,-0.149064942821849,
3.5));
#34769=CARTESIAN_POINT('',(-0.0398513841857265,-0.149064942821851,3.5));
#34770=CARTESIAN_POINT('Origin',(0.,0.,3.5));
#34771=CARTESIAN_POINT('Ctrl Pts',(-0.154553716617854,1.07385516829459E-5,
3.53957882764113));
#34772=CARTESIAN_POINT('Ctrl Pts',(-0.154554183576509,0.000527195138975443,
3.53955207027449));
#34773=CARTESIAN_POINT('Ctrl Pts',(-0.154317915988944,0.0521256879879336,
3.53687875288222));
#34774=CARTESIAN_POINT('Ctrl Pts',(-0.0973408901199132,0.154229940417525,
3.53155887546432));
#34775=CARTESIAN_POINT('Ctrl Pts',(0.0768181056158631,0.16543527210962,
3.52361919538745));
#34776=CARTESIAN_POINT('Ctrl Pts',(0.180643771975638,0.0251157687415861,
3.51567951531057));
#34777=CARTESIAN_POINT('Ctrl Pts',(0.119593430082514,-0.13672026231454,
3.50780645018142));
#34778=CARTESIAN_POINT('Ctrl Pts',(0.00819996357198913,-0.162114976519676,
3.5025799450779));
#34779=CARTESIAN_POINT('Ctrl Pts',(-0.0399398165374138,-0.14933059314829,
3.5));
#34780=CARTESIAN_POINT('Origin',(0.,0.,4.11042117235887));
#34781=CARTESIAN_POINT('',(-0.15419083216807,0.000129561635314926,3.58957882764113));
#34782=CARTESIAN_POINT('',(-0.154288256028425,-0.000141223516069758,3.58542117235887));
#34783=CARTESIAN_POINT('',(-0.1543,7.47606542906876E-15,4.11042117235887));
#34784=CARTESIAN_POINT('Ctrl Pts',(-0.154288256028425,-0.000141223516069763,
3.58542117235887));
#34785=CARTESIAN_POINT('Ctrl Pts',(-0.153932746614783,0.0387932487575316,
3.5834130484955));
#34786=CARTESIAN_POINT('Ctrl Pts',(-0.119227247372343,0.129604846059009,
3.57875836460651));
#34787=CARTESIAN_POINT('Ctrl Pts',(0.0333654249967142,0.179306991453011,
3.57145712069188));
#34788=CARTESIAN_POINT('Ctrl Pts',(0.16875469474836,0.0691889591605158,
3.56351744061501));
#34789=CARTESIAN_POINT('Ctrl Pts',(0.149631713131164,-0.104283094234219,
3.55557776053813));
#34790=CARTESIAN_POINT('Ctrl Pts',(-0.00648228852693025,-0.182263845309582,
3.54763808046125));
#34791=CARTESIAN_POINT('Ctrl Pts',(-0.133583343879226,-0.107056676726779,
3.54091921773484));
#34792=CARTESIAN_POINT('Ctrl Pts',(-0.154000066586259,-0.0277136758071254,
3.53684691503404));
#34793=CARTESIAN_POINT('Ctrl Pts',(-0.154050307343621,3.81371511608431E-5,
3.53542117235887));
#34794=CARTESIAN_POINT('Ctrl Pts',(-0.15419083216807,0.000129561635314916,
3.58957882764113));
#34795=CARTESIAN_POINT('Ctrl Pts',(-0.154316540000352,0.0159383321389732,
3.58876476376157));
#34796=CARTESIAN_POINT('Ctrl Pts',(-0.144808574808872,0.0829945710278969,
3.58530413985639));
#34797=CARTESIAN_POINT('Ctrl Pts',(-0.0479747871584019,0.175962994372803,
3.57919695592558));
#34798=CARTESIAN_POINT('Ctrl Pts',(0.121839171429706,0.13571993663382,3.5712572758487));
#34799=CARTESIAN_POINT('Ctrl Pts',(0.180099946935509,-0.0287862221383337,
3.56331759577183));
#34800=CARTESIAN_POINT('Ctrl Pts',(0.0734653204375665,-0.166934393666355,
3.55537791569495));
#34801=CARTESIAN_POINT('Ctrl Pts',(-0.0998464626320651,-0.152294592499083,
3.54746499298472));
#34802=CARTESIAN_POINT('Ctrl Pts',(-0.154507996889821,-0.0505553114913108,
3.54219863030011));
#34803=CARTESIAN_POINT('Ctrl Pts',(-0.154553716617854,1.07385516829459E-5,
3.53957882764113));
#34804=CARTESIAN_POINT('Origin',(0.,0.,4.11042117235887));
#34805=CARTESIAN_POINT('',(-0.154093198061062,-8.33060061860361E-5,3.63957882764113));
#34806=CARTESIAN_POINT('',(-0.154532949196129,5.22176212347235E-5,3.63542117235887));
#34807=CARTESIAN_POINT('',(-0.1543,7.47606542906876E-15,4.11042117235887));
#34808=CARTESIAN_POINT('Ctrl Pts',(-0.154532949196129,5.22176212347084E-5,
3.63542117235887));
#34809=CARTESIAN_POINT('Ctrl Pts',(-0.154545584588578,0.00292672178698735,
3.63527230200821));
#34810=CARTESIAN_POINT('Ctrl Pts',(-0.153169988902963,0.0568907246896308,
3.63247687163192));
#34811=CARTESIAN_POINT('Ctrl Pts',(-0.0901397813258339,0.158554191001936,
3.62703488123002));
#34812=CARTESIAN_POINT('Ctrl Pts',(0.0843490755327352,0.161709110561297,
3.61909520115314));
#34813=CARTESIAN_POINT('Ctrl Pts',(0.181609876119891,0.0168069020193158,
3.61115552107626));
#34814=CARTESIAN_POINT('Ctrl Pts',(0.11259272547993,-0.14348343554309,3.60321584099938));
#34815=CARTESIAN_POINT('Ctrl Pts',(-0.0595116136917225,-0.1724033835878,
3.59527616092251));
#34816=CARTESIAN_POINT('Ctrl Pts',(-0.147380741016298,-0.0760839947500021,
3.58934460470901));
#34817=CARTESIAN_POINT('Ctrl Pts',(-0.154401281957667,-0.0125195312047306,
3.58605960852113));
#34818=CARTESIAN_POINT('Ctrl Pts',(-0.154288256028425,-0.000141223516069763,
3.58542117235887));
#34819=CARTESIAN_POINT('Ctrl Pts',(-0.154093198061063,-8.33060061860274E-5,
3.63957882764113));
#34820=CARTESIAN_POINT('Ctrl Pts',(-0.153940587938977,0.0310641981069166,
3.63797745724865));
#34821=CARTESIAN_POINT('Ctrl Pts',(-0.129646233104354,0.113907608400038,
3.63372952683056));
#34822=CARTESIAN_POINT('Ctrl Pts',(0.00558664719359638,0.182300288895857,
3.62683503638684));
#34823=CARTESIAN_POINT('Ctrl Pts',(0.156205528517827,0.094151159125646,
3.61889535630996));
#34824=CARTESIAN_POINT('Ctrl Pts',(0.163806179027695,-0.0802006497663837,
3.61095567623308));
#34825=CARTESIAN_POINT('Ctrl Pts',(0.0214296163208854,-0.181122531330724,
3.60301599615621));
#34826=CARTESIAN_POINT('Ctrl Pts',(-0.123957687612568,-0.122868073634794,
3.59589037995889));
#34827=CARTESIAN_POINT('Ctrl Pts',(-0.1539078579151,-0.0354567255707862,
3.5914113237872));
#34828=CARTESIAN_POINT('Ctrl Pts',(-0.15419083216807,0.000129561635314916,
3.58957882764113));
#34829=CARTESIAN_POINT('Origin',(0.,0.,4.11042117235887));
#34830=CARTESIAN_POINT('',(-0.154494739391599,-8.56666717596894E-5,3.68957882764113));
#34831=CARTESIAN_POINT('',(-0.15413359010754,0.000108847378321225,3.68542117235887));
#34832=CARTESIAN_POINT('',(-0.1543,7.47606542906876E-15,4.11042117235887));
#34833=CARTESIAN_POINT('Ctrl Pts',(-0.15413359010754,0.00010884737832121,
3.68542117235887));
#34834=CARTESIAN_POINT('Ctrl Pts',(-0.154252061492927,0.0183060191525707,
3.6844849954953));
#34835=CARTESIAN_POINT('Ctrl Pts',(-0.142855501009428,0.0878027720491901,
3.6809022586061));
#34836=CARTESIAN_POINT('Ctrl Pts',(-0.039826269011209,0.177984489264188,
3.67467296169127));
#34837=CARTESIAN_POINT('Ctrl Pts',(0.127955809817362,0.129968921992697,
3.66673328161439));
#34838=CARTESIAN_POINT('Ctrl Pts',(0.178584458888466,-0.0370432344610292,
3.65879360153752));
#34839=CARTESIAN_POINT('Ctrl Pts',(0.0657052360091523,-0.170139449612234,
3.65085392146064));
#34840=CARTESIAN_POINT('Ctrl Pts',(-0.104087723049408,-0.147885095147454,
3.64306311173443));
#34841=CARTESIAN_POINT('Ctrl Pts',(-0.154320957425313,-0.0481751113503961,
3.63791886203384));
#34842=CARTESIAN_POINT('Ctrl Pts',(-0.154532949196129,5.22176212347084E-5,
3.63542117235887));
#34843=CARTESIAN_POINT('Ctrl Pts',(-0.154494739391599,-8.56666717596998E-5,
3.68957882764113));
#34844=CARTESIAN_POINT('Ctrl Pts',(-0.15418701910941,0.0460669561753479,
3.68719015073574));
#34845=CARTESIAN_POINT('Ctrl Pts',(-0.107714707332757,0.143892491682726,
3.68215491380472));
#34846=CARTESIAN_POINT('Ctrl Pts',(0.0586595287281965,0.172695299861449,
3.67447311684809));
#34847=CARTESIAN_POINT('Ctrl Pts',(0.176911729524118,0.0443491475303153,
3.66653343677121));
#34848=CARTESIAN_POINT('Ctrl Pts',(0.133187572742707,-0.124602076359984,
3.65859375669434));
#34849=CARTESIAN_POINT('Ctrl Pts',(-0.0324800977009374,-0.179470471240069,
3.65065407661746));
#34850=CARTESIAN_POINT('Ctrl Pts',(-0.140993802389242,-0.0920951181032393,
3.64431576693306));
#34851=CARTESIAN_POINT('Ctrl Pts',(-0.154192804322217,-0.0204127991394723,
3.64062401727428));
#34852=CARTESIAN_POINT('Ctrl Pts',(-0.154093198061063,-8.33060061860274E-5,
3.63957882764113));
#34853=CARTESIAN_POINT('Origin',(0.,0.,4.11042117235887));
#34854=CARTESIAN_POINT('',(-0.154352374546534,0.000136543067356262,3.73957882764113));
#34855=CARTESIAN_POINT('',(-0.154139174508622,-0.000111501026995055,3.73542117235887));
#34856=CARTESIAN_POINT('',(-0.1543,7.47606542906876E-15,4.11042117235887));
#34857=CARTESIAN_POINT('Ctrl Pts',(-0.154139174508622,-0.000111501026995059,
3.73542117235887));
#34858=CARTESIAN_POINT('Ctrl Pts',(-0.153915233552703,0.0333860868580806,
3.73369768898238));
#34859=CARTESIAN_POINT('Ctrl Pts',(-0.1267153517394,0.118653316414882,3.72932764558026));
#34860=CARTESIAN_POINT('Ctrl Pts',(0.0139700521550768,0.18185006934563,
3.72231104215253));
#34861=CARTESIAN_POINT('Ctrl Pts',(0.160372810275332,0.0868629483698537,
3.71437136207565));
#34862=CARTESIAN_POINT('Ctrl Pts',(0.15994186929589,-0.087653913339944,
3.70643168199877));
#34863=CARTESIAN_POINT('Ctrl Pts',(0.013071788942189,-0.181916844788939,
3.6984920019219));
#34864=CARTESIAN_POINT('Ctrl Pts',(-0.127037714877433,-0.11814535336758,
3.6914884987086));
#34865=CARTESIAN_POINT('Ctrl Pts',(-0.153917144400928,-0.0331371528280101,
3.68713155552092));
#34866=CARTESIAN_POINT('Ctrl Pts',(-0.15413359010754,0.00010884737832121,
3.68542117235887));
#34867=CARTESIAN_POINT('Ctrl Pts',(-0.154352374546534,0.000136543067356257,
3.73957882764113));
#34868=CARTESIAN_POINT('Ctrl Pts',(-0.154446737273245,0.0103903099163322,
3.73904940424845));
#34869=CARTESIAN_POINT('Ctrl Pts',(-0.148841316561083,0.0717994892151511,
3.73587342083015));
#34870=CARTESIAN_POINT('Ctrl Pts',(-0.0665446905722607,0.169812870767156,
3.73005087738622));
#34871=CARTESIAN_POINT('Ctrl Pts',(0.106602640202898,0.147988121222216,
3.72211119730934));
#34872=CARTESIAN_POINT('Ctrl Pts',(0.182147017152552,-0.0093311876933208,
3.71417151723247));
#34873=CARTESIAN_POINT('Ctrl Pts',(0.0909217261957518,-0.158107073301583,
3.70623183715559));
#34874=CARTESIAN_POINT('Ctrl Pts',(-0.0835494302172658,-0.162123717048593,
3.69829215707872));
#34875=CARTESIAN_POINT('Ctrl Pts',(-0.152048491522357,-0.0611528114853893,
3.69274115390723));
#34876=CARTESIAN_POINT('Ctrl Pts',(-0.154527961074428,-0.00506833400535766,
3.68983671076137));
#34877=CARTESIAN_POINT('Ctrl Pts',(-0.154494739391599,-8.56666717596998E-5,
3.68957882764113));
#34878=CARTESIAN_POINT('Origin',(0.,0.,4.11042117235887));
#34879=CARTESIAN_POINT('',(-0.154047977067031,2.09413777367551E-6,3.78957882764113));
#34880=CARTESIAN_POINT('',(-0.154536408180499,-4.7848165513455E-5,3.78542117235887));
#34881=CARTESIAN_POINT('',(-0.1543,7.47606542906876E-15,4.11042117235887));
#34882=CARTESIAN_POINT('Ctrl Pts',(-0.154536408180499,-4.78481655134459E-5,
3.78542117235887));
#34883=CARTESIAN_POINT('Ctrl Pts',(-0.154339106087067,0.0484295369338371,
3.78291038246947));
#34884=CARTESIAN_POINT('Ctrl Pts',(-0.103641790719782,0.148361335894058,
3.77775303255443));
#34885=CARTESIAN_POINT('Ctrl Pts',(0.0665446937287967,0.169812878822259,
3.76994912261378));
#34886=CARTESIAN_POINT('Ctrl Pts',(0.178765223990991,0.0361608181406009,
3.7620094425369));
#34887=CARTESIAN_POINT('Ctrl Pts',(0.127312379282745,-0.130599265535886,
3.75406976246003));
#34888=CARTESIAN_POINT('Ctrl Pts',(-0.0407047855299705,-0.177785630781348,
3.74613008238315));
#34889=CARTESIAN_POINT('Ctrl Pts',(-0.143071654254016,-0.0872869087240706,
3.73991388568277));
#34890=CARTESIAN_POINT('Ctrl Pts',(-0.154259114549828,-0.0180524000230757,
3.73634424900801));
#34891=CARTESIAN_POINT('Ctrl Pts',(-0.154139174508622,-0.000111501026995059,
3.73542117235887));
#34892=CARTESIAN_POINT('Ctrl Pts',(-0.154047977067031,2.09413777367898E-6,
3.78957882764113));
#34893=CARTESIAN_POINT('Ctrl Pts',(-0.154051078605937,0.0256319813134887,
3.78826209773554));
#34894=CARTESIAN_POINT('Ctrl Pts',(-0.135851564244815,0.102772493157479,
3.78429880780432));
#34895=CARTESIAN_POINT('Ctrl Pts',(-0.013970051492431,0.181850060719556,
3.77768895784748));
#34896=CARTESIAN_POINT('Ctrl Pts',(0.145223361235896,0.110339395832533,
3.7697492777706));
#34897=CARTESIAN_POINT('Ctrl Pts',(0.171453565975463,-0.0621955113766863,
3.76180959769372));
#34898=CARTESIAN_POINT('Ctrl Pts',(0.0407047835991549,-0.177785622348059,
3.75386991761685));
#34899=CARTESIAN_POINT('Ctrl Pts',(-0.11610887230377,-0.133745678862782,
3.74645966093265));
#34900=CARTESIAN_POINT('Ctrl Pts',(-0.153975022906486,-0.0408677376689339,
3.74169596427408));
#34901=CARTESIAN_POINT('Ctrl Pts',(-0.154352374546534,0.000136543067356257,
3.73957882764113));
#34902=CARTESIAN_POINT('Origin',(0.,0.,4.11042117235887));
#34903=CARTESIAN_POINT('',(-0.154344683817836,-0.000137602699895489,3.83957882764113));
#34904=CARTESIAN_POINT('',(-0.154280621254558,0.000141160201694546,3.83542117235887));
#34905=CARTESIAN_POINT('',(-0.1543,7.47606542906876E-15,4.11042117235887));
#34906=CARTESIAN_POINT('Ctrl Pts',(-0.154280621254558,0.000141160201694572,
3.83542117235887));
#34907=CARTESIAN_POINT('Ctrl Pts',(-0.154395390544122,0.0127750301081681,
3.83476963598218));
#34908=CARTESIAN_POINT('Ctrl Pts',(-0.147198204620896,0.0765990159781269,
3.83147153957986));
#34909=CARTESIAN_POINT('Ctrl Pts',(-0.0586595315107243,0.172695308053416,
3.82552688315191));
#34910=CARTESIAN_POINT('Ctrl Pts',(0.113300008356683,0.142925568707939,
3.81758720307504));
#34911=CARTESIAN_POINT('Ctrl Pts',(0.181524636378177,-0.0177035721096275,
3.80964752299816));
#34912=CARTESIAN_POINT('Ctrl Pts',(0.0835494341804624,-0.162123724738966,
3.80170784292129));
#34913=CARTESIAN_POINT('Ctrl Pts',(-0.0909217305086156,-0.158107080801413,
3.7937681628444));
#34914=CARTESIAN_POINT('Ctrl Pts',(-0.15329856504372,-0.056379054482583,
3.78833927265694));
#34915=CARTESIAN_POINT('Ctrl Pts',(-0.154547077226211,-0.00266924679639216,
3.78555694249509));
#34916=CARTESIAN_POINT('Ctrl Pts',(-0.154536408180499,-4.78481655134459E-5,
3.78542117235887));
#34917=CARTESIAN_POINT('Ctrl Pts',(-0.154344683817836,-0.000137602699895493,
3.83957882764113));
#34918=CARTESIAN_POINT('Ctrl Pts',(-0.153968758841032,0.0406181785207979,
3.83747479122262));
#34919=CARTESIAN_POINT('Ctrl Pts',(-0.11649114353226,0.133249851238064,
3.83272419477849));
#34920=CARTESIAN_POINT('Ctrl Pts',(0.039826267121788,0.177984480821945,
3.82532703830873));
#34921=CARTESIAN_POINT('Ctrl Pts',(0.171144313607041,0.063041501012073,
3.81738735823185));
#34922=CARTESIAN_POINT('Ctrl Pts',(0.145766517224248,-0.109620843643728,
3.80944767815498));
#34923=CARTESIAN_POINT('Ctrl Pts',(-0.0130717883220708,-0.181916836159762,
3.8015079980781));
#34924=CARTESIAN_POINT('Ctrl Pts',(-0.135584681571728,-0.103286631626578,
3.79488504790682));
#34925=CARTESIAN_POINT('Ctrl Pts',(-0.154044844670753,-0.0258827861209538,
3.79090865776116));
#34926=CARTESIAN_POINT('Ctrl Pts',(-0.154047977067031,2.09413777367898E-6,
3.78957882764113));
#34927=CARTESIAN_POINT('Origin',(0.,0.,4.11042117235887));
#34928=CARTESIAN_POINT('',(-0.154500132216325,8.19700297638587E-5,3.88957882764113));
#34929=CARTESIAN_POINT('',(-0.154055933642351,-3.65432311820964E-5,3.88542117235887));
#34930=CARTESIAN_POINT('',(-0.1543,7.47606542906876E-15,4.11042117235887));
#34931=CARTESIAN_POINT('Ctrl Pts',(-0.154055933642351,-3.6543231182122E-5,
3.88542117235887));
#34932=CARTESIAN_POINT('Ctrl Pts',(-0.15399662440304,0.0279666460980613,
3.88398232946926));
#34933=CARTESIAN_POINT('Ctrl Pts',(-0.133294661580101,0.10755966601202,
3.87989692655402));
#34934=CARTESIAN_POINT('Ctrl Pts',(-0.005586647457645,0.182300297549597,
3.87316496361317));
#34935=CARTESIAN_POINT('Ctrl Pts',(0.150147248343024,0.103539432915148,
3.86522528353629));
#34936=CARTESIAN_POINT('Ctrl Pts',(0.168409737102627,-0.0700197873807462,
3.85728560345941));
#34937=CARTESIAN_POINT('Ctrl Pts',(0.0324800992415292,-0.179470479754251,
3.84934592338254));
#34938=CARTESIAN_POINT('Ctrl Pts',(-0.1195927593937,-0.129104626018084,
3.84205777968236));
#34939=CARTESIAN_POINT('Ctrl Pts',(-0.153929194296616,-0.0385441229881096,
3.8374161960078));
#34940=CARTESIAN_POINT('Ctrl Pts',(-0.154280621254558,0.000141160201694572,
3.83542117235887));
#34941=CARTESIAN_POINT('Ctrl Pts',(-0.154500132216325,8.19700297638379E-5,
3.88957882764113));
#34942=CARTESIAN_POINT('Ctrl Pts',(-0.1545305647953,0.00481108885999716,
3.88933404473533));
#34943=CARTESIAN_POINT('Ctrl Pts',(-0.152188184006249,0.0606402533846132,
3.88644270180391));
#34944=CARTESIAN_POINT('Ctrl Pts',(-0.0843490715154628,0.161709102853824,
3.88090479884686));
#34945=CARTESIAN_POINT('Ctrl Pts',(0.0901397770410241,0.158554183500776,
3.87296511876998));
#34946=CARTESIAN_POINT('Ctrl Pts',(0.182098715355847,0.0102306290122647,
3.86502543869311));
#34947=CARTESIAN_POINT('Ctrl Pts',(0.107332199369115,-0.147459841777235,
3.85708575861623));
#34948=CARTESIAN_POINT('Ctrl Pts',(-0.0657052328909015,-0.17013944154474,
3.84914607853936));
#34949=CARTESIAN_POINT('Ctrl Pts',(-0.148671156397415,-0.0723140833987834,
3.84331043488099));
#34950=CARTESIAN_POINT('Ctrl Pts',(-0.154441615683002,-0.0106464385947012,
3.84012135124824));
#34951=CARTESIAN_POINT('Ctrl Pts',(-0.154344683817836,-0.000137602699895493,
3.83957882764113));
#34952=CARTESIAN_POINT('Origin',(0.,0.,4.11042117235887));
#34953=CARTESIAN_POINT('',(-0.154097159264761,8.62650376686758E-5,3.93957882764113));
#34954=CARTESIAN_POINT('',(-0.154414683966261,-0.000122711940234539,3.93542117235887));
#34955=CARTESIAN_POINT('',(-0.1543,7.47606542906876E-15,4.11042117235887));
#34956=CARTESIAN_POINT('Ctrl Pts',(-0.154414683966261,-0.00012271194023455,
3.93542117235887));
#34957=CARTESIAN_POINT('Ctrl Pts',(-0.15404065948349,0.0429479512135688,
3.93319502295635));
#34958=CARTESIAN_POINT('Ctrl Pts',(-0.11284743018063,0.1378508358131,3.9283223135282));
#34959=CARTESIAN_POINT('Ctrl Pts',(0.0479747894892283,0.175963002958517,
3.92080304407442));
#34960=CARTESIAN_POINT('Ctrl Pts',(0.173864125597012,0.0550988560374321,
3.91286336399754));
#34961=CARTESIAN_POINT('Ctrl Pts',(0.140567423109983,-0.116212816074597,
3.90492368392067));
#34962=CARTESIAN_POINT('Ctrl Pts',(-0.0214296173447312,-0.181122539961793,
3.89698400384379));
#34963=CARTESIAN_POINT('Ctrl Pts',(-0.138004452641611,-0.0984898965999405,
3.89048316665653));
#34964=CARTESIAN_POINT('Ctrl Pts',(-0.154105715856349,-0.0235414942304966,
3.88662888949489));
#34965=CARTESIAN_POINT('Ctrl Pts',(-0.154055933642351,-3.6543231182122E-5,
3.88542117235887));
#34966=CARTESIAN_POINT('Ctrl Pts',(-0.154097159264761,8.62650376686723E-5,
3.93957882764113));
#34967=CARTESIAN_POINT('Ctrl Pts',(-0.154199890802351,0.0201598980625174,
3.93854673822241));
#34968=CARTESIAN_POINT('Ctrl Pts',(-0.141224360537215,0.0915805799143205,
3.93486808877808));
#34969=CARTESIAN_POINT('Ctrl Pts',(-0.0333654229848094,0.179306981584077,
3.92854287930812));
#34970=CARTESIAN_POINT('Ctrl Pts',(0.132570265831228,0.125258780485074,
3.92060319923124));
#34971=CARTESIAN_POINT('Ctrl Pts',(0.17712875926901,-0.0434751369680033,
3.91266351915436));
#34972=CARTESIAN_POINT('Ctrl Pts',(0.059511610779771,-0.172403375181386,
3.90472383907749));
#34973=CARTESIAN_POINT('Ctrl Pts',(-0.107286687880009,-0.144375040164272,
3.89702894190641));
#34974=CARTESIAN_POINT('Ctrl Pts',(-0.154201531823291,-0.0463195111784584,
3.89198060476095));
#34975=CARTESIAN_POINT('Ctrl Pts',(-0.154500132216325,8.19700297638379E-5,
3.88957882764113));
#34976=CARTESIAN_POINT('Origin',(0.,0.,4.11042117235887));
#34977=CARTESIAN_POINT('',(-0.154145398954164,-0.00018319008806407,3.98957882764113));
#34978=CARTESIAN_POINT('',(-0.154443265232512,0.000108744696557919,3.98542117235887));
#34979=CARTESIAN_POINT('',(-0.1543,7.47606542906876E-15,4.11042117235887));
#34980=CARTESIAN_POINT('',(-0.0398513841857263,-0.149064942821851,4.));
#34981=CARTESIAN_POINT('Ctrl Pts',(-0.0398513841857263,-0.149064942821851,
4.));
#34982=CARTESIAN_POINT('Ctrl Pts',(-0.0894268873061843,-0.13581130730129,
3.99735343997437));
#34983=CARTESIAN_POINT('Ctrl Pts',(-0.144571567721208,-0.0835405737349159,
3.99387971585475));
#34984=CARTESIAN_POINT('Ctrl Pts',(-0.154267320225706,-0.0162511224334367,
3.99040599173513));
#34985=CARTESIAN_POINT('Ctrl Pts',(-0.154145398954164,-0.000183190088064077,
3.98957882764113));
#34986=CARTESIAN_POINT('',(0.0399397509085001,-0.149330346493117,4.));
#34987=CARTESIAN_POINT('Origin',(0.,0.,4.));
#34988=CARTESIAN_POINT('Ctrl Pts',(0.0399398308045223,-0.149330586455588,
4.));
#34989=CARTESIAN_POINT('Ctrl Pts',(-0.00819994193508078,-0.162114963086391,
3.9974200549221));
#34990=CARTESIAN_POINT('Ctrl Pts',(-0.111773735607764,-0.138502981643238,
3.99256044570839));
#34991=CARTESIAN_POINT('Ctrl Pts',(-0.154082201487749,-0.0439653055987776,
3.98770083649468));
#34992=CARTESIAN_POINT('Ctrl Pts',(-0.154443265232512,0.000108744696557906,
3.98542117235887));
#34993=CARTESIAN_POINT('Origin',(-1.70916393953233E-17,-6.81365885416763E-18,
3.5));
#34994=CARTESIAN_POINT('Ctrl Pts',(-0.0958116152722498,0.0825211298936362,
3.5));
#34995=CARTESIAN_POINT('Ctrl Pts',(-0.100695982673166,0.0779597798732974,
3.5));
#34996=CARTESIAN_POINT('Ctrl Pts',(-0.105169094336774,0.073000191113619,
3.5));
#34997=CARTESIAN_POINT('Ctrl Pts',(-0.109227190160158,0.0677117533966587,
3.5));
#34998=CARTESIAN_POINT('Ctrl Pts',(-0.111694873825402,0.0644959122887171,
3.5));
#34999=CARTESIAN_POINT('Ctrl Pts',(-0.114010184214277,0.0611562073506752,
3.5));
#35000=CARTESIAN_POINT('Ctrl Pts',(-0.116166807098829,0.0577125335531249,
3.5));
#35001=CARTESIAN_POINT('Ctrl Pts',(-0.121431726365849,0.0493055632589991,
3.5));
#35002=CARTESIAN_POINT('Ctrl Pts',(-0.12573464769667,0.0403151423737322,
3.5));
#35003=CARTESIAN_POINT('Ctrl Pts',(-0.129045466546674,0.0309386517006337,
3.5));
#35004=CARTESIAN_POINT('Ctrl Pts',(-0.130207164312345,0.0276486353154881,
3.5));
#35005=CARTESIAN_POINT('Ctrl Pts',(-0.131243087485824,0.0243197585947972,
3.5));
#35006=CARTESIAN_POINT('Ctrl Pts',(-0.132152263806834,0.0209620064696601,
3.5));
#35007=CARTESIAN_POINT('Ctrl Pts',(-0.134828933182204,0.0110765837240964,
3.5));
#35008=CARTESIAN_POINT('Ctrl Pts',(-0.136412178238084,0.000939292992310017,
3.5));
#35009=CARTESIAN_POINT('Ctrl Pts',(-0.136856372906323,-0.00925247465139327,
3.5));
#35010=CARTESIAN_POINT('Ctrl Pts',(-0.137021913483504,-0.0130506992112034,
3.5));
#35011=CARTESIAN_POINT('Ctrl Pts',(-0.137028726314264,-0.0168567537781713,
3.5));
#35012=CARTESIAN_POINT('Ctrl Pts',(-0.136872398016052,-0.0206609891299379,
3.5));
#35013=CARTESIAN_POINT('Ctrl Pts',(-0.136740582821431,-0.0238687002674301,
3.5));
#35014=CARTESIAN_POINT('Ctrl Pts',(-0.136493094718847,-0.0270653690856263,
3.5));
#35015=CARTESIAN_POINT('Ctrl Pts',(-0.13612917734588,-0.0302430275614766,
3.5));
#35016=CARTESIAN_POINT('Ctrl Pts',(-0.13576659429471,-0.0334090349888054,
3.5));
#35017=CARTESIAN_POINT('Ctrl Pts',(-0.135288410857674,-0.0365568188154616,
3.5));
#35018=CARTESIAN_POINT('Ctrl Pts',(-0.134693327673148,-0.0396806409761667,
3.5));
#35019=CARTESIAN_POINT('Ctrl Pts',(-0.133341599676801,-0.0467763848654778,
3.5));
#35020=CARTESIAN_POINT('Ctrl Pts',(-0.131387825400402,-0.0537485551880799,
3.5));
#35021=CARTESIAN_POINT('Ctrl Pts',(-0.128888271219693,-0.0605519919600177,
3.5));
#35022=CARTESIAN_POINT('Ctrl Pts',(-0.127520602506107,-0.0642745948504241,
3.5));
#35023=CARTESIAN_POINT('Ctrl Pts',(-0.125989250183059,-0.0679466858359917,
3.5));
#35024=CARTESIAN_POINT('Ctrl Pts',(-0.124301567034569,-0.0715605953668731,
3.5));
#35025=CARTESIAN_POINT('Ctrl Pts',(-0.123083413065749,-0.0741690815877246,
3.5));
#35026=CARTESIAN_POINT('Ctrl Pts',(-0.121784536276434,-0.0767452222753887,
3.5));
#35027=CARTESIAN_POINT('Ctrl Pts',(-0.120412533496435,-0.0792783080753084,
3.5));
#35028=CARTESIAN_POINT('Ctrl Pts',(-0.116240621079353,-0.0869807794232376,
3.5));
#35029=CARTESIAN_POINT('Ctrl Pts',(-0.111384900653015,-0.0943068033536031,
3.5));
#35030=CARTESIAN_POINT('Ctrl Pts',(-0.105936294580107,-0.101180758720708,
3.5));
#35031=CARTESIAN_POINT('Ctrl Pts',(-0.102498213514854,-0.105518237972245,
3.5));
#35032=CARTESIAN_POINT('Ctrl Pts',(-0.0988234872002696,-0.109675688132788,
3.5));
#35033=CARTESIAN_POINT('Ctrl Pts',(-0.0949300211352312,-0.113632240993693,
3.5));
#35034=CARTESIAN_POINT('Ctrl Pts',(-0.0916236146803262,-0.116992221972066,
3.5));
#35035=CARTESIAN_POINT('Ctrl Pts',(-0.0881545091528211,-0.120210812929281,
3.5));
#35036=CARTESIAN_POINT('Ctrl Pts',(-0.0845585132916744,-0.123253141705618,
3.5));
#35037=CARTESIAN_POINT('Ctrl Pts',(-0.0763242263006133,-0.13021961475866,
3.5));
#35038=CARTESIAN_POINT('Ctrl Pts',(-0.0674109291876633,-0.136284624413674,
3.5));
#35039=CARTESIAN_POINT('Ctrl Pts',(-0.0579550193346048,-0.141304740223277,
3.5));
#35040=CARTESIAN_POINT('Ctrl Pts',(-0.0532842084112166,-0.143784460538354,
3.5));
#35041=CARTESIAN_POINT('Ctrl Pts',(-0.0484803425336181,-0.146008805046434,
3.5));
#35042=CARTESIAN_POINT('Ctrl Pts',(-0.0435567265409999,-0.147956912059339,
3.5));
#35043=CARTESIAN_POINT('Ctrl Pts',(-0.042358096554505,-0.148431169086302,
3.5));
#35044=CARTESIAN_POINT('Ctrl Pts',(-0.0411523620931259,-0.148889040418797,
3.5));
#35045=CARTESIAN_POINT('Ctrl Pts',(-0.0399398165374117,-0.14933059314829,
3.5));
#35046=CARTESIAN_POINT('Ctrl Pts',(0.0398513841857336,-0.149064942821849,
3.5));
#35047=CARTESIAN_POINT('Ctrl Pts',(0.0462529496128914,-0.146725837162888,
3.5));
#35048=CARTESIAN_POINT('Ctrl Pts',(0.0524692076951892,-0.14393427563735,
3.5));
#35049=CARTESIAN_POINT('Ctrl Pts',(0.0584702623153416,-0.140728485236784,
3.5));
#35050=CARTESIAN_POINT('Ctrl Pts',(0.0631250229031883,-0.138241891170577,
3.5));
#35051=CARTESIAN_POINT('Ctrl Pts',(0.0676502468975603,-0.1355058910355,
3.5));
#35052=CARTESIAN_POINT('Ctrl Pts',(0.0720296458894365,-0.132535875720451,
3.5));
#35053=CARTESIAN_POINT('Ctrl Pts',(0.0754784967726087,-0.130196938354537,
3.5));
#35054=CARTESIAN_POINT('Ctrl Pts',(0.0788293975632557,-0.127717841671465,
3.5));
#35055=CARTESIAN_POINT('Ctrl Pts',(0.0820734025861846,-0.125108353169529,
3.5));
#35056=CARTESIAN_POINT('Ctrl Pts',(0.0878699486728443,-0.120445592089575,
3.5));
#35057=CARTESIAN_POINT('Ctrl Pts',(0.0933277488655726,-0.115365506062939,
3.5));
#35058=CARTESIAN_POINT('Ctrl Pts',(0.0983983261001443,-0.109911369421357,
3.5));
#35059=CARTESIAN_POINT('Ctrl Pts',(0.100785232866561,-0.107343907167555,
3.5));
#35060=CARTESIAN_POINT('Ctrl Pts',(0.103082837759472,-0.104696811464977,
3.5));
#35061=CARTESIAN_POINT('Ctrl Pts',(0.105281553373082,-0.101981102913922,
3.5));
#35062=CARTESIAN_POINT('Ctrl Pts',(0.111767020079616,-0.0939706820648148,
3.5));
#35063=CARTESIAN_POINT('Ctrl Pts',(0.117410242387804,-0.0853491014404185,
3.5));
#35064=CARTESIAN_POINT('Ctrl Pts',(0.122076804303227,-0.0762334533122014,
3.5));
#35065=CARTESIAN_POINT('Ctrl Pts',(0.124156859535273,-0.0721702796253988,
3.5));
#35066=CARTESIAN_POINT('Ctrl Pts',(0.126042226032514,-0.0680087185900064,
3.5));
#35067=CARTESIAN_POINT('Ctrl Pts',(0.127717516401833,-0.0637585923271345,
3.5));
#35068=CARTESIAN_POINT('Ctrl Pts',(0.128878955464437,-0.0608120806339354,
3.5));
#35069=CARTESIAN_POINT('Ctrl Pts',(0.129938690733468,-0.0578239271836136,
3.5));
#35070=CARTESIAN_POINT('Ctrl Pts',(0.130888204891735,-0.0548097446101512,
3.5));
#35071=CARTESIAN_POINT('Ctrl Pts',(0.132091470075251,-0.0509900428017762,
3.5));
#35072=CARTESIAN_POINT('Ctrl Pts',(0.133119907502104,-0.0471234083998808,
3.5));
#35073=CARTESIAN_POINT('Ctrl Pts',(0.13396498302397,-0.0432168875268929,
3.5));
#35074=CARTESIAN_POINT('Ctrl Pts',(0.135449870731708,-0.03635271423797,
3.5));
#35075=CARTESIAN_POINT('Ctrl Pts',(0.136369320260194,-0.0293652097985063,
3.5));
#35076=CARTESIAN_POINT('Ctrl Pts',(0.136739868479968,-0.022319296125407,
3.5));
#35077=CARTESIAN_POINT('Ctrl Pts',(0.136938614931574,-0.0185401649189451,
3.5));
#35078=CARTESIAN_POINT('Ctrl Pts',(0.13697923643291,-0.0147442545690828,
3.5));
#35079=CARTESIAN_POINT('Ctrl Pts',(0.136862895918197,-0.0109420689853019,
3.5));
#35080=CARTESIAN_POINT('Ctrl Pts',(0.136768618157157,-0.00786092786453014,
3.5));
#35081=CARTESIAN_POINT('Ctrl Pts',(0.136571008887471,-0.00477673741219634,
3.5));
#35082=CARTESIAN_POINT('Ctrl Pts',(0.136272480032331,-0.00170755776859209,
3.5));
#35083=CARTESIAN_POINT('Ctrl Pts',(0.135524862167375,0.00597871273026037,
3.5));
#35084=CARTESIAN_POINT('Ctrl Pts',(0.134145273604047,0.0135925891081728,
3.5));
#35085=CARTESIAN_POINT('Ctrl Pts',(0.132154756111308,0.0210469694652312,
3.5));
#35086=CARTESIAN_POINT('Ctrl Pts',(0.130956639638983,0.0255338508563019,
3.5));
#35087=CARTESIAN_POINT('Ctrl Pts',(0.129536820205507,0.0299628465144204,
3.5));
#35088=CARTESIAN_POINT('Ctrl Pts',(0.127896985354882,0.0343130630344241,
3.5));
#35089=CARTESIAN_POINT('Ctrl Pts',(0.126764260724531,0.0373179981946284,
3.5));
#35090=CARTESIAN_POINT('Ctrl Pts',(0.125525608395292,0.0402872565072415,
3.5));
#35091=CARTESIAN_POINT('Ctrl Pts',(0.124183958141022,0.0432071171955597,
3.5));
#35092=CARTESIAN_POINT('Ctrl Pts',(0.120305951421964,0.0516469019546402,
3.5));
#35093=CARTESIAN_POINT('Ctrl Pts',(0.115595095267004,0.0596252551381628,
3.5));
#35094=CARTESIAN_POINT('Ctrl Pts',(0.110076005567125,0.0669787038662309,
3.5));
#35095=CARTESIAN_POINT('Ctrl Pts',(0.106491490638639,0.0717545905024268,
3.5));
#35096=CARTESIAN_POINT('Ctrl Pts',(0.102565240148127,0.0762663779558996,
3.5));
#35097=CARTESIAN_POINT('Ctrl Pts',(0.0982968917172504,0.0804596491219306,
3.5));
#35098=CARTESIAN_POINT('Ctrl Pts',(0.0975400014439711,0.081203226224454,
3.5));
#35099=CARTESIAN_POINT('Ctrl Pts',(0.0967723418961243,0.0819367632413509,
3.5));
#35100=CARTESIAN_POINT('Ctrl Pts',(0.0959941578858439,0.0826601402795114,
3.5));
#35101=CARTESIAN_POINT('Origin',(0.,0.,4.11042117235887));
#35102=CARTESIAN_POINT('Ctrl Pts',(-0.154443265232512,0.000108744696557909,
3.98542117235887));
#35103=CARTESIAN_POINT('Ctrl Pts',(-0.154501375899708,0.00720215273278324,
3.98505427646906));
#35104=CARTESIAN_POINT('Ctrl Pts',(-0.150833043785448,0.0654047280234095,
3.98204082055362));
#35105=CARTESIAN_POINT('Ctrl Pts',(-0.0768181153328184,0.165435267997838,
3.97638080461255));
#35106=CARTESIAN_POINT('Ctrl Pts',(0.0973408978391562,0.154229954870798,
3.96844112453568));
#35107=CARTESIAN_POINT('Ctrl Pts',(0.182376570303567,0.00184388772387479,
3.9605014444588));
#35108=CARTESIAN_POINT('Ctrl Pts',(0.100432518024861,-0.152245093163996,
3.95256176438192));
#35109=CARTESIAN_POINT('Ctrl Pts',(-0.0734653243360244,-0.166934402953208,
3.94462208430505));
#35110=CARTESIAN_POINT('Ctrl Pts',(-0.150201443282177,-0.0675205906017345,
3.9389085536307));
#35111=CARTESIAN_POINT('Ctrl Pts',(-0.154485318877682,-0.00825665133948968,
3.93584158298197));
#35112=CARTESIAN_POINT('Ctrl Pts',(-0.154414683966261,-0.00012271194023455,
3.93542117235887));
#35113=CARTESIAN_POINT('Ctrl Pts',(-0.154145398954164,-0.000183190088064077,
3.98957882764113));
#35114=CARTESIAN_POINT('Ctrl Pts',(-0.153877225967651,0.0351591693674689,
3.9877594317095));
#35115=CARTESIAN_POINT('Ctrl Pts',(-0.124353035696744,0.122445639808398,
3.98329347575225));
#35116=CARTESIAN_POINT('Ctrl Pts',(0.0205691872966891,0.181176549232701,
3.97618095976937));
#35117=CARTESIAN_POINT('Ctrl Pts',(0.16339053139201,0.0810339956098913,
3.9682412796925));
#35118=CARTESIAN_POINT('Ctrl Pts',(0.156677599794682,-0.0933915431448235,
3.96030159961562));
#35119=CARTESIAN_POINT('Ctrl Pts',(0.00648228676056323,-0.182263829019595,
3.95236191953875));
#35120=CARTESIAN_POINT('Ctrl Pts',(-0.129338242603737,-0.114419911622588,
3.94545432888058));
#35121=CARTESIAN_POINT('Ctrl Pts',(-0.153936458995158,-0.0313143964796836,
3.94119329824804));
#35122=CARTESIAN_POINT('Ctrl Pts',(-0.154097159264761,8.62650376686723E-5,
3.93957882764113));
#35123=CARTESIAN_POINT('Ctrl Pts',(0.095811615272233,0.0825211298936557,
4.));
#35124=CARTESIAN_POINT('Ctrl Pts',(0.123256207240687,0.0506564342651108,
3.99735343997437));
#35125=CARTESIAN_POINT('Ctrl Pts',(0.143368215702842,-0.042067892211591,
3.99206031992312));
#35126=CARTESIAN_POINT('Ctrl Pts',(0.0422170408642446,-0.143478264550263,
3.98412063984626));
#35127=CARTESIAN_POINT('Ctrl Pts',(-0.0975844110283061,-0.113165467831369,
3.97618095976937));
#35128=CARTESIAN_POINT('Ctrl Pts',(-0.148038914743343,0.0205825766583269,
3.9682412796925));
#35129=CARTESIAN_POINT('Ctrl Pts',(-0.0629530180417037,0.135575435115532,
3.96030159961561));
#35130=CARTESIAN_POINT('Ctrl Pts',(0.0797715912622248,0.126392597494572,
3.95236191953875));
#35131=CARTESIAN_POINT('Ctrl Pts',(0.149458958618833,0.00151107973223563,
3.94442223946186));
#35132=CARTESIAN_POINT('Ctrl Pts',(0.0823051970462972,-0.124765988532646,
3.936482559385));
#35133=CARTESIAN_POINT('Ctrl Pts',(-0.0602053808314341,-0.136803987384531,
3.92854287930812));
#35134=CARTESIAN_POINT('Ctrl Pts',(-0.147593255628917,-0.0235905240738923,
3.92060319923124));
#35135=CARTESIAN_POINT('Ctrl Pts',(-0.0998481138804565,0.11122350451698,
3.91266351915437));
#35136=CARTESIAN_POINT('Ctrl Pts',(0.0393156975431816,0.144202992379161,
3.90472383907749));
#35137=CARTESIAN_POINT('Ctrl Pts',(0.142482946738445,0.0451539231751995,
3.89678415900061));
#35138=CARTESIAN_POINT('Ctrl Pts',(0.115196050889548,-0.0952372689088321,
3.88884447892374));
#35139=CARTESIAN_POINT('Ctrl Pts',(-0.0175617311292369,-0.148431271407445,
3.88090479884687));
#35140=CARTESIAN_POINT('Ctrl Pts',(-0.134240390927499,-0.0657250333201687,
3.87296511876998));
#35141=CARTESIAN_POINT('Ctrl Pts',(-0.128011600896121,0.0771575802637476,
3.86502543869311));
#35142=CARTESIAN_POINT('Ctrl Pts',(-0.00457829922889965,0.149396452528493,
3.85708575861623));
#35143=CARTESIAN_POINT('Ctrl Pts',(0.123046789066594,0.0848513369547663,
3.84914607853936));
#35144=CARTESIAN_POINT('Ctrl Pts',(0.138013034715666,-0.0573817376169498,
3.84120639846248));
#35145=CARTESIAN_POINT('Ctrl Pts',(0.0266176834030549,-0.147077395754537,
3.83326671838561));
#35146=CARTESIAN_POINT('Ctrl Pts',(-0.109148213688832,-0.102112335081275,
3.82532703830873));
#35147=CARTESIAN_POINT('Ctrl Pts',(-0.144980487747744,0.0363444586596486,
3.81738735823185));
#35148=CARTESIAN_POINT('Ctrl Pts',(-0.0480719232633252,0.141525092050256,
3.80944767815498));
#35149=CARTESIAN_POINT('Ctrl Pts',(0.0928502012748058,0.117128568782365,
3.8015079980781));
#35150=CARTESIAN_POINT('Ctrl Pts',(0.148760792417501,-0.0145082092888036,
3.79356831800123));
#35151=CARTESIAN_POINT('Ctrl Pts',(0.0684693840059589,-0.13286160073391,
3.78562863792435));
#35152=CARTESIAN_POINT('Ctrl Pts',(-0.0745110357927053,-0.129569931090983,
3.77768895784747));
#35153=CARTESIAN_POINT('Ctrl Pts',(-0.149270845181396,-0.00764697822290441,
3.7697492777706));
#35154=CARTESIAN_POINT('Ctrl Pts',(-0.0873616623012301,0.121277374051889,
3.76180959769372));
#35155=CARTESIAN_POINT('Ctrl Pts',(0.0545338724692569,0.139162919812538,
3.75386991761685));
#35156=CARTESIAN_POINT('Ctrl Pts',(0.146499433400264,0.0296340599732921,
3.74593023753997));
#35157=CARTESIAN_POINT('Ctrl Pts',(0.104333443683106,-0.107027071464762,
3.7379905574631));
#35158=CARTESIAN_POINT('Ctrl Pts',(-0.0333578751151315,-0.14569664946404,
3.73005087738622));
#35159=CARTESIAN_POINT('Ctrl Pts',(-0.14050748182764,-0.0509696875349592,
3.72211119730934));
#35160=CARTESIAN_POINT('Ctrl Pts',(-0.119011632529845,0.0904239615350441,
3.71417151723247));
#35161=CARTESIAN_POINT('Ctrl Pts',(0.0114485618600744,0.149027487159785,
3.70623183715559));
#35162=CARTESIAN_POINT('Ctrl Pts',(0.131426713281372,0.0711848335798314,
3.69829215707872));
#35163=CARTESIAN_POINT('Ctrl Pts',(0.131073553936911,-0.0718330352678932,
3.69035247700184));
#35164=CARTESIAN_POINT('Ctrl Pts',(0.0107124284623447,-0.149082210133256,
3.68241279692496));
#35165=CARTESIAN_POINT('Ctrl Pts',(-0.119456752931603,-0.0898351026331364,
3.67447311684809));
#35166=CARTESIAN_POINT('Ctrl Pts',(-0.140254047194737,0.0516629823793918,
3.66653343677121));
#35167=CARTESIAN_POINT('Ctrl Pts',(-0.0326379242804108,0.145859615472823,
3.65859375669434));
#35168=CARTESIAN_POINT('Ctrl Pts',(0.10486073980172,0.10651050023316,3.65065407661746));
#35169=CARTESIAN_POINT('Ctrl Pts',(0.146351295051501,-0.0303572067245441,
3.64271439654059));
#35170=CARTESIAN_POINT('Ctrl Pts',(0.0538459306115186,-0.139430547008859,
3.63477471646371));
#35171=CARTESIAN_POINT('Ctrl Pts',(-0.0879595415059408,-0.12084444509365,
3.62683503638684));
#35172=CARTESIAN_POINT('Ctrl Pts',(-0.149231261493045,0.00838407713103302,
3.61889535630996));
#35173=CARTESIAN_POINT('Ctrl Pts',(-0.0738702226095378,0.12993634123263,
3.61095567623308));
#35174=CARTESIAN_POINT('Ctrl Pts',(0.0691246960538845,0.132521821325185,
3.60301599615621));
#35175=CARTESIAN_POINT('Ctrl Pts',(0.148830647021129,0.0137733814668988,
3.59507631607933));
#35176=CARTESIAN_POINT('Ctrl Pts',(0.0922705776859184,-0.11758574481156,
3.58713663600245));
#35177=CARTESIAN_POINT('Ctrl Pts',(-0.0487702109612334,-0.141285857774966,
3.57919695592558));
#35178=CARTESIAN_POINT('Ctrl Pts',(-0.145158345123895,-0.0356282001147357,
3.5712572758487));
#35179=CARTESIAN_POINT('Ctrl Pts',(-0.108642326262961,0.10265050841275,
3.56331759577183));
#35180=CARTESIAN_POINT('Ctrl Pts',(0.0273432144577738,0.14694341587319,
3.55537791569495));
#35181=CARTESIAN_POINT('Ctrl Pts',(0.138295730077318,0.0567008676982971,
3.54743823561807));
#35182=CARTESIAN_POINT('Ctrl Pts',(0.122624304118183,-0.0854607729482632,
3.5394985555412));
#35183=CARTESIAN_POINT('Ctrl Pts',(-0.00531228376040394,-0.149366579646122,
3.53155887546432));
#35184=CARTESIAN_POINT('Ctrl Pts',(-0.128398465432132,-0.0765350583850204,
3.52361919538745));
#35185=CARTESIAN_POINT('Ctrl Pts',(-0.133899765542225,0.0664079477775043,
3.51567951531057));
#35186=CARTESIAN_POINT('Ctrl Pts',(-0.0168566046022346,0.148475571278638,
3.5077398352337));
#35187=CARTESIAN_POINT('Ctrl Pts',(0.115720245650148,0.0947476421044766,
3.49980015515682));
#35188=CARTESIAN_POINT('Ctrl Pts',(0.142146925240749,-0.0460261281615502,
3.49186047507995));
#35189=CARTESIAN_POINT('Ctrl Pts',(0.0732860006472317,-0.111298378536925,
3.48656735502869));
#35190=CARTESIAN_POINT('Ctrl Pts',(0.0326585063531174,-0.122159831625553,
3.48392079500307));
#35191=CARTESIAN_POINT('Ctrl Pts',(0.102845629995659,0.0885794229410745,
4.00535973499898));
#35192=CARTESIAN_POINT('Ctrl Pts',(0.132305068112318,0.0543753790239966,
4.00271317497335));
#35193=CARTESIAN_POINT('Ctrl Pts',(0.153893600722808,-0.0451563087084747,
3.9974200549221));
#35194=CARTESIAN_POINT('Ctrl Pts',(0.0453164071172279,-0.154011728812092,
3.98948037484522));
#35195=CARTESIAN_POINT('Ctrl Pts',(-0.104748575644461,-0.121473516543913,
3.98154069476835));
#35196=CARTESIAN_POINT('Ctrl Pts',(-0.158907199376537,0.0220936475952833,
3.97360101469147));
#35197=CARTESIAN_POINT('Ctrl Pts',(-0.067574717138742,0.145528712742967,
3.9656613346146));
#35198=CARTESIAN_POINT('Ctrl Pts',(0.0856280267878686,0.135671716619981,
3.95772165453772));
#35199=CARTESIAN_POINT('Ctrl Pts',(0.160431495847078,0.00162201572944855,
3.94978197446085));
#35200=CARTESIAN_POINT('Ctrl Pts',(0.0883476373724852,-0.133925690076429,
3.94184229438397));
#35201=CARTESIAN_POINT('Ctrl Pts',(-0.0646253619996309,-0.146847459240757,
3.93390261430709));
#35202=CARTESIAN_POINT('Ctrl Pts',(-0.158428822175023,-0.0253224236269645,
3.92596293423022));
#35203=CARTESIAN_POINT('Ctrl Pts',(-0.107178468359357,0.119388983891694,
3.91802325415334));
#35204=CARTESIAN_POINT('Ctrl Pts',(0.0422020615251973,0.15478966257228,
3.91008357407647));
#35205=CARTESIAN_POINT('Ctrl Pts',(0.152943339691301,0.0484689007959436,
3.90214389399959));
#35206=CARTESIAN_POINT('Ctrl Pts',(0.123653174963026,-0.102229117964087,
3.89420421392272));
#35207=CARTESIAN_POINT('Ctrl Pts',(-0.0188510265344017,-0.159328360925561,
3.88626453384584));
#35208=CARTESIAN_POINT('Ctrl Pts',(-0.144095656216364,-0.0705502400631941,
3.87832485376896));
#35209=CARTESIAN_POINT('Ctrl Pts',(-0.137409579240545,0.0828221080358456,
3.87038517369209));
#35210=CARTESIAN_POINT('Ctrl Pts',(-0.00491441530514796,0.160364400868861,
3.86244549361521));
#35211=CARTESIAN_POINT('Ctrl Pts',(0.13208027549207,0.0910807022748934,
3.85450581353834));
#35212=CARTESIAN_POINT('Ctrl Pts',(0.148145268844653,-0.0615944208715485,
3.84656613346146));
#35213=CARTESIAN_POINT('Ctrl Pts',(0.0285718220158795,-0.157875090421108,
3.83862645338458));
#35214=CARTESIAN_POINT('Ctrl Pts',(-0.117161335479353,-0.109608917477515,
3.83068677330771));
#35215=CARTESIAN_POINT('Ctrl Pts',(-0.155624237803826,0.0390126889843388,
3.82274709323083));
#35216=CARTESIAN_POINT('Ctrl Pts',(-0.0516011260124583,0.151915164051309,
3.81480741315396));
#35217=CARTESIAN_POINT('Ctrl Pts',(0.0996668036354316,0.125727568757556,
3.80686773307708));
#35218=CARTESIAN_POINT('Ctrl Pts',(0.159682073737726,-0.0155733302290782,
3.7989280530002));
#35219=CARTESIAN_POINT('Ctrl Pts',(0.0734960673974602,-0.142615642068929,
3.79098837292333));
#35220=CARTESIAN_POINT('Ctrl Pts',(-0.0799812673646754,-0.139082314327793,
3.78304869284645));
#35221=CARTESIAN_POINT('Ctrl Pts',(-0.160229572051837,-0.00820838152726148,
3.77510901276958));
#35222=CARTESIAN_POINT('Ctrl Pts',(-0.0937753232873622,0.13018095878194,
3.7671693326927));
#35223=CARTESIAN_POINT('Ctrl Pts',(0.0585374795557702,0.149379572815778,
3.75922965261583));
#35224=CARTESIAN_POINT('Ctrl Pts',(0.157254696930506,0.0318096460290618,
3.75128997253895));
#35225=CARTESIAN_POINT('Ctrl Pts',(0.111993088882986,-0.11488446948847,
3.74335029246207));
#35226=CARTESIAN_POINT('Ctrl Pts',(-0.0358068452534112,-0.156392976569809,
3.7354106123852));
#35227=CARTESIAN_POINT('Ctrl Pts',(-0.15082284592122,-0.0547116297989597,
3.72747093230832));
#35228=CARTESIAN_POINT('Ctrl Pts',(-0.127748877728095,0.0970624413788584,
3.71953125223145));
#35229=CARTESIAN_POINT('Ctrl Pts',(0.0122890586250752,0.1599683478884,3.71159157215457));
#35230=CARTESIAN_POINT('Ctrl Pts',(0.141075412279359,0.0764108718431722,
3.7036518920777));
#35231=CARTESIAN_POINT('Ctrl Pts',(0.140696325723237,-0.0771066612919101,
3.69571221200082));
#35232=CARTESIAN_POINT('Ctrl Pts',(0.0114988819556263,-0.160027088351817,
3.68777253192394));
#35233=CARTESIAN_POINT('Ctrl Pts',(-0.128226676667323,-0.0964303513700096,
3.67983285184707));
#35234=CARTESIAN_POINT('Ctrl Pts',(-0.150550805371548,0.0554558229204912,
3.67189317177019));
#35235=CARTESIAN_POINT('Ctrl Pts',(-0.035034039190677,0.156567906736611,
3.66395349169332));
#35236=CARTESIAN_POINT('Ctrl Pts',(0.112559096473601,0.114329974153006,
3.65601381161644));
#35237=CARTESIAN_POINT('Ctrl Pts',(0.157095682997156,-0.0325858826367059,
3.64807413153956));
#35238=CARTESIAN_POINT('Ctrl Pts',(0.0577990324107298,-0.14966684787665,
3.64013445146269));
#35239=CARTESIAN_POINT('Ctrl Pts',(-0.0944170958250141,-0.129716246321693,
3.63219477138581));
#35240=CARTESIAN_POINT('Ctrl Pts',(-0.160187082324945,0.00899959459010582,
3.62425509130894));
#35241=CARTESIAN_POINT('Ctrl Pts',(-0.0792934088483033,0.139475624489065,
3.61631541123206));
#35242=CARTESIAN_POINT('Ctrl Pts',(0.0741994892135014,0.142250917737222,
3.60837573115519));
#35243=CARTESIAN_POINT('Ctrl Pts',(0.159757056720716,0.0147845549843712,
3.60043605107831));
#35244=CARTESIAN_POINT('Ctrl Pts',(0.099044626950589,-0.126218308388737,
3.59249637100143));
#35245=CARTESIAN_POINT('Ctrl Pts',(-0.0523506785380631,-0.151658366379244,
3.58455669092456));
#35246=CARTESIAN_POINT('Ctrl Pts',(-0.155815152588506,-0.0382438462810607,
3.57661701084768));
#35247=CARTESIAN_POINT('Ctrl Pts',(-0.116618308301774,0.110186600832138,
3.5686773307708));
#35248=CARTESIAN_POINT('Ctrl Pts',(0.0293506179707539,0.157731274399797,
3.56073765069393));
#35249=CARTESIAN_POINT('Ctrl Pts',(0.148448718300998,0.06086356485237,3.55279797061705));
#35250=CARTESIAN_POINT('Ctrl Pts',(0.131626773789177,-0.0917348800435817,
3.54485829054018));
#35251=CARTESIAN_POINT('Ctrl Pts',(-0.00570228534924597,-0.160332334867275,
3.5369186104633));
#35252=CARTESIAN_POINT('Ctrl Pts',(-0.137824845456608,-0.0821538836809814,
3.52897893038643));
#35253=CARTESIAN_POINT('Ctrl Pts',(-0.143730023800696,0.0712832907209694,
3.52103925030955));
#35254=CARTESIAN_POINT('Ctrl Pts',(-0.0180941331067087,0.159375913074104,
3.51309957023267));
#35255=CARTESIAN_POINT('Ctrl Pts',(0.124215853509266,0.101703545182399,
3.5051598901558));
#35256=CARTESIAN_POINT('Ctrl Pts',(0.152582649157857,-0.0494051387567767,
3.49722021007893));
#35257=CARTESIAN_POINT('Ctrl Pts',(0.0786662962002181,-0.119469354791712,
3.49192709002767));
#35258=CARTESIAN_POINT('Ctrl Pts',(0.0350561322973228,-0.131128202024318,
3.48928053000205));
#35259=CARTESIAN_POINT('Ctrl Pts',(0.109879644719085,0.0946377159884933,
4.01071946999795));
#35260=CARTESIAN_POINT('Ctrl Pts',(0.141353928983949,0.0580943237828825,
4.00807290997233));
#35261=CARTESIAN_POINT('Ctrl Pts',(0.164418985742774,-0.0482447252053583,
4.00277978992107));
#35262=CARTESIAN_POINT('Ctrl Pts',(0.0484157733702112,-0.164545193073921,
3.99484010984421));
#35263=CARTESIAN_POINT('Ctrl Pts',(-0.111912740260616,-0.129781565256457,
3.98690042976732));
#35264=CARTESIAN_POINT('Ctrl Pts',(-0.16977548400973,0.0236047185322397,
3.97896074969046));
#35265=CARTESIAN_POINT('Ctrl Pts',(-0.0721964162357802,0.155481990370402,
3.97102106961357));
#35266=CARTESIAN_POINT('Ctrl Pts',(0.0914844623135124,0.14495083574539,
3.9630813895367));
#35267=CARTESIAN_POINT('Ctrl Pts',(0.171404033075322,0.0017329517266617,
3.95514170945982));
#35268=CARTESIAN_POINT('Ctrl Pts',(0.0943900776986731,-0.143085391620212,
3.94720202938295));
#35269=CARTESIAN_POINT('Ctrl Pts',(-0.0690453431678277,-0.156890931096983,
3.93926234930607));
#35270=CARTESIAN_POINT('Ctrl Pts',(-0.169264388721129,-0.0270543231800365,
3.9313226692292));
#35271=CARTESIAN_POINT('Ctrl Pts',(-0.114508822838256,0.127554463266409,
3.92338298915232));
#35272=CARTESIAN_POINT('Ctrl Pts',(0.0450884255072127,0.165376332765398,
3.91544330907545));
#35273=CARTESIAN_POINT('Ctrl Pts',(0.163403732644156,0.0517838784166879,
3.90750362899857));
#35274=CARTESIAN_POINT('Ctrl Pts',(0.132110299036504,-0.109220967019342,
3.89956394892169));
#35275=CARTESIAN_POINT('Ctrl Pts',(-0.0201403219395664,-0.170225450443677,
3.89162426884482));
#35276=CARTESIAN_POINT('Ctrl Pts',(-0.153950921505229,-0.0753754468062197,
3.88368458876794));
#35277=CARTESIAN_POINT('Ctrl Pts',(-0.146807557584968,0.0884866358079437,
3.87574490869107));
#35278=CARTESIAN_POINT('Ctrl Pts',(-0.00525053138139654,0.171332349209229,
3.86780522861419));
#35279=CARTESIAN_POINT('Ctrl Pts',(0.141113761917547,0.0973100675950205,
3.85986554853731));
#35280=CARTESIAN_POINT('Ctrl Pts',(0.15827750297364,-0.0658071041261473,
3.85192586846044));
#35281=CARTESIAN_POINT('Ctrl Pts',(0.0305259606287044,-0.16867278508768,
3.84398618838356));
#35282=CARTESIAN_POINT('Ctrl Pts',(-0.125174457269873,-0.117105499873754,
3.83604650830669));
#35283=CARTESIAN_POINT('Ctrl Pts',(-0.166267987859908,0.0416809193090289,
3.82810682822981));
#35284=CARTESIAN_POINT('Ctrl Pts',(-0.0551303287615912,0.162305236052362,
3.82016714815293));
#35285=CARTESIAN_POINT('Ctrl Pts',(0.106483405996057,0.134326568732747,
3.81222746807606));
#35286=CARTESIAN_POINT('Ctrl Pts',(0.170603355057952,-0.0166384511693528,
3.80428778799918));
#35287=CARTESIAN_POINT('Ctrl Pts',(0.0785227507889612,-0.152369683403947,
3.79634810792231));
#35288=CARTESIAN_POINT('Ctrl Pts',(-0.0854514989366454,-0.148594697564603,
3.78840842784543));
#35289=CARTESIAN_POINT('Ctrl Pts',(-0.171188298922279,-0.00876978483161878,
3.78046874776855));
#35290=CARTESIAN_POINT('Ctrl Pts',(-0.100188984273494,0.139084543511992,
3.77252906769168));
#35291=CARTESIAN_POINT('Ctrl Pts',(0.0625410866422834,0.159596225819019,
3.7645893876148));
#35292=CARTESIAN_POINT('Ctrl Pts',(0.168009960460748,0.0339852320848313,
3.75664970753793));
#35293=CARTESIAN_POINT('Ctrl Pts',(0.119652734082865,-0.122741867512178,
3.74871002746105));
#35294=CARTESIAN_POINT('Ctrl Pts',(-0.0382558153916907,-0.167089303675579,
3.74077034738417));
#35295=CARTESIAN_POINT('Ctrl Pts',(-0.161138210014801,-0.0584535720629604,
3.7328306673073));
#35296=CARTESIAN_POINT('Ctrl Pts',(-0.136486122926345,0.103700921222673,
3.72489098723042));
#35297=CARTESIAN_POINT('Ctrl Pts',(0.0131295553900761,0.170909208617015,
3.71695130715355));
#35298=CARTESIAN_POINT('Ctrl Pts',(0.150724111277345,0.081636910106513,
3.70901162707667));
#35299=CARTESIAN_POINT('Ctrl Pts',(0.150319097509564,-0.0823802873159272,
3.7010719469998));
#35300=CARTESIAN_POINT('Ctrl Pts',(0.0122853354489075,-0.170971966570378,
3.69313226692292));
#35301=CARTESIAN_POINT('Ctrl Pts',(-0.136996600403042,-0.103025600106883,
3.68519258684605));
#35302=CARTESIAN_POINT('Ctrl Pts',(-0.16084756354836,0.0592486634615907,
3.67725290676916));
#35303=CARTESIAN_POINT('Ctrl Pts',(-0.037430154100943,0.1672761980004,3.66931322669229));
#35304=CARTESIAN_POINT('Ctrl Pts',(0.120257453145481,0.122149448072851,
3.66137354661541));
#35305=CARTESIAN_POINT('Ctrl Pts',(0.167840070942811,-0.0348145585488677,
3.65343386653854));
#35306=CARTESIAN_POINT('Ctrl Pts',(0.0617521342099411,-0.159903148744442,
3.64549418646166));
#35307=CARTESIAN_POINT('Ctrl Pts',(-0.100874650144087,-0.138588047549736,
3.63755450638479));
#35308=CARTESIAN_POINT('Ctrl Pts',(-0.171142903156845,0.00961511204917869,
3.62961482630791));
#35309=CARTESIAN_POINT('Ctrl Pts',(-0.0847165950870686,0.149014907745501,
3.62167514623104));
#35310=CARTESIAN_POINT('Ctrl Pts',(0.0792742823731183,0.15198001414926,
3.61373546615416));
#35311=CARTESIAN_POINT('Ctrl Pts',(0.170683466420304,0.0157957285018435,
3.60579578607728));
#35312=CARTESIAN_POINT('Ctrl Pts',(0.10581867621526,-0.134850871965913,
3.59785610600041));
#35313=CARTESIAN_POINT('Ctrl Pts',(-0.0559311461148929,-0.162030874983522,
3.58991642592353));
#35314=CARTESIAN_POINT('Ctrl Pts',(-0.166471960053118,-0.0408594924473857,
3.58197674584666));
#35315=CARTESIAN_POINT('Ctrl Pts',(-0.124594290340586,0.117722693251527,
3.57403706576978));
#35316=CARTESIAN_POINT('Ctrl Pts',(0.0313580214837342,0.168519132926404,
3.56609738569291));
#35317=CARTESIAN_POINT('Ctrl Pts',(0.158601706524679,0.065026262006443,
3.55815770561603));
#35318=CARTESIAN_POINT('Ctrl Pts',(0.14062924346017,-0.0980089871389004,
3.55021802553916));
#35319=CARTESIAN_POINT('Ctrl Pts',(-0.00609228693808808,-0.171298090088428,
3.54227834546228));
#35320=CARTESIAN_POINT('Ctrl Pts',(-0.147251225481083,-0.0877727089769424,
3.5343386653854));
#35321=CARTESIAN_POINT('Ctrl Pts',(-0.153560282059167,0.0761586336644345,
3.52639898530853));
#35322=CARTESIAN_POINT('Ctrl Pts',(-0.0193316616111828,0.17027625486957,
3.51845930523165));
#35323=CARTESIAN_POINT('Ctrl Pts',(0.132711461368385,0.10865944826032,3.51051962515478));
#35324=CARTESIAN_POINT('Ctrl Pts',(0.163018373074965,-0.0527841493520032,
3.5025799450779));
#35325=CARTESIAN_POINT('Ctrl Pts',(0.0840465917532045,-0.127640331046499,
3.49728682502665));
#35326=CARTESIAN_POINT('Ctrl Pts',(0.0374537582415282,-0.140096572423083,
3.49464026500102));
#35327=CARTESIAN_POINT('Ctrl Pts',(0.116913659442511,0.100696009035912,
4.01607920499693));
#35328=CARTESIAN_POINT('Ctrl Pts',(0.15040278985558,0.0618132685417683,
4.01343264497131));
#35329=CARTESIAN_POINT('Ctrl Pts',(0.17494437076274,-0.0513331417022419,
4.00813952492005));
#35330=CARTESIAN_POINT('Ctrl Pts',(0.0515151396231945,-0.17507865733575,
4.00019984484318));
#35331=CARTESIAN_POINT('Ctrl Pts',(-0.119076904876771,-0.138089613969001,
3.9922601647663));
#35332=CARTESIAN_POINT('Ctrl Pts',(-0.180643768642924,0.0251157894691961,
3.98432048468943));
#35333=CARTESIAN_POINT('Ctrl Pts',(-0.0768181153328184,0.165435267997838,
3.97638080461255));
#35334=CARTESIAN_POINT('Ctrl Pts',(0.0973408978391562,0.154229954870798,
3.96844112453568));
#35335=CARTESIAN_POINT('Ctrl Pts',(0.182376570303567,0.00184388772387479,
3.9605014444588));
#35336=CARTESIAN_POINT('Ctrl Pts',(0.100432518024861,-0.152245093163996,
3.95256176438192));
#35337=CARTESIAN_POINT('Ctrl Pts',(-0.0734653243360244,-0.166934402953208,
3.94462208430505));
#35338=CARTESIAN_POINT('Ctrl Pts',(-0.180099955267235,-0.0287862227331087,
3.93668240422817));
#35339=CARTESIAN_POINT('Ctrl Pts',(-0.121839177317157,0.135719942641123,
3.9287427241513));
#35340=CARTESIAN_POINT('Ctrl Pts',(0.0479747894892283,0.175963002958517,
3.92080304407442));
#35341=CARTESIAN_POINT('Ctrl Pts',(0.173864125597012,0.0550988560374321,
3.91286336399754));
#35342=CARTESIAN_POINT('Ctrl Pts',(0.140567423109983,-0.116212816074597,
3.90492368392067));
#35343=CARTESIAN_POINT('Ctrl Pts',(-0.0214296173447312,-0.181122539961793,
3.89698400384379));
#35344=CARTESIAN_POINT('Ctrl Pts',(-0.163806186794094,-0.0802006535492451,
3.88904432376692));
#35345=CARTESIAN_POINT('Ctrl Pts',(-0.156205535929391,0.0941511635800416,
3.88110464369004));
#35346=CARTESIAN_POINT('Ctrl Pts',(-0.005586647457645,0.182300297549597,
3.87316496361317));
#35347=CARTESIAN_POINT('Ctrl Pts',(0.150147248343024,0.103539432915148,
3.86522528353629));
#35348=CARTESIAN_POINT('Ctrl Pts',(0.168409737102627,-0.0700197873807462,
3.85728560345941));
#35349=CARTESIAN_POINT('Ctrl Pts',(0.0324800992415292,-0.179470479754251,
3.84934592338254));
#35350=CARTESIAN_POINT('Ctrl Pts',(-0.133187579060394,-0.124602082269994,
3.84140624330566));
#35351=CARTESIAN_POINT('Ctrl Pts',(-0.17691173791599,0.0443491496337192,
3.83346656322879));
#35352=CARTESIAN_POINT('Ctrl Pts',(-0.0586595315107243,0.172695308053416,
3.82552688315191));
#35353=CARTESIAN_POINT('Ctrl Pts',(0.113300008356683,0.142925568707939,
3.81758720307504));
#35354=CARTESIAN_POINT('Ctrl Pts',(0.181524636378177,-0.0177035721096275,
3.80964752299816));
#35355=CARTESIAN_POINT('Ctrl Pts',(0.0835494341804624,-0.162123724738966,
3.80170784292129));
#35356=CARTESIAN_POINT('Ctrl Pts',(-0.0909217305086156,-0.158107080801413,
3.7937681628444));
#35357=CARTESIAN_POINT('Ctrl Pts',(-0.18214702579272,-0.00933118813597588,
3.78582848276753));
#35358=CARTESIAN_POINT('Ctrl Pts',(-0.106602645259627,0.147988128242044,
3.77788880269065));
#35359=CARTESIAN_POINT('Ctrl Pts',(0.0665446937287967,0.169812878822259,
3.76994912261378));
#35360=CARTESIAN_POINT('Ctrl Pts',(0.178765223990991,0.0361608181406009,
3.7620094425369));
#35361=CARTESIAN_POINT('Ctrl Pts',(0.127312379282745,-0.130599265535886,
3.75406976246003));
#35362=CARTESIAN_POINT('Ctrl Pts',(-0.0407047855299705,-0.177785630781348,
3.74613008238315));
#35363=CARTESIAN_POINT('Ctrl Pts',(-0.171453574108382,-0.0621955143269609,
3.73819040230628));
#35364=CARTESIAN_POINT('Ctrl Pts',(-0.145223368124595,0.110339401066487,
3.7302507222294));
#35365=CARTESIAN_POINT('Ctrl Pts',(0.0139700521550768,0.18185006934563,
3.72231104215253));
#35366=CARTESIAN_POINT('Ctrl Pts',(0.160372810275332,0.0868629483698537,
3.71437136207565));
#35367=CARTESIAN_POINT('Ctrl Pts',(0.15994186929589,-0.087653913339944,
3.70643168199877));
#35368=CARTESIAN_POINT('Ctrl Pts',(0.013071788942189,-0.181916844788939,
3.6984920019219));
#35369=CARTESIAN_POINT('Ctrl Pts',(-0.145766524138762,-0.109620848843756,
3.69055232184502));
#35370=CARTESIAN_POINT('Ctrl Pts',(-0.171144321725171,0.06304150400269,
3.68261264176815));
#35371=CARTESIAN_POINT('Ctrl Pts',(-0.039826269011209,0.177984489264188,
3.67467296169127));
#35372=CARTESIAN_POINT('Ctrl Pts',(0.127955809817362,0.129968921992697,
3.66673328161439));
#35373=CARTESIAN_POINT('Ctrl Pts',(0.178584458888466,-0.0370432344610292,
3.65879360153752));
#35374=CARTESIAN_POINT('Ctrl Pts',(0.0657052360091523,-0.170139449612234,
3.65085392146064));
#35375=CARTESIAN_POINT('Ctrl Pts',(-0.107332204463161,-0.147459848777779,
3.64291424138377));
#35376=CARTESIAN_POINT('Ctrl Pts',(-0.182098723988745,0.0102306295082514,
3.63497456130689));
#35377=CARTESIAN_POINT('Ctrl Pts',(-0.0901397813258339,0.158554191001936,
3.62703488123002));
#35378=CARTESIAN_POINT('Ctrl Pts',(0.0843490755327352,0.161709110561297,
3.61909520115314));
#35379=CARTESIAN_POINT('Ctrl Pts',(0.181609876119891,0.0168069020193158,
3.61115552107626));
#35380=CARTESIAN_POINT('Ctrl Pts',(0.11259272547993,-0.14348343554309,3.60321584099938));
#35381=CARTESIAN_POINT('Ctrl Pts',(-0.0595116136917225,-0.1724033835878,
3.59527616092251));
#35382=CARTESIAN_POINT('Ctrl Pts',(-0.17712876751773,-0.0434751386137106,
3.58733648084563));
#35383=CARTESIAN_POINT('Ctrl Pts',(-0.132570272379398,0.125258785670915,
3.57939680076876));
#35384=CARTESIAN_POINT('Ctrl Pts',(0.0333654249967142,0.179306991453011,
3.57145712069188));
#35385=CARTESIAN_POINT('Ctrl Pts',(0.16875469474836,0.0691889591605158,
3.56351744061501));
#35386=CARTESIAN_POINT('Ctrl Pts',(0.149631713131164,-0.104283094234219,
3.55557776053813));
#35387=CARTESIAN_POINT('Ctrl Pts',(-0.00648228852693025,-0.182263845309582,
3.54763808046125));
#35388=CARTESIAN_POINT('Ctrl Pts',(-0.156677605505559,-0.0933915342729034,
3.53969840038438));
#35389=CARTESIAN_POINT('Ctrl Pts',(-0.163390540317638,0.0810339766078996,
3.5317587203075));
#35390=CARTESIAN_POINT('Ctrl Pts',(-0.0205691901156568,0.181176596665036,
3.52381904023063));
#35391=CARTESIAN_POINT('Ctrl Pts',(0.141207069227503,0.115615351338242,
3.51587936015375));
#35392=CARTESIAN_POINT('Ctrl Pts',(0.173454096992073,-0.0561631599472297,
3.50793968007688));
#35393=CARTESIAN_POINT('Ctrl Pts',(0.089426887306191,-0.135811307301286,
3.50264656002563));
#35394=CARTESIAN_POINT('Ctrl Pts',(0.0398513841857336,-0.149064942821849,
3.5));
#35395=CARTESIAN_POINT('Ctrl Pts',(0.095811615272233,0.0825211298936557,
4.));
#35396=CARTESIAN_POINT('Ctrl Pts',(0.102493030557671,0.0762815759767258,
4.));
#35397=CARTESIAN_POINT('Ctrl Pts',(0.10839405706188,0.0693097484661253,
4.));
#35398=CARTESIAN_POINT('Ctrl Pts',(0.11350885289652,0.0617853075148104,
4.));
#35399=CARTESIAN_POINT('Ctrl Pts',(0.117424080053794,0.0560255672420171,
4.));
#35400=CARTESIAN_POINT('Ctrl Pts',(0.120878299816185,0.0499406938168944,
4.));
#35401=CARTESIAN_POINT('Ctrl Pts',(0.123857056765335,0.0435961076613069,
4.));
#35402=CARTESIAN_POINT('Ctrl Pts',(0.125170781948423,0.0407979462969676,
4.));
#35403=CARTESIAN_POINT('Ctrl Pts',(0.126390002992329,0.0379525898756446,
4.));
#35404=CARTESIAN_POINT('Ctrl Pts',(0.12751038950843,0.0350750832122783,
4.));
#35405=CARTESIAN_POINT('Ctrl Pts',(0.131085166597008,0.0258939258664803,
4.));
#35406=CARTESIAN_POINT('Ctrl Pts',(0.133669431833427,0.0163619242015854,
4.));
#35407=CARTESIAN_POINT('Ctrl Pts',(0.135230958047781,0.0066616777752228,
4.));
#35408=CARTESIAN_POINT('Ctrl Pts',(0.135923073683569,0.00236223524203686,
4.));
#35409=CARTESIAN_POINT('Ctrl Pts',(0.136413711726375,-0.0019706858607116,
4.));
#35410=CARTESIAN_POINT('Ctrl Pts',(0.136697089502038,-0.00632254181082518,
4.));
#35411=CARTESIAN_POINT('Ctrl Pts',(0.136879678085431,-0.00912656979504798,
4.));
#35412=CARTESIAN_POINT('Ctrl Pts',(0.136975856810266,-0.011936494905405,
4.));
#35413=CARTESIAN_POINT('Ctrl Pts',(0.136984537674321,-0.0147391030393356,
4.));
#35414=CARTESIAN_POINT('Ctrl Pts',(0.137010531466213,-0.0231311723225325,
4.));
#35415=CARTESIAN_POINT('Ctrl Pts',(0.136255503035819,-0.0314800211532621,
4.));
#35416=CARTESIAN_POINT('Ctrl Pts',(0.134693290097439,-0.0396806821547801,
4.));
#35417=CARTESIAN_POINT('Ctrl Pts',(0.133704762250079,-0.0448698478361003,
4.));
#35418=CARTESIAN_POINT('Ctrl Pts',(0.132392592878428,-0.0499999054788172,
4.));
#35419=CARTESIAN_POINT('Ctrl Pts',(0.130776991260223,-0.0550529928649125,
4.));
#35420=CARTESIAN_POINT('Ctrl Pts',(0.129445892801333,-0.0592162449664668,
4.));
#35421=CARTESIAN_POINT('Ctrl Pts',(0.127906314848104,-0.0633316423760335,
4.));
#35422=CARTESIAN_POINT('Ctrl Pts',(0.126180878863323,-0.0673610722009708,
4.));
#35423=CARTESIAN_POINT('Ctrl Pts',(0.122312843187174,-0.0763941388895448,
4.));
#35424=CARTESIAN_POINT('Ctrl Pts',(0.117508253438465,-0.0850205194401279,
4.));
#35425=CARTESIAN_POINT('Ctrl Pts',(0.111900166266883,-0.0931314900308112,
4.));
#35426=CARTESIAN_POINT('Ctrl Pts',(0.108605841530307,-0.097896068439994,
4.));
#35427=CARTESIAN_POINT('Ctrl Pts',(0.105033346987346,-0.102482765945667,
4.));
#35428=CARTESIAN_POINT('Ctrl Pts',(0.101203104491781,-0.106867390005116,
4.));
#35429=CARTESIAN_POINT('Ctrl Pts',(0.0988795404734533,-0.109527261987172,
4.));
#35430=CARTESIAN_POINT('Ctrl Pts',(0.0964620699804362,-0.112111128650417,
4.));
#35431=CARTESIAN_POINT('Ctrl Pts',(0.0939639375491823,-0.114605366763082,
4.));
#35432=CARTESIAN_POINT('Ctrl Pts',(0.0874788757256353,-0.121080319075824,
4.));
#35433=CARTESIAN_POINT('Ctrl Pts',(0.0804377540716352,-0.126968968726175,
4.));
#35434=CARTESIAN_POINT('Ctrl Pts',(0.0729230547225638,-0.132178932127324,
4.));
#35435=CARTESIAN_POINT('Ctrl Pts',(0.0694491809116136,-0.134587379168854,
4.));
#35436=CARTESIAN_POINT('Ctrl Pts',(0.0658808132415588,-0.136845565695848,
4.));
#35437=CARTESIAN_POINT('Ctrl Pts',(0.0622290543017492,-0.138943290379685,
4.));
#35438=CARTESIAN_POINT('Ctrl Pts',(0.0562216582547972,-0.142394192583524,
4.));
#35439=CARTESIAN_POINT('Ctrl Pts',(0.0499865922958981,-0.145412833318798,
4.));
#35440=CARTESIAN_POINT('Ctrl Pts',(0.0435567401413007,-0.147956905966761,
4.));
#35441=CARTESIAN_POINT('Ctrl Pts',(0.0423577886630555,-0.148431290072134,
4.));
#35442=CARTESIAN_POINT('Ctrl Pts',(0.0411520494229064,-0.148889152887265,
4.));
#35443=CARTESIAN_POINT('Ctrl Pts',(0.0399398308045252,-0.149330586455588,
4.));
#35444=CARTESIAN_POINT('Ctrl Pts',(-0.126543984365092,-0.000100563349596846,
3.91934196736194));
#35445=CARTESIAN_POINT('Ctrl Pts',(-0.126601870201444,-0.00676638730964717,
3.91976237798504));
#35446=CARTESIAN_POINT('Ctrl Pts',(-0.126120638953643,-0.0134238307402375,
3.92018278860814));
#35447=CARTESIAN_POINT('Ctrl Pts',(-0.125071086204593,-0.0199904298605203,
3.92060319923124));
#35448=CARTESIAN_POINT('Ctrl Pts',(-0.118463964029756,-0.0613283451774388,
3.92324975925687));
#35449=CARTESIAN_POINT('Ctrl Pts',(-0.089334672430595,-0.0990661662809851,
3.92589631928249));
#35450=CARTESIAN_POINT('Ctrl Pts',(-0.0510182636513927,-0.115928743690777,
3.92854287930812));
#35451=CARTESIAN_POINT('Ctrl Pts',(-0.0127018548721904,-0.132791321100569,
3.93118943933374));
#35452=CARTESIAN_POINT('Ctrl Pts',(0.0348016710870533,-0.128778654816608,
3.93383599935937));
#35453=CARTESIAN_POINT('Ctrl Pts',(0.0697457276620979,-0.10572614363048,
3.93648255938499));
#35454=CARTESIAN_POINT('Ctrl Pts',(0.104689784237142,-0.0826736324443521,
3.93912911941062));
#35455=CARTESIAN_POINT('Ctrl Pts',(0.127074371427988,-0.0405812763560585,
3.94177567943624));
#35456=CARTESIAN_POINT('Ctrl Pts',(0.126652103797309,0.00127848798181101,
3.94442223946187));
#35457=CARTESIAN_POINT('Ctrl Pts',(0.126229836166631,0.0431382523196808,
3.94706879948749));
#35458=CARTESIAN_POINT('Ctrl Pts',(0.103000713714428,0.0847654249071265,
3.94971535951312));
#35459=CARTESIAN_POINT('Ctrl Pts',(0.067598717604338,0.107109484137676,
3.95236191953875));
#35460=CARTESIAN_POINT('Ctrl Pts',(0.0321967214942486,0.129453543368225,
3.95500847956437));
#35461=CARTESIAN_POINT('Ctrl Pts',(-0.0153781482737276,0.132514489241879,
3.95765503958999));
#35462=CARTESIAN_POINT('Ctrl Pts',(-0.0533465659413221,0.114879485769171,
3.96030159961562));
#35463=CARTESIAN_POINT('Ctrl Pts',(-0.0913149836089167,0.0972444822964635,
3.96294815964124));
#35464=CARTESIAN_POINT('Ctrl Pts',(-0.11967694917613,0.0589135294773952,
3.96559471966687));
#35465=CARTESIAN_POINT('Ctrl Pts',(-0.12544884800723,0.0174567123195785,
3.9682412796925));
#35466=CARTESIAN_POINT('Ctrl Pts',(-0.1262490134813,0.0117095024801126,
3.96860817558231));
#35467=CARTESIAN_POINT('Ctrl Pts',(-0.126615029050668,0.00590221784225734,
3.96897507147213));
#35468=CARTESIAN_POINT('Ctrl Pts',(-0.126567406925801,8.9117089303592E-5,
3.96934196736194));
#35469=CARTESIAN_POINT('Ctrl Pts',(-0.0398513841857263,-0.149064942821851,
4.));
#35470=CARTESIAN_POINT('Ctrl Pts',(-0.0894268873061843,-0.13581130730129,
3.99735343997437));
#35471=CARTESIAN_POINT('Ctrl Pts',(-0.173454116750112,-0.0561632816072737,
3.99206031992313));
#35472=CARTESIAN_POINT('Ctrl Pts',(-0.141207051852386,0.115615412698802,
3.98412063984625));
#35473=CARTESIAN_POINT('Ctrl Pts',(0.0205691872966891,0.181176549232701,
3.97618095976937));
#35474=CARTESIAN_POINT('Ctrl Pts',(0.16339053139201,0.0810339956098913,
3.9682412796925));
#35475=CARTESIAN_POINT('Ctrl Pts',(0.156677599794682,-0.0933915431448235,
3.96030159961562));
#35476=CARTESIAN_POINT('Ctrl Pts',(0.00648228676056323,-0.182263829019595,
3.95236191953875));
#35477=CARTESIAN_POINT('Ctrl Pts',(-0.149631704989928,-0.104283093629962,
3.94442223946187));
#35478=CARTESIAN_POINT('Ctrl Pts',(-0.168754687429674,0.0691889583215889,
3.93648255938499));
#35479=CARTESIAN_POINT('Ctrl Pts',(-0.0333654229848094,0.179306981584077,
3.92854287930812));
#35480=CARTESIAN_POINT('Ctrl Pts',(0.132570265831228,0.125258780485074,
3.92060319923124));
#35481=CARTESIAN_POINT('Ctrl Pts',(0.17712875926901,-0.0434751369680033,
3.91266351915436));
#35482=CARTESIAN_POINT('Ctrl Pts',(0.059511610779771,-0.172403375181386,
3.90472383907749));
#35483=CARTESIAN_POINT('Ctrl Pts',(-0.112592720088119,-0.143483428861666,
3.89678415900062));
#35484=CARTESIAN_POINT('Ctrl Pts',(-0.181609867534042,0.0168069012899025,
3.88884447892373));
#35485=CARTESIAN_POINT('Ctrl Pts',(-0.0843490715154628,0.161709102853824,
3.88090479884686));
#35486=CARTESIAN_POINT('Ctrl Pts',(0.0901397770410241,0.158554183500776,
3.87296511876998));
#35487=CARTESIAN_POINT('Ctrl Pts',(0.182098715355847,0.0102306290122647,
3.86502543869311));
#35488=CARTESIAN_POINT('Ctrl Pts',(0.107332199369115,-0.147459841777235,
3.85708575861623));
#35489=CARTESIAN_POINT('Ctrl Pts',(-0.0657052328909015,-0.17013944154474,
3.84914607853936));
#35490=CARTESIAN_POINT('Ctrl Pts',(-0.178584450418103,-0.0370432327022405,
3.84120639846248));
#35491=CARTESIAN_POINT('Ctrl Pts',(-0.127955803747328,0.129968915826709,
3.83326671838561));
#35492=CARTESIAN_POINT('Ctrl Pts',(0.039826267121788,0.177984480821945,
3.82532703830873));
#35493=CARTESIAN_POINT('Ctrl Pts',(0.171144313607041,0.063041501012073,
3.81738735823185));
#35494=CARTESIAN_POINT('Ctrl Pts',(0.145766517224248,-0.109620843643728,
3.80944767815498));
#35495=CARTESIAN_POINT('Ctrl Pts',(-0.0130717883220708,-0.181916836159762,
3.8015079980781));
#35496=CARTESIAN_POINT('Ctrl Pts',(-0.159941861709037,-0.0876539091820477,
3.79356831800123));
#35497=CARTESIAN_POINT('Ctrl Pts',(-0.160372802668024,0.0868629442494614,
3.78562863792435));
#35498=CARTESIAN_POINT('Ctrl Pts',(-0.013970051492431,0.181850060719556,
3.77768895784748));
#35499=CARTESIAN_POINT('Ctrl Pts',(0.145223361235896,0.110339395832533,
3.7697492777706));
#35500=CARTESIAN_POINT('Ctrl Pts',(0.171453565975463,-0.0621955113766863,
3.76180959769372));
#35501=CARTESIAN_POINT('Ctrl Pts',(0.0407047835991549,-0.177785622348059,
3.75386991761685));
#35502=CARTESIAN_POINT('Ctrl Pts',(-0.127312373243651,-0.130599259340906,
3.74593023753997));
#35503=CARTESIAN_POINT('Ctrl Pts',(-0.178765215511242,0.0361608164252855,
3.7379905574631));
#35504=CARTESIAN_POINT('Ctrl Pts',(-0.0665446905722607,0.169812870767156,
3.73005087738622));
#35505=CARTESIAN_POINT('Ctrl Pts',(0.106602640202898,0.147988121222216,
3.72211119730934));
#35506=CARTESIAN_POINT('Ctrl Pts',(0.182147017152552,-0.0093311876933208,
3.71417151723247));
#35507=CARTESIAN_POINT('Ctrl Pts',(0.0909217261957518,-0.158107073301583,
3.70623183715559));
#35508=CARTESIAN_POINT('Ctrl Pts',(-0.0835494302172658,-0.162123717048593,
3.69829215707872));
#35509=CARTESIAN_POINT('Ctrl Pts',(-0.181524627767524,-0.0177035712699219,
3.69035247700185));
#35510=CARTESIAN_POINT('Ctrl Pts',(-0.113300002982309,0.14292556192831,
3.68241279692496));
#35511=CARTESIAN_POINT('Ctrl Pts',(0.0586595287281965,0.172695299861449,
3.67447311684809));
#35512=CARTESIAN_POINT('Ctrl Pts',(0.176911729524118,0.0443491475303153,
3.66653343677121));
#35513=CARTESIAN_POINT('Ctrl Pts',(0.133187572742707,-0.124602076359984,
3.65859375669434));
#35514=CARTESIAN_POINT('Ctrl Pts',(-0.0324800977009374,-0.179470471240069,
3.65065407661746));
#35515=CARTESIAN_POINT('Ctrl Pts',(-0.168409729113823,-0.0700197840611982,
3.64271439654059));
#35516=CARTESIAN_POINT('Ctrl Pts',(-0.150147241221285,0.103539428007117,
3.63477471646371));
#35517=CARTESIAN_POINT('Ctrl Pts',(0.00558664719359638,0.182300288895857,
3.62683503638684));
#35518=CARTESIAN_POINT('Ctrl Pts',(0.156205528517827,0.094151159125646,
3.61889535630996));
#35519=CARTESIAN_POINT('Ctrl Pts',(0.163806179027695,-0.0802006497663837,
3.61095567623308));
#35520=CARTESIAN_POINT('Ctrl Pts',(0.0214296163208854,-0.181122531330724,
3.60301599615621));
#35521=CARTESIAN_POINT('Ctrl Pts',(-0.140567416427732,-0.116212810634341,
3.59507631607934));
#35522=CARTESIAN_POINT('Ctrl Pts',(-0.173864117377934,0.0550988535555318,
3.58713663600245));
#35523=CARTESIAN_POINT('Ctrl Pts',(-0.0479747871584019,0.175962994372803,
3.57919695592558));
#35524=CARTESIAN_POINT('Ctrl Pts',(0.121839171429706,0.13571993663382,3.5712572758487));
#35525=CARTESIAN_POINT('Ctrl Pts',(0.180099946935509,-0.0287862221383337,
3.56331759577183));
#35526=CARTESIAN_POINT('Ctrl Pts',(0.0734653204375665,-0.166934393666355,
3.55537791569495));
#35527=CARTESIAN_POINT('Ctrl Pts',(-0.100432512451176,-0.152245088347237,
3.54743823561807));
#35528=CARTESIAN_POINT('Ctrl Pts',(-0.182376563237206,0.00184389181179004,
3.5394985555412));
#35529=CARTESIAN_POINT('Ctrl Pts',(-0.0973408901199132,0.154229940417525,
3.53155887546432));
#35530=CARTESIAN_POINT('Ctrl Pts',(0.0768181056158631,0.16543527210962,
3.52361919538745));
#35531=CARTESIAN_POINT('Ctrl Pts',(0.180643771975638,0.0251157687415861,
3.51567951531057));
#35532=CARTESIAN_POINT('Ctrl Pts',(0.11907687582224,-0.13808957637103,3.50773983523369));
#35533=CARTESIAN_POINT('Ctrl Pts',(-0.0515150906951779,-0.17507869823889,
3.49980015515682));
#35534=CARTESIAN_POINT('Ctrl Pts',(-0.174944455635001,-0.0513330523253054,
3.49186047507995));
#35535=CARTESIAN_POINT('Ctrl Pts',(-0.15040278985559,0.061813268541742,
3.4865673550287));
#35536=CARTESIAN_POINT('Ctrl Pts',(-0.116913659442529,0.100696009035892,
3.48392079500307));
#35537=CARTESIAN_POINT('Ctrl Pts',(-0.0374537582415214,-0.140096572423085,
4.00535973499898));
#35538=CARTESIAN_POINT('Ctrl Pts',(-0.0840465917531983,-0.127640331046503,
4.00271317497335));
#35539=CARTESIAN_POINT('Ctrl Pts',(-0.163018391644278,-0.0527842636924701,
3.9974200549221));
#35540=CARTESIAN_POINT('Ctrl Pts',(-0.132711445038627,0.108659505929172,
3.98948037484522));
#35541=CARTESIAN_POINT('Ctrl Pts',(0.0193316589618159,0.170276210290963,
3.98154069476835));
#35542=CARTESIAN_POINT('Ctrl Pts',(0.153560273670542,0.0761586515231869,
3.97360101469147));
#35543=CARTESIAN_POINT('Ctrl Pts',(0.147251220113796,-0.0877727173150906,
3.9656613346146));
#35544=CARTESIAN_POINT('Ctrl Pts',(0.00609228527799324,-0.171298074778515,
3.95772165453772));
#35545=CARTESIAN_POINT('Ctrl Pts',(-0.140629235808745,-0.0980089865709976,
3.94978197446085));
#35546=CARTESIAN_POINT('Ctrl Pts',(-0.158601699646316,0.0650262612179893,
3.94184229438397));
#35547=CARTESIAN_POINT('Ctrl Pts',(-0.0313580195928739,0.168519123651227,
3.93390261430709));
#35548=CARTESIAN_POINT('Ctrl Pts',(0.124594284186381,0.117722688377688,
3.92596293423022));
#35549=CARTESIAN_POINT('Ctrl Pts',(0.166471952300676,-0.0408594909006909,
3.91802325415334));
#35550=CARTESIAN_POINT('Ctrl Pts',(0.0559311433781364,-0.162030867082874,
3.91008357407647));
#35551=CARTESIAN_POINT('Ctrl Pts',(-0.105818671147842,-0.134850865686472,
3.90214389399959));
#35552=CARTESIAN_POINT('Ctrl Pts',(-0.170683458351015,0.0157957278163147,
3.89420421392272));
#35553=CARTESIAN_POINT('Ctrl Pts',(-0.0792742785975418,0.151980006905501,
3.88626453384583));
#35554=CARTESIAN_POINT('Ctrl Pts',(0.0847165910600508,0.149014900695642,
3.87832485376897));
#35555=CARTESIAN_POINT('Ctrl Pts',(0.171142895043338,0.00961511158303258,
3.87038517369209));
#35556=CARTESIAN_POINT('Ctrl Pts',(0.100874645356521,-0.138588040970374,
3.86244549361521));
#35557=CARTESIAN_POINT('Ctrl Pts',(-0.0617521312792973,-0.159903141162322,
3.85450581353833));
#35558=CARTESIAN_POINT('Ctrl Pts',(-0.16784006298206,-0.0348145568958948,
3.84656613346146));
#35559=CARTESIAN_POINT('Ctrl Pts',(-0.120257447440646,0.122149442277835,
3.83862645338458));
#35560=CARTESIAN_POINT('Ctrl Pts',(0.0374301523251976,0.167276190066077,
3.83068677330771));
#35561=CARTESIAN_POINT('Ctrl Pts',(0.16084755591865,0.0592486606509017,
3.82274709323083));
#35562=CARTESIAN_POINT('Ctrl Pts',(0.136996593904535,-0.103025595219711,
3.81480741315396));
#35563=CARTESIAN_POINT('Ctrl Pts',(-0.0122853348660984,-0.170971958460368,
3.80686773307708));
#35564=CARTESIAN_POINT('Ctrl Pts',(-0.150319090379167,-0.0823802834081873,
3.7989280530002));
#35565=CARTESIAN_POINT('Ctrl Pts',(-0.150724104127725,0.0816369062340208,
3.79098837292333));
#35566=CARTESIAN_POINT('Ctrl Pts',(-0.0131295547672976,0.170909200509922,
3.78304869284645));
#35567=CARTESIAN_POINT('Ctrl Pts',(0.136486116452099,0.103700916303616,
3.77510901276958));
#35568=CARTESIAN_POINT('Ctrl Pts',(0.161138202371193,-0.0584535692901865,
3.7671693326927));
#35569=CARTESIAN_POINT('Ctrl Pts',(0.0382558135770412,-0.167089295749672,
3.75922965261583));
#35570=CARTESIAN_POINT('Ctrl Pts',(-0.119652728407108,-0.122741861689914,
3.75128997253895));
#35571=CARTESIAN_POINT('Ctrl Pts',(-0.168009952491177,0.0339852304727166,
3.74335029246208));
#35572=CARTESIAN_POINT('Ctrl Pts',(-0.0625410836756577,0.159596218248545,
3.73541061238519));
#35573=CARTESIAN_POINT('Ctrl Pts',(0.100188979521,0.139084536914507,3.72747093230832));
#35574=CARTESIAN_POINT('Ctrl Pts',(0.171188290801939,-0.00876978441559563,
3.71953125223144));
#35575=CARTESIAN_POINT('Ctrl Pts',(0.0854514948832616,-0.148594690515994,
3.71159157215457));
#35576=CARTESIAN_POINT('Ctrl Pts',(-0.078522747064207,-0.15236967617626,
3.7036518920777));
#35577=CARTESIAN_POINT('Ctrl Pts',(-0.170603346965352,-0.0166384503801673,
3.69571221200081));
#35578=CARTESIAN_POINT('Ctrl Pts',(-0.106483400945028,0.134326562361009,
3.68777253192394));
#35579=CARTESIAN_POINT('Ctrl Pts',(0.0551303261464719,0.162305228353258,
3.67983285184707));
#35580=CARTESIAN_POINT('Ctrl Pts',(0.166267979972926,0.0416809173321745,
3.67189317177019));
#35581=CARTESIAN_POINT('Ctrl Pts',(0.125174451332285,-0.117105494319316,
3.66395349169331));
#35582=CARTESIAN_POINT('Ctrl Pts',(-0.030525959180801,-0.168672777085747,
3.65601381161644));
#35583=CARTESIAN_POINT('Ctrl Pts',(-0.158277495465476,-0.0658071010063173,
3.64807413153956));
#35584=CARTESIAN_POINT('Ctrl Pts',(-0.141113755224281,0.0973100629822772,
3.64013445146269));
#35585=CARTESIAN_POINT('Ctrl Pts',(0.0052505311332342,0.171332341076135,
3.63219477138581));
#35586=CARTESIAN_POINT('Ctrl Pts',(0.146807550619315,0.0884866316215429,
3.62425509130893));
#35587=CARTESIAN_POINT('Ctrl Pts',(0.153950914206089,-0.0753754432509509,
3.61631541123206));
#35588=CARTESIAN_POINT('Ctrl Pts',(0.0201403209773194,-0.170225442331889,
3.60837573115518));
#35589=CARTESIAN_POINT('Ctrl Pts',(-0.132110292756286,-0.109220961906395,
3.60043605107832));
#35590=CARTESIAN_POINT('Ctrl Pts',(-0.163403724919573,0.0517838760841091,
3.59249637100142));
#35591=CARTESIAN_POINT('Ctrl Pts',(-0.0450884233166185,0.165376324696236,
3.58455669092456));
#35592=CARTESIAN_POINT('Ctrl Pts',(0.114508817305019,0.12755445762053,3.57661701084768));
#35593=CARTESIAN_POINT('Ctrl Pts',(0.169264380890674,-0.0270543226210457,
3.56867733077081));
#35594=CARTESIAN_POINT('Ctrl Pts',(0.0690453395039173,-0.156890922368865,
3.56073765069393));
#35595=CARTESIAN_POINT('Ctrl Pts',(-0.0943900724603247,-0.14308538709325,
3.55279797061705));
#35596=CARTESIAN_POINT('Ctrl Pts',(-0.171404026434103,0.00173295556863096,
3.54485829054018));
#35597=CARTESIAN_POINT('Ctrl Pts',(-0.0914844550586914,0.144950822161685,
3.5369186104633));
#35598=CARTESIAN_POINT('Ctrl Pts',(0.0721964071034376,0.155481994234803,
3.52897893038643));
#35599=CARTESIAN_POINT('Ctrl Pts',(0.169775487141934,0.0236046990516893,
3.52103925030955));
#35600=CARTESIAN_POINT('Ctrl Pts',(0.111912712954128,-0.129781529920537,
3.51309957023267));
#35601=CARTESIAN_POINT('Ctrl Pts',(-0.0484157273859087,-0.164545231516157,
3.5051598901558));
#35602=CARTESIAN_POINT('Ctrl Pts',(-0.164419065508765,-0.0482446412057121,
3.49722021007893));
#35603=CARTESIAN_POINT('Ctrl Pts',(-0.141353928983959,0.0580943237828579,
3.49192709002767));
#35604=CARTESIAN_POINT('Ctrl Pts',(-0.109879644719102,0.094637715988474,
3.48928053000205));
#35605=CARTESIAN_POINT('Ctrl Pts',(-0.0350561322973164,-0.13112820202432,
4.01071946999795));
#35606=CARTESIAN_POINT('Ctrl Pts',(-0.0786662962002123,-0.119469354791716,
4.00807290997233));
#35607=CARTESIAN_POINT('Ctrl Pts',(-0.152582666538444,-0.0494052457776665,
4.00277978992108));
#35608=CARTESIAN_POINT('Ctrl Pts',(-0.124215838224868,0.101703599159542,
3.9948401098442));
#35609=CARTESIAN_POINT('Ctrl Pts',(0.0180941306269427,0.159375871349225,
3.98690042976732));
#35610=CARTESIAN_POINT('Ctrl Pts',(0.143730015949074,0.0712833074364824,
3.97896074969045));
#35611=CARTESIAN_POINT('Ctrl Pts',(0.137824840432911,-0.0821538914853577,
3.97102106961357));
#35612=CARTESIAN_POINT('Ctrl Pts',(0.0057022837954231,-0.160332320537436,
3.9630813895367));
#35613=CARTESIAN_POINT('Ctrl Pts',(-0.131626766627563,-0.0917348795120337,
3.95514170945982));
#35614=CARTESIAN_POINT('Ctrl Pts',(-0.148448711862958,0.0608635641143897,
3.94720202938295));
#35615=CARTESIAN_POINT('Ctrl Pts',(-0.0293506162009384,0.157731265718376,
3.93926234930607));
#35616=CARTESIAN_POINT('Ctrl Pts',(0.116618302541534,0.110186596270301,
3.93132266922919));
#35617=CARTESIAN_POINT('Ctrl Pts',(0.155815145332341,-0.0382438448333786,
3.92338298915232));
#35618=CARTESIAN_POINT('Ctrl Pts',(0.0523506759765019,-0.151658358984361,
3.91544330907544));
#35619=CARTESIAN_POINT('Ctrl Pts',(-0.0990446222075651,-0.126218302511277,
3.90750362899857));
#35620=CARTESIAN_POINT('Ctrl Pts',(-0.159757049167988,0.0147845543427269,
3.89956394892169));
#35621=CARTESIAN_POINT('Ctrl Pts',(-0.0741994856796208,0.142250910957177,
3.89162426884482));
#35622=CARTESIAN_POINT('Ctrl Pts',(0.0792934050790776,0.139475617890508,
3.88368458876794));
#35623=CARTESIAN_POINT('Ctrl Pts',(0.160187074730829,0.0089995941538004,
3.87574490869107));
#35624=CARTESIAN_POINT('Ctrl Pts',(0.0944170913439271,-0.129716240163513,
3.86780522861419));
#35625=CARTESIAN_POINT('Ctrl Pts',(-0.0577990296676931,-0.149666840779905,
3.85986554853731));
#35626=CARTESIAN_POINT('Ctrl Pts',(-0.157095675546018,-0.0325858810895492,
3.85192586846044));
#35627=CARTESIAN_POINT('Ctrl Pts',(-0.112559091133964,0.114329968728961,
3.84398618838356));
#35628=CARTESIAN_POINT('Ctrl Pts',(0.0350340375286068,0.156567899310209,
3.83604650830669));
#35629=CARTESIAN_POINT('Ctrl Pts',(0.150550798230259,0.0554558202897304,
3.8281068282298));
#35630=CARTESIAN_POINT('Ctrl Pts',(0.128226670584821,-0.0964303467956928,
3.82016714815294));
#35631=CARTESIAN_POINT('Ctrl Pts',(-0.0114988814101258,-0.160027080760974,
3.81222746807605));
#35632=CARTESIAN_POINT('Ctrl Pts',(-0.140696319049298,-0.0771066576343268,
3.80428778799918));
#35633=CARTESIAN_POINT('Ctrl Pts',(-0.141075405587426,0.0764108682185801,
3.79634810792231));
#35634=CARTESIAN_POINT('Ctrl Pts',(-0.0122890580421644,0.159968340300288,
3.78840842784543));
#35635=CARTESIAN_POINT('Ctrl Pts',(0.127748871668302,0.0970624367746977,
3.78046874776856));
#35636=CARTESIAN_POINT('Ctrl Pts',(0.150822838766923,-0.0547116272036868,
3.77252906769167));
#35637=CARTESIAN_POINT('Ctrl Pts',(0.0358068435549273,-0.156392969151285,
3.7645893876148));
#35638=CARTESIAN_POINT('Ctrl Pts',(-0.111993083570565,-0.114884464038922,
3.75664970753792));
#35639=CARTESIAN_POINT('Ctrl Pts',(-0.157254689471112,0.0318096445201475,
3.74871002746105));
#35640=CARTESIAN_POINT('Ctrl Pts',(-0.0585374767790549,0.149379565729933,
3.74077034738417));
#35641=CARTESIAN_POINT('Ctrl Pts',(0.0937753188391016,0.130180952606797,
3.7328306673073));
#35642=CARTESIAN_POINT('Ctrl Pts',(0.160229564451327,-0.00820838113787044,
3.72489098723042));
#35643=CARTESIAN_POINT('Ctrl Pts',(0.0799812635707716,-0.139082307730405,
3.71695130715355));
#35644=CARTESIAN_POINT('Ctrl Pts',(-0.0734960639111485,-0.142615635303926,
3.70901162707667));
#35645=CARTESIAN_POINT('Ctrl Pts',(-0.15968206616318,-0.015573329490413,
3.7010719469998));
#35646=CARTESIAN_POINT('Ctrl Pts',(-0.0996667989077476,0.125727562793709,
3.69313226692292));
#35647=CARTESIAN_POINT('Ctrl Pts',(0.0516011235647474,0.151915156845068,
3.68519258684604));
#35648=CARTESIAN_POINT('Ctrl Pts',(0.155624230421734,0.039012687134034,
3.67725290676917));
#35649=CARTESIAN_POINT('Ctrl Pts',(0.117161329921862,-0.109608912278647,
3.66931322669229));
#35650=CARTESIAN_POINT('Ctrl Pts',(-0.0285718206606646,-0.157875082931424,
3.66137354661541));
#35651=CARTESIAN_POINT('Ctrl Pts',(-0.148145261817129,-0.0615944179514364,
3.65343386653854));
#35652=CARTESIAN_POINT('Ctrl Pts',(-0.132080269227278,0.0910806979574378,
3.64549418646166));
#35653=CARTESIAN_POINT('Ctrl Pts',(0.00491441507287188,0.160364393256412,
3.63755450638479));
#35654=CARTESIAN_POINT('Ctrl Pts',(0.137409572720802,0.08282210411744,3.62961482630791));
#35655=CARTESIAN_POINT('Ctrl Pts',(0.144095649384483,-0.0705502367355182,
3.62167514623104));
#35656=CARTESIAN_POINT('Ctrl Pts',(0.0188510256337537,-0.159328353333054,
3.61373546615416));
#35657=CARTESIAN_POINT('Ctrl Pts',(-0.12365316908484,-0.102229113178448,
3.60579578607729));
#35658=CARTESIAN_POINT('Ctrl Pts',(-0.152943332461211,0.0484688986126864,
3.5978561060004));
#35659=CARTESIAN_POINT('Ctrl Pts',(-0.0422020594748354,0.15478965501967,
3.58991642592354));
#35660=CARTESIAN_POINT('Ctrl Pts',(0.107178463180333,0.119388978607241,
3.58197674584666));
#35661=CARTESIAN_POINT('Ctrl Pts',(0.15842881484584,-0.0253224231037578,
3.57403706576978));
#35662=CARTESIAN_POINT('Ctrl Pts',(0.0646253585702682,-0.146847451071376,
3.56609738569291));
#35663=CARTESIAN_POINT('Ctrl Pts',(-0.0883476324694729,-0.133925685839263,
3.55815770561603));
#35664=CARTESIAN_POINT('Ctrl Pts',(-0.160431489631001,0.00162201932547174,
3.55021802553915));
#35665=CARTESIAN_POINT('Ctrl Pts',(-0.0856280199974695,0.135671703905846,
3.54227834546228));
#35666=CARTESIAN_POINT('Ctrl Pts',(0.067574708591012,0.145528716359985,
3.5343386653854));
#35667=CARTESIAN_POINT('Ctrl Pts',(0.15890720230823,0.0220936293617927,
3.52639898530853));
#35668=CARTESIAN_POINT('Ctrl Pts',(0.104748550086015,-0.121473483470044,
3.51845930523165));
#35669=CARTESIAN_POINT('Ctrl Pts',(-0.0453163640766394,-0.154011764793424,
3.51051962515478));
#35670=CARTESIAN_POINT('Ctrl Pts',(-0.153893675382528,-0.0451562300861186,
3.5025799450779));
#35671=CARTESIAN_POINT('Ctrl Pts',(-0.132305068112328,0.0543753790239735,
3.49728682502665));
#35672=CARTESIAN_POINT('Ctrl Pts',(-0.102845629995675,0.0885794229410565,
3.49464026500102));
#35673=CARTESIAN_POINT('Ctrl Pts',(-0.0326585063531114,-0.122159831625554,
4.01607920499693));
#35674=CARTESIAN_POINT('Ctrl Pts',(-0.0732860006472263,-0.111298378536929,
4.0134326449713));
#35675=CARTESIAN_POINT('Ctrl Pts',(-0.142146941432609,-0.046026227862863,
4.00813952492006));
#35676=CARTESIAN_POINT('Ctrl Pts',(-0.11572023141111,0.0947476923899126,
4.00019984484318));
#35677=CARTESIAN_POINT('Ctrl Pts',(0.0168566022920696,0.148475532407486,
3.9922601647663));
#35678=CARTESIAN_POINT('Ctrl Pts',(0.133899758227606,0.0664079633497781,
3.98432048468943));
#35679=CARTESIAN_POINT('Ctrl Pts',(0.128398460752025,-0.076535065655625,
3.97638080461255));
#35680=CARTESIAN_POINT('Ctrl Pts',(0.00531228231285306,-0.149366566296356,
3.96844112453568));
#35681=CARTESIAN_POINT('Ctrl Pts',(-0.12262429744638,-0.0854607724530698,
3.9605014444588));
#35682=CARTESIAN_POINT('Ctrl Pts',(-0.1382957240796,0.0567008670107902,
3.95256176438192));
#35683=CARTESIAN_POINT('Ctrl Pts',(-0.0273432128090029,0.146943407785525,
3.94462208430505));
#35684=CARTESIAN_POINT('Ctrl Pts',(0.108642320896687,0.102650504162914,
3.93668240422817));
#35685=CARTESIAN_POINT('Ctrl Pts',(0.145158338364007,-0.0356281987660663,
3.9287427241513));
#35686=CARTESIAN_POINT('Ctrl Pts',(0.0487702085748674,-0.141285850885848,
3.92080304407442));
#35687=CARTESIAN_POINT('Ctrl Pts',(-0.0922705732672884,-0.117585739336083,
3.91286336399754));
#35688=CARTESIAN_POINT('Ctrl Pts',(-0.148830639984962,0.0137733808691391,
3.90492368392067));
#35689=CARTESIAN_POINT('Ctrl Pts',(-0.0691246927616998,0.132521815008853,
3.89698400384379));
#35690=CARTESIAN_POINT('Ctrl Pts',(0.0738702190981043,0.129936335085374,
3.88904432376692));
#35691=CARTESIAN_POINT('Ctrl Pts',(0.149231254418321,0.00838407672456824,
3.88110464369004));
#35692=CARTESIAN_POINT('Ctrl Pts',(0.0879595373313327,-0.120844439356652,
3.87316496361317));
#35693=CARTESIAN_POINT('Ctrl Pts',(-0.0538459280560888,-0.139430540397488,
3.86522528353628));
#35694=CARTESIAN_POINT('Ctrl Pts',(-0.146351288109975,-0.0303572052832036,
3.85728560345941));
#35695=CARTESIAN_POINT('Ctrl Pts',(-0.104860734827282,0.106510495180087,
3.84934592338253));
#35696=CARTESIAN_POINT('Ctrl Pts',(0.0326379227320163,0.145859608554342,
3.84140624330567));
#35697=CARTESIAN_POINT('Ctrl Pts',(0.140254040541868,0.0516629799285589,
3.83346656322878));
#35698=CARTESIAN_POINT('Ctrl Pts',(0.119456747265108,-0.0898350983716749,
3.82552688315191));
#35699=CARTESIAN_POINT('Ctrl Pts',(-0.0107124279541533,-0.14908220306158,
3.81758720307504));
#35700=CARTESIAN_POINT('Ctrl Pts',(-0.131073547719428,-0.0718330318604663,
3.80964752299816));
#35701=CARTESIAN_POINT('Ctrl Pts',(-0.131426707047127,0.0711848302031395,
3.80170784292129));
#35702=CARTESIAN_POINT('Ctrl Pts',(-0.0114485613170311,0.149027480090653,
3.7937681628444));
#35703=CARTESIAN_POINT('Ctrl Pts',(0.119011626884504,0.0904239572457801,
3.78582848276753));
#35704=CARTESIAN_POINT('Ctrl Pts',(0.140507475162653,-0.0509696851171873,
3.77788880269065));
#35705=CARTESIAN_POINT('Ctrl Pts',(0.0333578735328136,-0.145696642552897,
3.76994912261378));
#35706=CARTESIAN_POINT('Ctrl Pts',(-0.104333438734023,-0.10702706638793,
3.7620094425369));
#35707=CARTESIAN_POINT('Ctrl Pts',(-0.146499426451047,0.0296340585675785,
3.75406976246003));
#35708=CARTESIAN_POINT('Ctrl Pts',(-0.0545338698824522,0.139162913211322,
3.74613008238315));
#35709=CARTESIAN_POINT('Ctrl Pts',(0.0873616581572035,0.121277368299088,
3.73819040230628));
#35710=CARTESIAN_POINT('Ctrl Pts',(0.149270838100714,-0.00764697786014525,
3.7302507222294));
#35711=CARTESIAN_POINT('Ctrl Pts',(0.0745110322582815,-0.129569924944816,
3.72231104215252));
#35712=CARTESIAN_POINT('Ctrl Pts',(-0.0684693807580898,-0.132861594431592,
3.71437136207565));
#35713=CARTESIAN_POINT('Ctrl Pts',(-0.148760785361007,-0.0145082086006585,
3.70643168199877));
#35714=CARTESIAN_POINT('Ctrl Pts',(-0.0928501968704667,0.117128563226408,
3.6984920019219));
#35715=CARTESIAN_POINT('Ctrl Pts',(0.0480719209830229,0.141525085336877,
3.69055232184502));
#35716=CARTESIAN_POINT('Ctrl Pts',(0.144980480870543,0.0363444569358934,
3.68261264176815));
#35717=CARTESIAN_POINT('Ctrl Pts',(0.10914820851144,-0.102112330237978,
3.67467296169127));
#35718=CARTESIAN_POINT('Ctrl Pts',(-0.0266176821405283,-0.147077388777102,
3.66673328161439));
#35719=CARTESIAN_POINT('Ctrl Pts',(-0.138013028168781,-0.0573817348965553,
3.65879360153751));
#35720=CARTESIAN_POINT('Ctrl Pts',(-0.123046783230275,0.0848513329325982,
3.65085392146064));
#35721=CARTESIAN_POINT('Ctrl Pts',(0.00457829901250977,0.149396445436689,
3.64291424138376));
#35722=CARTESIAN_POINT('Ctrl Pts',(0.128011594822289,0.0771575766133371,
3.63497456130689));
#35723=CARTESIAN_POINT('Ctrl Pts',(0.134240384562878,-0.0657250302200856,
3.62703488123001));
#35724=CARTESIAN_POINT('Ctrl Pts',(0.0175617302901878,-0.148431264334219,
3.61909520115314));
#35725=CARTESIAN_POINT('Ctrl Pts',(-0.115196045413394,-0.0952372644505018,
3.61115552107626));
#35726=CARTESIAN_POINT('Ctrl Pts',(-0.14248294000285,0.0451539211412638,
3.60321584099938));
#35727=CARTESIAN_POINT('Ctrl Pts',(-0.039315695633052,0.144202985343104,
3.59527616092251));
#35728=CARTESIAN_POINT('Ctrl Pts',(0.0998481090556468,0.111223499593951,
3.58733648084563));
#35729=CARTESIAN_POINT('Ctrl Pts',(0.147593248801005,-0.0235905235864699,
3.57939680076876));
#35730=CARTESIAN_POINT('Ctrl Pts',(0.0602053776366188,-0.136803979773886,
3.57145712069188));
#35731=CARTESIAN_POINT('Ctrl Pts',(-0.0823051924786211,-0.124765984585276,
3.56351744061501));
#35732=CARTESIAN_POINT('Ctrl Pts',(-0.149458952827898,0.00151108308231263,
3.55557776053813));
#35733=CARTESIAN_POINT('Ctrl Pts',(-0.0797715849362477,0.126392585650007,
3.54763808046126));
#35734=CARTESIAN_POINT('Ctrl Pts',(0.0629530100785864,0.135575438485168,
3.53969840038438));
#35735=CARTESIAN_POINT('Ctrl Pts',(0.148038917474527,0.020582559671896,
3.5317587203075));
#35736=CARTESIAN_POINT('Ctrl Pts',(0.097584387217902,-0.113165437019551,
3.52381904023062));
#35737=CARTESIAN_POINT('Ctrl Pts',(-0.0422170007673702,-0.143478298070691,
3.51587936015375));
#35738=CARTESIAN_POINT('Ctrl Pts',(-0.143368285256292,-0.0420678189665254,
3.50793968007687));
#35739=CARTESIAN_POINT('Ctrl Pts',(-0.123256207240696,0.0506564342650893,
3.50264656002563));
#35740=CARTESIAN_POINT('Ctrl Pts',(-0.0958116152722475,0.0825211298936389,
3.5));
#35741=CARTESIAN_POINT('Ctrl Pts',(-0.126283770505697,7.06948412972308E-5,
3.95565803263806));
#35742=CARTESIAN_POINT('Ctrl Pts',(-0.126367959766412,0.0165211867142232,
3.95462594321935));
#35743=CARTESIAN_POINT('Ctrl Pts',(-0.123384590961307,0.0329424219101817,
3.95359385380063));
#35744=CARTESIAN_POINT('Ctrl Pts',(-0.117191734428964,0.0480476838959361,
3.95256176438192));
#35745=CARTESIAN_POINT('Ctrl Pts',(-0.101311553656068,0.086781713935702,
3.9499152043563));
#35746=CARTESIAN_POINT('Ctrl Pts',(-0.0643273832325353,0.116862560860614,
3.94726864433067));
#35747=CARTESIAN_POINT('Ctrl Pts',(-0.0231710424031541,0.124520833719301,
3.94462208430505));
#35748=CARTESIAN_POINT('Ctrl Pts',(0.0179852984262271,0.132179106577988,
3.94197552427942));
#35749=CARTESIAN_POINT('Ctrl Pts',(0.0633138096614572,0.117414805370451,
3.9393289642538));
#35750=CARTESIAN_POINT('Ctrl Pts',(0.0920640681902922,0.0869862042785193,
3.93668240422817));
#35751=CARTESIAN_POINT('Ctrl Pts',(0.120814326719127,0.0565576031865874,
3.93403584420254));
#35752=CARTESIAN_POINT('Ctrl Pts',(0.132986332541567,0.0104647022102606,
3.93138928417692));
#35753=CARTESIAN_POINT('Ctrl Pts',(0.123007647154597,-0.0301913569645331,
3.9287427241513));
#35754=CARTESIAN_POINT('Ctrl Pts',(0.113028961767627,-0.0708474161393267,
3.92609616412567));
#35755=CARTESIAN_POINT('Ctrl Pts',(0.0808995851712473,-0.106066633512587,
3.92344960410005));
#35756=CARTESIAN_POINT('Ctrl Pts',(0.0413280998993647,-0.11972622360759,
3.92080304407442));
#35757=CARTESIAN_POINT('Ctrl Pts',(0.00175661462748208,-0.133385813702593,
3.91815648404879));
#35758=CARTESIAN_POINT('Ctrl Pts',(-0.0452569793199031,-0.125485776519338,
3.91550992402317));
#35759=CARTESIAN_POINT('Ctrl Pts',(-0.0781904540798746,-0.0996425712268402,
3.91286336399754));
#35760=CARTESIAN_POINT('Ctrl Pts',(-0.10807787979064,-0.0761896290779491,
3.91046158687771));
#35761=CARTESIAN_POINT('Ctrl Pts',(-0.126369304595299,-0.037959184630699,
3.90805980975789));
#35762=CARTESIAN_POINT('Ctrl Pts',(-0.126614009842867,6.71750503076223E-5,
3.90565803263806));
#35763=CARTESIAN_POINT('Ctrl Pts',(-0.0398513841857263,-0.149064942821851,
4.));
#35764=CARTESIAN_POINT('Ctrl Pts',(-0.0498814023543805,-0.14540001546545,
4.));
#35765=CARTESIAN_POINT('Ctrl Pts',(-0.0594354697797451,-0.140634945951871,
4.));
#35766=CARTESIAN_POINT('Ctrl Pts',(-0.0684028880593604,-0.13492060142061,
4.));
#35767=CARTESIAN_POINT('Ctrl Pts',(-0.0752795449518356,-0.130538561296954,
4.));
#35768=CARTESIAN_POINT('Ctrl Pts',(-0.0818109545260972,-0.125596962852027,
4.));
#35769=CARTESIAN_POINT('Ctrl Pts',(-0.0879325986341956,-0.120150358192012,
4.));
#35770=CARTESIAN_POINT('Ctrl Pts',(-0.0903223739843738,-0.118024105615282,
4.));
#35771=CARTESIAN_POINT('Ctrl Pts',(-0.0926479810229214,-0.115821878910758,
4.));
#35772=CARTESIAN_POINT('Ctrl Pts',(-0.0948977224364798,-0.11355536832373,
4.));
#35773=CARTESIAN_POINT('Ctrl Pts',(-0.1022475948872,-0.106150711227375,
4.));
#35774=CARTESIAN_POINT('Ctrl Pts',(-0.108817076574654,-0.0980392058992304,
4.));
#35775=CARTESIAN_POINT('Ctrl Pts',(-0.114476228961537,-0.0893439955398699,
4.));
#35776=CARTESIAN_POINT('Ctrl Pts',(-0.117310911144628,-0.0849885450768213,
4.));
#35777=CARTESIAN_POINT('Ctrl Pts',(-0.119916487835761,-0.0804862654238585,
4.));
#35778=CARTESIAN_POINT('Ctrl Pts',(-0.122271719969265,-0.0758513570938915,
4.));
#35779=CARTESIAN_POINT('Ctrl Pts',(-0.123706258421051,-0.073028300238791,
4.));
#35780=CARTESIAN_POINT('Ctrl Pts',(-0.12504717142243,-0.0701567413128179,
4.));
#35781=CARTESIAN_POINT('Ctrl Pts',(-0.126284991686486,-0.067251866211871,
4.));
#35782=CARTESIAN_POINT('Ctrl Pts',(-0.1295973650463,-0.0594784994498528,
4.));
#35783=CARTESIAN_POINT('Ctrl Pts',(-0.132185052379765,-0.051445045564302,
4.));
#35784=CARTESIAN_POINT('Ctrl Pts',(-0.133964990884521,-0.0432169428549209,
4.));
#35785=CARTESIAN_POINT('Ctrl Pts',(-0.135518726559135,-0.0360345055517295,
4.));
#35786=CARTESIAN_POINT('Ctrl Pts',(-0.13645631947854,-0.0287032207927444,
4.));
#35787=CARTESIAN_POINT('Ctrl Pts',(-0.136789702571871,-0.0212983790736885,
4.));
#35788=CARTESIAN_POINT('Ctrl Pts',(-0.13693233353465,-0.0181303728827948,
4.));
#35789=CARTESIAN_POINT('Ctrl Pts',(-0.136963744111631,-0.0149584576035291,
4.));
#35790=CARTESIAN_POINT('Ctrl Pts',(-0.136886254945713,-0.0117904221806244,
4.));
#35791=CARTESIAN_POINT('Ctrl Pts',(-0.136677592311597,-0.00325954423806801,
4.));
#35792=CARTESIAN_POINT('Ctrl Pts',(-0.135681410366555,0.00524856144622462,
4.));
#35793=CARTESIAN_POINT('Ctrl Pts',(-0.133925248777689,0.0136159175851835,
4.));
#35794=CARTESIAN_POINT('Ctrl Pts',(-0.132934632228228,0.018335780221422,
4.));
#35795=CARTESIAN_POINT('Ctrl Pts',(-0.131701699385377,0.0230107212566983,
4.));
#35796=CARTESIAN_POINT('Ctrl Pts',(-0.130227956640556,0.0276173752808998,
4.));
#35797=CARTESIAN_POINT('Ctrl Pts',(-0.129158656751422,0.030959813881302,
4.));
#35798=CARTESIAN_POINT('Ctrl Pts',(-0.12796229886657,0.0342658696738965,
4.));
#35799=CARTESIAN_POINT('Ctrl Pts',(-0.126644858507038,0.0375136883583919,
4.));
#35800=CARTESIAN_POINT('Ctrl Pts',(-0.124572648602295,0.042622201998594,
4.));
#35801=CARTESIAN_POINT('Ctrl Pts',(-0.122198572282107,0.0475953519381505,
4.));
#35802=CARTESIAN_POINT('Ctrl Pts',(-0.119526530046339,0.0523977893098404,
4.));
#35803=CARTESIAN_POINT('Ctrl Pts',(-0.116935312520942,0.0570549611597328,
4.));
#35804=CARTESIAN_POINT('Ctrl Pts',(-0.11406058633243,0.0615550019486321,
4.));
#35805=CARTESIAN_POINT('Ctrl Pts',(-0.11092106856286,0.0658392337664117,
4.));
#35806=CARTESIAN_POINT('Ctrl Pts',(-0.10710607669906,0.071045227402084,
4.));
#35807=CARTESIAN_POINT('Ctrl Pts',(-0.102897192277319,0.075940267594365,
4.));
#35808=CARTESIAN_POINT('Ctrl Pts',(-0.0982968852906839,0.0804596595786888,
4.));
#35809=CARTESIAN_POINT('Ctrl Pts',(-0.0975398380300018,0.0812033911017416,
4.));
#35810=CARTESIAN_POINT('Ctrl Pts',(-0.0967721750025885,0.0819369232370377,
4.));
#35811=CARTESIAN_POINT('Ctrl Pts',(-0.0959941513168557,0.0826601513985347,
4.));
#35812=CARTESIAN_POINT('Origin',(0.,0.,3.7));
#35813=CARTESIAN_POINT('Origin',(0.,0.,3.4));
#35814=CARTESIAN_POINT('Origin',(1.,0.,3.8));
#35815=CARTESIAN_POINT('',(0.8,2.44929359829471E-17,4.));
#35816=CARTESIAN_POINT('Origin',(1.,0.,4.));
#35817=CARTESIAN_POINT('',(0.8,2.44929359829471E-17,3.6));
#35818=CARTESIAN_POINT('',(0.8,2.44929359829471E-17,3.8));
#35819=CARTESIAN_POINT('Origin',(1.,0.,3.6));
#35820=CARTESIAN_POINT('Origin',(1.4,-0.6,3.6));
#35821=CARTESIAN_POINT('',(1.4,-0.6,3.6));
#35822=CARTESIAN_POINT('',(1.4,0.6,3.6));
#35823=CARTESIAN_POINT('',(1.4,-0.6,3.6));
#35824=CARTESIAN_POINT('',(1.4,0.6,4.));
#35825=CARTESIAN_POINT('',(1.4,0.6,3.6));
#35826=CARTESIAN_POINT('',(1.4,-0.6,4.));
#35827=CARTESIAN_POINT('',(1.4,-0.6,4.));
#35828=CARTESIAN_POINT('',(1.4,-0.6,3.6));
#35829=CARTESIAN_POINT('Origin',(0.7,0.,3.6));
#35830=CARTESIAN_POINT('',(0.4,0.6,3.6));
#35831=CARTESIAN_POINT('',(0.4,-0.6,3.6));
#35832=CARTESIAN_POINT('',(0.4,-0.3,3.6));
#35833=CARTESIAN_POINT('',(1.4,0.6,3.6));
#35834=CARTESIAN_POINT('',(0.,-0.6,3.6));
#35835=CARTESIAN_POINT('Origin',(0.4,0.6,2.6));
#35836=CARTESIAN_POINT('',(-0.4,0.6,4.));
#35837=CARTESIAN_POINT('',(0.4,0.6,4.));
#35838=CARTESIAN_POINT('',(0.4,0.6,2.6));
#35839=CARTESIAN_POINT('',(0.4,0.6,2.6));
#35840=CARTESIAN_POINT('',(-0.4,0.6,2.6));
#35841=CARTESIAN_POINT('',(0.4,0.6,2.6));
#35842=CARTESIAN_POINT('',(-0.4,0.6,2.6));
#35843=CARTESIAN_POINT('Origin',(0.4,-0.6,2.6));
#35844=CARTESIAN_POINT('',(0.4,-0.6,2.6));
#35845=CARTESIAN_POINT('',(0.4,-0.6,2.6));
#35846=CARTESIAN_POINT('',(0.4,-0.6,2.6));
#35847=CARTESIAN_POINT('Origin',(-0.4,-0.6,2.6));
#35848=CARTESIAN_POINT('',(-0.4,-0.6,4.));
#35849=CARTESIAN_POINT('',(-0.4,-0.6,4.));
#35850=CARTESIAN_POINT('',(-0.4,-0.6,2.6));
#35851=CARTESIAN_POINT('',(-0.4,-0.6,2.6));
#35852=CARTESIAN_POINT('',(-0.4,-0.6,2.6));
#35853=CARTESIAN_POINT('Origin',(-0.4,0.6,2.6));
#35854=CARTESIAN_POINT('',(-0.4,0.6,2.6));
#35855=CARTESIAN_POINT('',(-0.4,0.6,4.));
#35856=CARTESIAN_POINT('Origin',(0.,0.,4.));
#35857=CARTESIAN_POINT('Origin',(0.,0.,2.6));
#35858=CARTESIAN_POINT('',(0.,0.,0.));
#35859=CARTESIAN_POINT('Origin',(0.,0.,4.1));
#35860=CARTESIAN_POINT('',(-0.2,2.44929359829471E-17,4.2));
#35861=CARTESIAN_POINT('Origin',(0.,0.,4.2));
#35862=CARTESIAN_POINT('',(-0.2,2.44929359829471E-17,4.));
#35863=CARTESIAN_POINT('',(-0.2,2.44929359829471E-17,4.1));
#35864=CARTESIAN_POINT('Origin',(0.,0.,4.));
#35865=CARTESIAN_POINT('Origin',(0.4,0.4,4.));
#35866=CARTESIAN_POINT('',(0.4,0.4,4.));
#35867=CARTESIAN_POINT('',(-0.4,0.4,4.));
#35868=CARTESIAN_POINT('',(0.4,0.4,4.));
#35869=CARTESIAN_POINT('',(-0.4,0.4,4.2));
#35870=CARTESIAN_POINT('',(-0.4,0.4,4.));
#35871=CARTESIAN_POINT('',(0.4,0.4,4.2));
#35872=CARTESIAN_POINT('',(0.4,0.4,4.2));
#35873=CARTESIAN_POINT('',(0.4,0.4,4.));
#35874=CARTESIAN_POINT('Origin',(0.4,-0.4,4.));
#35875=CARTESIAN_POINT('',(0.4,-0.4,4.));
#35876=CARTESIAN_POINT('',(0.4,-0.4,4.));
#35877=CARTESIAN_POINT('',(0.4,-0.4,4.2));
#35878=CARTESIAN_POINT('',(0.4,-0.4,4.2));
#35879=CARTESIAN_POINT('',(0.4,-0.4,4.));
#35880=CARTESIAN_POINT('Origin',(-0.4,-0.4,4.));
#35881=CARTESIAN_POINT('',(-0.4,-0.4,4.));
#35882=CARTESIAN_POINT('',(-0.4,-0.4,4.));
#35883=CARTESIAN_POINT('',(-0.4,-0.4,4.2));
#35884=CARTESIAN_POINT('',(-0.4,-0.4,4.2));
#35885=CARTESIAN_POINT('',(-0.4,-0.4,4.));
#35886=CARTESIAN_POINT('Origin',(-0.4,0.4,4.));
#35887=CARTESIAN_POINT('',(-0.4,0.4,4.));
#35888=CARTESIAN_POINT('',(-0.4,0.4,4.2));
#35889=CARTESIAN_POINT('Origin',(0.,0.,4.2));
#35890=CARTESIAN_POINT('Origin',(0.,0.,4.));
#35891=CARTESIAN_POINT('',(0.,0.,0.));
#35892=CARTESIAN_POINT('Origin',(0.,0.,0.));
#35893=CARTESIAN_POINT('',(-1.22464679914735E-17,-1.49975978266186E-33,
0.2));
#35894=CARTESIAN_POINT('',(-1.22464679914735E-17,-1.49975978266186E-33,
-0.2));
#35895=CARTESIAN_POINT('Origin',(0.,0.,0.));
#35896=CARTESIAN_POINT('',(0.,0.,0.));
#35897=CARTESIAN_POINT('Origin',(0.,0.,0.3));
#35898=CARTESIAN_POINT('',(-0.35,-4.28626379701574E-17,0.3));
#35899=CARTESIAN_POINT('Origin',(0.,0.,0.3));
#35900=CARTESIAN_POINT('',(-0.2,-2.44929359829471E-17,0.3));
#35901=CARTESIAN_POINT('Origin',(0.,0.,0.3));
#35902=CARTESIAN_POINT('Origin',(0.,0.,0.3));
#35903=CARTESIAN_POINT('',(-0.35,-4.28626379701574E-17,0.5));
#35904=CARTESIAN_POINT('Origin',(0.,0.,0.5));
#35905=CARTESIAN_POINT('',(-0.35,-4.28626379701574E-17,0.3));
#35906=CARTESIAN_POINT('Origin',(0.,0.,0.5));
#35907=CARTESIAN_POINT('Origin',(0.,0.,0.));
#35908=CARTESIAN_POINT('',(-0.2,-2.44929359829471E-17,0.));
#35909=CARTESIAN_POINT('',(-0.2,-2.44929359829471E-17,0.));
#35910=CARTESIAN_POINT('Origin',(0.,0.,0.));
#35911=CARTESIAN_POINT('Origin',(0.,0.,0.));
#35912=CARTESIAN_POINT('',(0.,0.,0.));
#35913=CARTESIAN_POINT('Ctrl Pts',(0.35,-6.12323399573676E-18,0.));
#35914=CARTESIAN_POINT('Ctrl Pts',(0.35,0.00590530772593761,-0.0578714436187594));
#35915=CARTESIAN_POINT('Ctrl Pts',(0.320737036978914,0.0177159231778128,
-0.173548309605457));
#35916=CARTESIAN_POINT('Ctrl Pts',(0.199460245847326,0.0354318463556257,
-0.305323295892745));
#35917=CARTESIAN_POINT('Ctrl Pts',(0.0301195604177668,0.0531477695334385,
-0.363416175774699));
#35918=CARTESIAN_POINT('Ctrl Pts',(-0.146502340124411,0.0708636927112515,
-0.333985996548453));
#35919=CARTESIAN_POINT('Ctrl Pts',(-0.287770405730312,0.088579615889064,
-0.223981002451209));
#35920=CARTESIAN_POINT('Ctrl Pts',(-0.359728502950795,0.106295539066877,
-0.0600284421673934));
#35921=CARTESIAN_POINT('Ctrl Pts',(-0.344906058802126,0.12401146224469,
0.118406781736645));
#35922=CARTESIAN_POINT('Ctrl Pts',(-0.247005954023888,0.141727385422503,
0.268319590417229));
#35923=CARTESIAN_POINT('Ctrl Pts',(-0.0895198614025972,0.159443308600316,
0.353506441262074));
#35924=CARTESIAN_POINT('Ctrl Pts',(0.0895288995299922,0.177159231778128,
0.353541847300449));
#35925=CARTESIAN_POINT('Ctrl Pts',(0.246980934267327,0.194875154955941,
0.268292799062886));
#35926=CARTESIAN_POINT('Ctrl Pts',(0.344941099461226,0.212591078133754,
0.118418424896554));
#35927=CARTESIAN_POINT('Ctrl Pts',(0.359691482037638,0.230307001311567,
-0.0600218865157286));
#35928=CARTESIAN_POINT('Ctrl Pts',(0.287800848035351,0.248022924489379,
-0.22400439780941));
#35929=CARTESIAN_POINT('Ctrl Pts',(0.146484276133641,0.265738847667193,
-0.33395050615258));
#35930=CARTESIAN_POINT('Ctrl Pts',(-0.0301168255445678,0.283454770845005,
-0.363456018331913));
#35931=CARTESIAN_POINT('Ctrl Pts',(-0.199452865725669,0.301170694022818,
-0.305285338376046));
#35932=CARTESIAN_POINT('Ctrl Pts',(-0.320745536260988,0.318886617200631,
-0.173578803829894));
#35933=CARTESIAN_POINT('Ctrl Pts',(-0.364665029422868,0.336602540378444,
-2.32705416708787E-16));
#35934=CARTESIAN_POINT('Ctrl Pts',(-0.320745536260988,0.354318463556256,
0.173578803829895));
#35935=CARTESIAN_POINT('Ctrl Pts',(-0.199452865725669,0.37203438673407,
0.305285338376046));
#35936=CARTESIAN_POINT('Ctrl Pts',(-0.0301168255445679,0.389750309911882,
0.363456018331913));
#35937=CARTESIAN_POINT('Ctrl Pts',(0.146484276133641,0.407466233089696,
0.33395050615258));
#35938=CARTESIAN_POINT('Ctrl Pts',(0.287800848035351,0.425182156267507,
0.224004397809409));
#35939=CARTESIAN_POINT('Ctrl Pts',(0.359691482037638,0.442898079445321,
0.0600218865157286));
#35940=CARTESIAN_POINT('Ctrl Pts',(0.344941099461226,0.460614002623134,
-0.118418424896554));
#35941=CARTESIAN_POINT('Ctrl Pts',(0.246980934267327,0.478329925800947,
-0.268292799062886));
#35942=CARTESIAN_POINT('Ctrl Pts',(0.0895288995299929,0.49604584897876,
-0.353541847300449));
#35943=CARTESIAN_POINT('Ctrl Pts',(-0.0895198614025975,0.513761772156572,
-0.353506441262075));
#35944=CARTESIAN_POINT('Ctrl Pts',(-0.247005954023888,0.531477695334385,
-0.268319590417228));
#35945=CARTESIAN_POINT('Ctrl Pts',(-0.344906058802126,0.549193618512198,
-0.118406781736645));
#35946=CARTESIAN_POINT('Ctrl Pts',(-0.359728502950795,0.56690954169001,
0.0600284421673935));
#35947=CARTESIAN_POINT('Ctrl Pts',(-0.287770405730312,0.584625464867824,
0.223981002451209));
#35948=CARTESIAN_POINT('Ctrl Pts',(-0.146502340124411,0.602341388045636,
0.333985996548453));
#35949=CARTESIAN_POINT('Ctrl Pts',(0.0301195604177669,0.62005731122345,
0.3634161757747));
#35950=CARTESIAN_POINT('Ctrl Pts',(0.199460245847326,0.637773234401262,
0.305323295892745));
#35951=CARTESIAN_POINT('Ctrl Pts',(0.320737036978914,0.655489157579075,
0.173548309605457));
#35952=CARTESIAN_POINT('Ctrl Pts',(0.35,0.66729977303095,0.0578714436187596));
#35953=CARTESIAN_POINT('Ctrl Pts',(0.35,0.673205080756888,2.57175827820944E-16));
#35954=CARTESIAN_POINT('Ctrl Pts',(0.35,-0.0149599650170943,0.));
#35955=CARTESIAN_POINT('Ctrl Pts',(0.35,-0.00905465729115664,-0.0578939412128541));
#35956=CARTESIAN_POINT('Ctrl Pts',(0.320737127540777,0.00275595816071859,
-0.17353420038403));
#35957=CARTESIAN_POINT('Ctrl Pts',(0.199462254474698,0.0204718813385314,
-0.305334734920036));
#35958=CARTESIAN_POINT('Ctrl Pts',(0.0301198482341514,0.0381878045163443,
-0.363411053172193));
#35959=CARTESIAN_POINT('Ctrl Pts',(-0.146504814797102,0.0559037276941571,
-0.33399283744356));
#35960=CARTESIAN_POINT('Ctrl Pts',(-0.287768683388874,0.0736196508719699,
-0.223978927605389));
#35961=CARTESIAN_POINT('Ctrl Pts',(-0.359733999999531,0.0913355740497829,
-0.060029831390249));
#35962=CARTESIAN_POINT('Ctrl Pts',(-0.344904107829491,0.109051497227595,
0.118406345723654));
#35963=CARTESIAN_POINT('Ctrl Pts',(-0.247009698820708,0.126767420405409,
0.268323507761981));
#35964=CARTESIAN_POINT('Ctrl Pts',(-0.0895193547402367,0.144483343583221,
0.353504534892372));
#35965=CARTESIAN_POINT('Ctrl Pts',(0.0895302448190081,0.162199266761034,
0.353547145096981));
#35966=CARTESIAN_POINT('Ctrl Pts',(0.246979562985841,0.179915189938847,
0.268291322927849));
#35967=CARTESIAN_POINT('Ctrl Pts',(0.344946301010151,0.19763111311666,0.118420201706933));
#35968=CARTESIAN_POINT('Ctrl Pts',(0.35968948216843,0.215347036294473,-0.0600215483887705));
#35969=CARTESIAN_POINT('Ctrl Pts',(0.287805188713831,0.233062959472285,
-0.224007779090794));
#35970=CARTESIAN_POINT('Ctrl Pts',(0.14648346160033,0.250778882650098,-0.333948647665377));
#35971=CARTESIAN_POINT('Ctrl Pts',(-0.0301172799130791,0.268494805827911,
-0.363461501186809));
#35972=CARTESIAN_POINT('Ctrl Pts',(-0.199451756376582,0.286210729005724,
-0.305283640177881));
#35973=CARTESIAN_POINT('Ctrl Pts',(-0.320750374264358,0.303926652183536,
-0.173581422140521));
#35974=CARTESIAN_POINT('Ctrl Pts',(-0.364663001235008,0.32164257536135,
-2.44953070219776E-16));
#35975=CARTESIAN_POINT('Ctrl Pts',(-0.320750374264359,0.339358498539162,
0.173581422140521));
#35976=CARTESIAN_POINT('Ctrl Pts',(-0.199451756376583,0.357074421716976,
0.305283640177881));
#35977=CARTESIAN_POINT('Ctrl Pts',(-0.0301172799130792,0.374790344894787,
0.363461501186809));
#35978=CARTESIAN_POINT('Ctrl Pts',(0.14648346160033,0.392506268072602,0.333948647665377));
#35979=CARTESIAN_POINT('Ctrl Pts',(0.287805188713831,0.410222191250413,
0.224007779090794));
#35980=CARTESIAN_POINT('Ctrl Pts',(0.35968948216843,0.427938114428227,0.0600215483887707));
#35981=CARTESIAN_POINT('Ctrl Pts',(0.344946301010151,0.445654037606039,
-0.118420201706934));
#35982=CARTESIAN_POINT('Ctrl Pts',(0.246979562985841,0.463369960783852,
-0.268291322927849));
#35983=CARTESIAN_POINT('Ctrl Pts',(0.0895302448190086,0.481085883961665,
-0.353547145096981));
#35984=CARTESIAN_POINT('Ctrl Pts',(-0.0895193547402369,0.498801807139478,
-0.353504534892371));
#35985=CARTESIAN_POINT('Ctrl Pts',(-0.247009698820707,0.516517730317291,
-0.268323507761982));
#35986=CARTESIAN_POINT('Ctrl Pts',(-0.344904107829491,0.534233653495103,
-0.118406345723654));
#35987=CARTESIAN_POINT('Ctrl Pts',(-0.359733999999531,0.551949576672917,
0.0600298313902493));
#35988=CARTESIAN_POINT('Ctrl Pts',(-0.287768683388874,0.569665499850729,
0.223978927605389));
#35989=CARTESIAN_POINT('Ctrl Pts',(-0.146504814797102,0.587381423028543,
0.333992837443561));
#35990=CARTESIAN_POINT('Ctrl Pts',(0.0301198482341516,0.605097346206355,
0.363411053172192));
#35991=CARTESIAN_POINT('Ctrl Pts',(0.199462254474698,0.622813269384167,
0.305334734920036));
#35992=CARTESIAN_POINT('Ctrl Pts',(0.320737127540777,0.640529192561981,
0.17353420038403));
#35993=CARTESIAN_POINT('Ctrl Pts',(0.35,0.652339808013856,0.0578939412128544));
#35994=CARTESIAN_POINT('Ctrl Pts',(0.35,0.658245115739793,2.57175827820944E-16));
#35995=CARTESIAN_POINT('Ctrl Pts',(0.335708111401436,-0.0447458605757917,
0.));
#35996=CARTESIAN_POINT('Ctrl Pts',(0.335708111401436,-0.0388405528498541,
-0.0554977928230549));
#35997=CARTESIAN_POINT('Ctrl Pts',(0.307640028870999,-0.0270299373979789,
-0.166468247501657));
#35998=CARTESIAN_POINT('Ctrl Pts',(0.191314552514196,-0.00931401422016608,
-0.292850380259684));
#35999=CARTESIAN_POINT('Ctrl Pts',(0.0288895245544089,0.00840190895764677,
-0.348578849160588));
#36000=CARTESIAN_POINT('Ctrl Pts',(-0.140518910052752,0.0261178321354596,
-0.32034482131761));
#36001=CARTESIAN_POINT('Ctrl Pts',(-0.276020404510637,0.0438337553132723,
-0.214835940639136));
#36002=CARTESIAN_POINT('Ctrl Pts',(-0.345036788048542,0.0615496784910853,
-0.0575765924801678));
#36003=CARTESIAN_POINT('Ctrl Pts',(-0.330823089198529,0.0792656016688981,
0.113571967147225));
#36004=CARTESIAN_POINT('Ctrl Pts',(-0.236917968165966,0.0969815248467109,
0.257361203462888));
#36005=CARTESIAN_POINT('Ctrl Pts',(-0.0858646474450097,0.114697448024524,
0.339072263044565));
#36006=CARTESIAN_POINT('Ctrl Pts',(0.0858724496913478,0.132413371202337,
0.33910285135484));
#36007=CARTESIAN_POINT('Ctrl Pts',(0.236896364680631,0.150129294380149,
0.257338030560792));
#36008=CARTESIAN_POINT('Ctrl Pts',(0.330853351222059,0.167845217557962,
0.113582099143669));
#36009=CARTESIAN_POINT('Ctrl Pts',(0.34500478782966,0.185561140735775,-0.0575711130196162));
#36010=CARTESIAN_POINT('Ctrl Pts',(0.276046765897809,0.203277063913588,
-0.214855826894537));
#36011=CARTESIAN_POINT('Ctrl Pts',(0.140503123221668,0.220992987091401,
-0.320314851940556));
#36012=CARTESIAN_POINT('Ctrl Pts',(-0.0288868234010755,0.238708910269214,
-0.348612100831537));
#36013=CARTESIAN_POINT('Ctrl Pts',(-0.191308933142308,0.256424833447026,
-0.292820121666851));
#36014=CARTESIAN_POINT('Ctrl Pts',(-0.307645959021329,0.274140756624839,
-0.166489667090601));
#36015=CARTESIAN_POINT('Ctrl Pts',(-0.349775258797716,0.291856679802652,
-1.83714802664832E-16));
#36016=CARTESIAN_POINT('Ctrl Pts',(-0.307645959021329,0.309572602980465,
0.166489667090601));
#36017=CARTESIAN_POINT('Ctrl Pts',(-0.191308933142307,0.327288526158277,
0.292820121666851));
#36018=CARTESIAN_POINT('Ctrl Pts',(-0.0288868234010758,0.345004449336091,
0.348612100831537));
#36019=CARTESIAN_POINT('Ctrl Pts',(0.140503123221668,0.362720372513903,
0.320314851940556));
#36020=CARTESIAN_POINT('Ctrl Pts',(0.27604676589781,0.380436295691716,0.214855826894537));
#36021=CARTESIAN_POINT('Ctrl Pts',(0.34500478782966,0.398152218869529,0.0575711130196162));
#36022=CARTESIAN_POINT('Ctrl Pts',(0.330853351222058,0.415868142047341,
-0.113582099143669));
#36023=CARTESIAN_POINT('Ctrl Pts',(0.236896364680631,0.433584065225155,
-0.257338030560792));
#36024=CARTESIAN_POINT('Ctrl Pts',(0.0858724496913482,0.451299988402968,
-0.33910285135484));
#36025=CARTESIAN_POINT('Ctrl Pts',(-0.0858646474450095,0.46901591158078,
-0.339072263044565));
#36026=CARTESIAN_POINT('Ctrl Pts',(-0.236917968165967,0.486731834758593,
-0.257361203462888));
#36027=CARTESIAN_POINT('Ctrl Pts',(-0.330823089198529,0.504447757936406,
-0.113571967147225));
#36028=CARTESIAN_POINT('Ctrl Pts',(-0.345036788048542,0.522163681114218,
0.0575765924801677));
#36029=CARTESIAN_POINT('Ctrl Pts',(-0.276020404510636,0.539879604292032,
0.214835940639137));
#36030=CARTESIAN_POINT('Ctrl Pts',(-0.140518910052752,0.557595527469844,
0.320344821317609));
#36031=CARTESIAN_POINT('Ctrl Pts',(0.0288895245544092,0.575311450647657,
0.348578849160589));
#36032=CARTESIAN_POINT('Ctrl Pts',(0.191314552514196,0.59302737382547,0.292850380259683));
#36033=CARTESIAN_POINT('Ctrl Pts',(0.307640028870999,0.610743297003283,
0.166468247501657));
#36034=CARTESIAN_POINT('Ctrl Pts',(0.335708111401436,0.622553912455158,
0.0554977928230551));
#36035=CARTESIAN_POINT('Ctrl Pts',(0.335708111401436,0.628459220181096,
2.46674318445343E-16));
#36036=CARTESIAN_POINT('Ctrl Pts',(0.287271575555009,-0.0557889266101467,
0.));
#36037=CARTESIAN_POINT('Ctrl Pts',(0.287271575555009,-0.0498836188842091,
-0.0475015952121335));
#36038=CARTESIAN_POINT('Ctrl Pts',(0.263253248344736,-0.0380730034323339,
-0.142442953697593));
#36039=CARTESIAN_POINT('Ctrl Pts',(0.163712356953626,-0.020357080254521,
-0.250603083626219));
#36040=CARTESIAN_POINT('Ctrl Pts',(0.0247214371762577,-0.00264115707670821,
-0.298282769894969));
#36041=CARTESIAN_POINT('Ctrl Pts',(-0.120245826277052,0.0150747661011046,
-0.27412830773178));
#36042=CARTESIAN_POINT('Ctrl Pts',(-0.236194861111183,0.0327906892789176,
-0.183838021283139));
#36043=CARTESIAN_POINT('Ctrl Pts',(-0.295257011496817,0.0505066124567302,
-0.0492700305779588));
#36044=CARTESIAN_POINT('Ctrl Pts',(-0.283090408491503,0.0682225356345432,
0.0971853955774754));
#36045=CARTESIAN_POINT('Ctrl Pts',(-0.202736892426251,0.0859384588123559,
0.220230628323799));
#36046=CARTESIAN_POINT('Ctrl Pts',(-0.0734757000535192,0.103654381990169,
0.290149399582528));
#36047=CARTESIAN_POINT('Ctrl Pts',(0.0734832917947263,0.121370305167982,
0.290179134787802));
#36048=CARTESIAN_POINT('Ctrl Pts',(0.202715877612707,0.139086228345794,
0.220208133442515));
#36049=CARTESIAN_POINT('Ctrl Pts',(0.283119838964945,0.156802151523607,
0.0971951592678911));
#36050=CARTESIAN_POINT('Ctrl Pts',(0.295225923420481,0.17451807470142,-0.0492644880639345));
#36051=CARTESIAN_POINT('Ctrl Pts',(0.236220415317673,0.192233997879233,
-0.183857734680427));
#36052=CARTESIAN_POINT('Ctrl Pts',(0.120230691703391,0.209949921057046,
-0.274098363237872));
#36053=CARTESIAN_POINT('Ctrl Pts',(-0.0247192080583375,0.227665844234859,
-0.298316465071458));
#36054=CARTESIAN_POINT('Ctrl Pts',(-0.16370600748086,0.245381767412672,
-0.250570698506515));
#36055=CARTESIAN_POINT('Ctrl Pts',(-0.263260669021949,0.263097690590484,
-0.142469549414193));
#36056=CARTESIAN_POINT('Ctrl Pts',(-0.299308088749296,0.280813613768297,
4.89906140439551E-17));
#36057=CARTESIAN_POINT('Ctrl Pts',(-0.263260669021949,0.29852953694611,
0.142469549414192));
#36058=CARTESIAN_POINT('Ctrl Pts',(-0.163706007480861,0.316245460123924,
0.250570698506515));
#36059=CARTESIAN_POINT('Ctrl Pts',(-0.0247192080583377,0.333961383301735,
0.298316465071458));
#36060=CARTESIAN_POINT('Ctrl Pts',(0.120230691703391,0.351677306479549,
0.274098363237873));
#36061=CARTESIAN_POINT('Ctrl Pts',(0.236220415317673,0.369393229657361,
0.183857734680427));
#36062=CARTESIAN_POINT('Ctrl Pts',(0.295225923420481,0.387109152835174,
0.0492644880639345));
#36063=CARTESIAN_POINT('Ctrl Pts',(0.283119838964945,0.404825076012987,
-0.0971951592678911));
#36064=CARTESIAN_POINT('Ctrl Pts',(0.202715877612707,0.4225409991908,-0.220208133442515));
#36065=CARTESIAN_POINT('Ctrl Pts',(0.0734832917947267,0.440256922368613,
-0.290179134787802));
#36066=CARTESIAN_POINT('Ctrl Pts',(-0.0734757000535193,0.457972845546425,
-0.290149399582527));
#36067=CARTESIAN_POINT('Ctrl Pts',(-0.202736892426251,0.47568876872424,
-0.220230628323799));
#36068=CARTESIAN_POINT('Ctrl Pts',(-0.283090408491504,0.493404691902051,
-0.0971853955774754));
#36069=CARTESIAN_POINT('Ctrl Pts',(-0.295257011496816,0.511120615079865,
0.0492700305779587));
#36070=CARTESIAN_POINT('Ctrl Pts',(-0.236194861111183,0.528836538257677,
0.183838021283139));
#36071=CARTESIAN_POINT('Ctrl Pts',(-0.120245826277051,0.54655246143549,
0.27412830773178));
#36072=CARTESIAN_POINT('Ctrl Pts',(0.0247214371762577,0.564268384613303,
0.298282769894969));
#36073=CARTESIAN_POINT('Ctrl Pts',(0.163712356953627,0.581984307791115,
0.250603083626218));
#36074=CARTESIAN_POINT('Ctrl Pts',(0.263253248344736,0.599700230968929,
0.142442953697593));
#36075=CARTESIAN_POINT('Ctrl Pts',(0.287271575555009,0.611510846420803,
0.0475015952121336));
#36076=CARTESIAN_POINT('Ctrl Pts',(0.287271575555009,0.617416154146741,
2.11083729293675E-16));
#36077=CARTESIAN_POINT('Ctrl Pts',(0.2483964525207,-0.0248377821418625,
0.));
#36078=CARTESIAN_POINT('Ctrl Pts',(0.2483964525207,-0.0189324744159249,
-0.0410748300994032));
#36079=CARTESIAN_POINT('Ctrl Pts',(0.227628419209138,-0.00712185896404963,
-0.123165932150964));
#36080=CARTESIAN_POINT('Ctrl Pts',(0.141558052308102,0.0105940642137631,
-0.216690850682477));
#36081=CARTESIAN_POINT('Ctrl Pts',(0.0213760183023638,0.0283099873915761,
-0.257917233510476));
#36082=CARTESIAN_POINT('Ctrl Pts',(-0.103973673673943,0.0460259105693889,
-0.237032228868884));
#36083=CARTESIAN_POINT('Ctrl Pts',(-0.204231604209003,0.0637418337472016,
-0.158959949419166));
#36084=CARTESIAN_POINT('Ctrl Pts',(-0.255301599773748,0.0814577569250147,
-0.0426026337570547));
#36085=CARTESIAN_POINT('Ctrl Pts',(-0.244780981522273,0.0991736801028273,
0.0840337218647635));
#36086=CARTESIAN_POINT('Ctrl Pts',(-0.175301687703595,0.11688960328064,
0.190428088650001));
#36087=CARTESIAN_POINT('Ctrl Pts',(-0.063532544489394,0.134605526458453,
0.250884715042728));
#36088=CARTESIAN_POINT('Ctrl Pts',(0.0635392244753556,0.152321449636266,
0.250910876008833));
#36089=CARTESIAN_POINT('Ctrl Pts',(0.175283197378719,0.170037372814079,
0.190408301232517));
#36090=CARTESIAN_POINT('Ctrl Pts',(0.244806875770799,0.187753295991892,
0.0840423024059766));
#36091=CARTESIAN_POINT('Ctrl Pts',(0.255274250740611,0.205469219169704,
-0.0425977334636045));
#36092=CARTESIAN_POINT('Ctrl Pts',(0.204254078740494,0.223185142347517,
-0.158977335668398));
#36093=CARTESIAN_POINT('Ctrl Pts',(0.103960381877751,0.24090106552533,-0.23700579360409));
#36094=CARTESIAN_POINT('Ctrl Pts',(-0.0213741012368434,0.258616988703143,
-0.25794703087359));
#36095=CARTESIAN_POINT('Ctrl Pts',(-0.141552367454289,0.276332911880956,
-0.216662028058088));
#36096=CARTESIAN_POINT('Ctrl Pts',(-0.227635132018289,0.294048835058769,
-0.123189972933852));
#36097=CARTESIAN_POINT('Ctrl Pts',(-0.25880399389923,0.311764758236581,
-1.22476535109888E-17));
#36098=CARTESIAN_POINT('Ctrl Pts',(-0.227635132018289,0.329480681414395,
0.123189972933851));
#36099=CARTESIAN_POINT('Ctrl Pts',(-0.141552367454289,0.347196604592207,
0.216662028058088));
#36100=CARTESIAN_POINT('Ctrl Pts',(-0.0213741012368437,0.364912527770019,
0.257947030873589));
#36101=CARTESIAN_POINT('Ctrl Pts',(0.103960381877751,0.382628450947834,
0.23700579360409));
#36102=CARTESIAN_POINT('Ctrl Pts',(0.204254078740494,0.400344374125644,
0.158977335668397));
#36103=CARTESIAN_POINT('Ctrl Pts',(0.255274250740611,0.418060297303459,
0.0425977334636048));
#36104=CARTESIAN_POINT('Ctrl Pts',(0.244806875770799,0.435776220481271,
-0.0840423024059769));
#36105=CARTESIAN_POINT('Ctrl Pts',(0.175283197378719,0.453492143659084,
-0.190408301232516));
#36106=CARTESIAN_POINT('Ctrl Pts',(0.0635392244753558,0.471208066836898,
-0.250910876008834));
#36107=CARTESIAN_POINT('Ctrl Pts',(-0.063532544489394,0.488923990014709,
-0.250884715042728));
#36108=CARTESIAN_POINT('Ctrl Pts',(-0.175301687703595,0.506639913192522,
-0.190428088650001));
#36109=CARTESIAN_POINT('Ctrl Pts',(-0.244780981522273,0.524355836370335,
-0.0840337218647634));
#36110=CARTESIAN_POINT('Ctrl Pts',(-0.255301599773748,0.542071759548147,
0.0426026337570547));
#36111=CARTESIAN_POINT('Ctrl Pts',(-0.204231604209003,0.559787682725961,
0.158959949419166));
#36112=CARTESIAN_POINT('Ctrl Pts',(-0.103973673673943,0.577503605903774,
0.237032228868883));
#36113=CARTESIAN_POINT('Ctrl Pts',(0.0213760183023641,0.595219529081586,
0.257917233510476));
#36114=CARTESIAN_POINT('Ctrl Pts',(0.141558052308102,0.6129354522594,0.216690850682477));
#36115=CARTESIAN_POINT('Ctrl Pts',(0.227628419209138,0.630651375437212,
0.123165932150964));
#36116=CARTESIAN_POINT('Ctrl Pts',(0.2483964525207,0.642461990889088,0.0410748300994034));
#36117=CARTESIAN_POINT('Ctrl Pts',(0.2483964525207,0.648367298615025,1.8251875229942E-16));
#36118=CARTESIAN_POINT('Ctrl Pts',(0.248462856117505,0.024811377463635,
0.));
#36119=CARTESIAN_POINT('Ctrl Pts',(0.248462856117505,0.0307166851895726,
-0.0410773426135567));
#36120=CARTESIAN_POINT('Ctrl Pts',(0.227689236819528,0.0425273006414479,
-0.123204168627986));
#36121=CARTESIAN_POINT('Ctrl Pts',(0.141595138855583,0.0602432238192606,
-0.216744472856645));
#36122=CARTESIAN_POINT('Ctrl Pts',(0.0213816244011575,0.0779591469970735,
-0.257988110411106));
#36123=CARTESIAN_POINT('Ctrl Pts',(-0.104000537406664,0.0956750701748862,
-0.237093019599219));
#36124=CARTESIAN_POINT('Ctrl Pts',(-0.204286849538004,0.113390993352699,
-0.159003224998934));
#36125=CARTESIAN_POINT('Ctrl Pts',(-0.255367780255422,0.131106916530512,
-0.042613499783648));
#36126=CARTESIAN_POINT('Ctrl Pts',(-0.244847152934927,0.148822839708325,
0.08405635063601));
#36127=CARTESIAN_POINT('Ctrl Pts',(-0.175347141420753,0.166538762886138,
0.190477521147925));
#36128=CARTESIAN_POINT('Ctrl Pts',(-0.0635497192916874,0.184254686063951,
0.250952501372567));
#36129=CARTESIAN_POINT('Ctrl Pts',(0.0635557039981047,0.201970609241763,
0.250975957719874));
#36130=CARTESIAN_POINT('Ctrl Pts',(0.175330571819336,0.219686532419577,
0.19045975851969));
#36131=CARTESIAN_POINT('Ctrl Pts',(0.244870361932152,0.237402455597388,
0.0840641005753268));
#36132=CARTESIAN_POINT('Ctrl Pts',(0.255343245713768,0.255118378775203,
-0.0426092483460967));
#36133=CARTESIAN_POINT('Ctrl Pts',(0.20430704798701,0.272834301953014,-0.159018562236839));
#36134=CARTESIAN_POINT('Ctrl Pts',(0.103988480097989,0.290550225130828,
-0.2370698516718));
#36135=CARTESIAN_POINT('Ctrl Pts',(-0.0213796441337567,0.30826614830864,
-0.258013923898435));
#36136=CARTESIAN_POINT('Ctrl Pts',(-0.141590626072894,0.325982071486454,
-0.216720587313536));
#36137=CARTESIAN_POINT('Ctrl Pts',(-0.227694164509807,0.343697994664265,
-0.123221919677699));
#36138=CARTESIAN_POINT('Ctrl Pts',(-0.258873943134403,0.361413917842079,
-7.34859210659327E-17));
#36139=CARTESIAN_POINT('Ctrl Pts',(-0.227694164509807,0.379129841019892,
0.123221919677698));
#36140=CARTESIAN_POINT('Ctrl Pts',(-0.141590626072894,0.396845764197705,
0.216720587313536));
#36141=CARTESIAN_POINT('Ctrl Pts',(-0.0213796441337568,0.414561687375517,
0.258013923898435));
#36142=CARTESIAN_POINT('Ctrl Pts',(0.103988480097989,0.432277610553331,
0.2370698516718));
#36143=CARTESIAN_POINT('Ctrl Pts',(0.20430704798701,0.449993533731143,0.159018562236839));
#36144=CARTESIAN_POINT('Ctrl Pts',(0.255343245713769,0.467709456908956,
0.0426092483460965));
#36145=CARTESIAN_POINT('Ctrl Pts',(0.244870361932151,0.485425380086769,
-0.0840641005753267));
#36146=CARTESIAN_POINT('Ctrl Pts',(0.175330571819337,0.503141303264581,
-0.19045975851969));
#36147=CARTESIAN_POINT('Ctrl Pts',(0.063555703998105,0.520857226442395,
-0.250975957719874));
#36148=CARTESIAN_POINT('Ctrl Pts',(-0.0635497192916875,0.538573149620206,
-0.250952501372567));
#36149=CARTESIAN_POINT('Ctrl Pts',(-0.175347141420753,0.556289072798021,
-0.190477521147925));
#36150=CARTESIAN_POINT('Ctrl Pts',(-0.244847152934927,0.574004995975833,
-0.0840563506360099));
#36151=CARTESIAN_POINT('Ctrl Pts',(-0.255367780255422,0.591720919153647,
0.0426134997836479));
#36152=CARTESIAN_POINT('Ctrl Pts',(-0.204286849538004,0.609436842331458,
0.159003224998935));
#36153=CARTESIAN_POINT('Ctrl Pts',(-0.104000537406664,0.627152765509273,
0.23709301959922));
#36154=CARTESIAN_POINT('Ctrl Pts',(0.0213816244011575,0.644868688687084,
0.257988110411106));
#36155=CARTESIAN_POINT('Ctrl Pts',(0.141595138855583,0.662584611864898,
0.216744472856645));
#36156=CARTESIAN_POINT('Ctrl Pts',(0.227689236819528,0.680300535042709,
0.123204168627986));
#36157=CARTESIAN_POINT('Ctrl Pts',(0.248462856117505,0.692111150494585,
0.0410773426135568));
#36158=CARTESIAN_POINT('Ctrl Pts',(0.248462856117505,0.698016458220523,
1.82567544870787E-16));
#36159=CARTESIAN_POINT('Ctrl Pts',(0.28724245097485,0.055853598532737,0.));
#36160=CARTESIAN_POINT('Ctrl Pts',(0.28724245097485,0.0617589062586746,
-0.0475027005302338));
#36161=CARTESIAN_POINT('Ctrl Pts',(0.263226582660364,0.0735695217105498,
-0.142424798902927));
#36162=CARTESIAN_POINT('Ctrl Pts',(0.163696287887152,0.0912854448883627,
-0.250580687287576));
#36163=CARTESIAN_POINT('Ctrl Pts',(0.0247190065829995,0.109001368066176,
-0.298251180732612));
#36164=CARTESIAN_POINT('Ctrl Pts',(-0.120234286656455,0.126717291243988,
-0.274102316132114));
#36165=CARTESIAN_POINT('Ctrl Pts',(-0.236170461556994,0.144433214421801,
-0.183818837068975));
#36166=CARTESIAN_POINT('Ctrl Pts',(-0.295228524106512,0.162149137599614,
-0.0492654010455716));
#36167=CARTESIAN_POINT('Ctrl Pts',(-0.283061194331496,0.179865060777427,
0.0971754278326294));
#36168=CARTESIAN_POINT('Ctrl Pts',(-0.20271732386458,0.197580983955239,
0.220209331600313));
#36169=CARTESIAN_POINT('Ctrl Pts',(-0.0734681174847661,0.215296907133053,
0.290119481496877));
#36170=CARTESIAN_POINT('Ctrl Pts',(0.0734761958756083,0.233012830310865,
0.290151109768457));
#36171=CARTESIAN_POINT('Ctrl Pts',(0.202694964669258,0.250728753488678,
0.220185419477375));
#36172=CARTESIAN_POINT('Ctrl Pts',(0.283092504309657,0.268444676666491,
0.0971857729312045));
#36173=CARTESIAN_POINT('Ctrl Pts',(0.295195466051039,0.286160599844304,
-0.0492594044683245));
#36174=CARTESIAN_POINT('Ctrl Pts',(0.236197608912768,0.303876523022116,
-0.18383998447823));
#36175=CARTESIAN_POINT('Ctrl Pts',(0.120218287923552,0.32159244619993,-0.274070085063785));
#36176=CARTESIAN_POINT('Ctrl Pts',(-0.0247168215263096,0.339308369377742,
-0.298287663767521));
#36177=CARTESIAN_POINT('Ctrl Pts',(-0.163689118430773,0.357024292555555,
-0.25054484783482));
#36178=CARTESIAN_POINT('Ctrl Pts',(-0.263235252075215,0.374740215733368,
-0.142455794480522));
#36179=CARTESIAN_POINT('Ctrl Pts',(-0.299277210062645,0.392456138911181,
-1.22476535109888E-17));
#36180=CARTESIAN_POINT('Ctrl Pts',(-0.263235252075215,0.410172062088994,
0.142455794480522));
#36181=CARTESIAN_POINT('Ctrl Pts',(-0.163689118430773,0.427887985266806,
0.250544847834821));
#36182=CARTESIAN_POINT('Ctrl Pts',(-0.0247168215263098,0.445603908444619,
0.29828766376752));
#36183=CARTESIAN_POINT('Ctrl Pts',(0.120218287923551,0.463319831622433,
0.274070085063786));
#36184=CARTESIAN_POINT('Ctrl Pts',(0.236197608912768,0.481035754800244,
0.18383998447823));
#36185=CARTESIAN_POINT('Ctrl Pts',(0.29519546605104,0.498751677978058,0.0492594044683247));
#36186=CARTESIAN_POINT('Ctrl Pts',(0.283092504309657,0.51646760115587,-0.0971857729312049));
#36187=CARTESIAN_POINT('Ctrl Pts',(0.202694964669258,0.534183524333684,
-0.220185419477374));
#36188=CARTESIAN_POINT('Ctrl Pts',(0.0734761958756085,0.551899447511496,
-0.290151109768457));
#36189=CARTESIAN_POINT('Ctrl Pts',(-0.073468117484766,0.569615370689309,
-0.290119481496877));
#36190=CARTESIAN_POINT('Ctrl Pts',(-0.20271732386458,0.587331293867122,
-0.220209331600313));
#36191=CARTESIAN_POINT('Ctrl Pts',(-0.283061194331496,0.605047217044934,
-0.0971754278326294));
#36192=CARTESIAN_POINT('Ctrl Pts',(-0.295228524106513,0.622763140222748,
0.0492654010455718));
#36193=CARTESIAN_POINT('Ctrl Pts',(-0.236170461556994,0.64047906340056,
0.183818837068975));
#36194=CARTESIAN_POINT('Ctrl Pts',(-0.120234286656455,0.658194986578373,
0.274102316132114));
#36195=CARTESIAN_POINT('Ctrl Pts',(0.0247190065829998,0.675910909756186,
0.298251180732612));
#36196=CARTESIAN_POINT('Ctrl Pts',(0.163696287887152,0.693626832933998,
0.250580687287576));
#36197=CARTESIAN_POINT('Ctrl Pts',(0.263226582660364,0.711342756111813,
0.142424798902927));
#36198=CARTESIAN_POINT('Ctrl Pts',(0.28724245097485,0.723153371563687,0.047502700530234));
#36199=CARTESIAN_POINT('Ctrl Pts',(0.28724245097485,0.729058679289624,2.11062328899355E-16));
#36200=CARTESIAN_POINT('Ctrl Pts',(0.335700057265398,0.0447030440973884,
0.));
#36201=CARTESIAN_POINT('Ctrl Pts',(0.335700057265398,0.050608351823326,
-0.0554935013777734));
#36202=CARTESIAN_POINT('Ctrl Pts',(0.307632636214863,0.0624189672752012,
-0.166466110007902));
#36203=CARTESIAN_POINT('Ctrl Pts',(0.191309698322281,0.0801348904530141,
-0.292841849330558));
#36204=CARTESIAN_POINT('Ctrl Pts',(0.0288887935843006,0.0978508136308268,
-0.348571160208687));
#36205=CARTESIAN_POINT('Ctrl Pts',(-0.140515213206916,0.11556673680864,
-0.320336235724583));
#36206=CARTESIAN_POINT('Ctrl Pts',(-0.276014008976892,0.133282659986453,
-0.214831059389936));
#36207=CARTESIAN_POINT('Ctrl Pts',(-0.345027786866192,0.150998583164266,
-0.0575750283544988));
#36208=CARTESIAN_POINT('Ctrl Pts',(-0.330815408947634,0.168714506342078,
0.113569299752606));
#36209=CARTESIAN_POINT('Ctrl Pts',(-0.236911791455489,0.186430429519891,
0.257354513587));
#36210=CARTESIAN_POINT('Ctrl Pts',(-0.0858626540853489,0.204146352697704,
0.339064379015408));
#36211=CARTESIAN_POINT('Ctrl Pts',(0.0858702124863541,0.221862275875517,
0.33909401875172));
#36212=CARTESIAN_POINT('Ctrl Pts',(0.23689086160232,0.23957819905333,0.257332050851972));
#36213=CARTESIAN_POINT('Ctrl Pts',(0.330844729199832,0.257294122231142,
0.113579140368498));
#36214=CARTESIAN_POINT('Ctrl Pts',(0.344996773771998,0.275010045408956,
-0.0575697762899338));
#36215=CARTESIAN_POINT('Ctrl Pts',(0.276039572030225,0.292725968586768,
-0.214850227314705));
#36216=CARTESIAN_POINT('Ctrl Pts',(0.140499859509914,0.310441891764581,
-0.32030741162972));
#36217=CARTESIAN_POINT('Ctrl Pts',(-0.0288860705827872,0.328157814942394,
-0.348603015739585));
#36218=CARTESIAN_POINT('Ctrl Pts',(-0.191304489312158,0.345873738120207,
-0.292813319906457));
#36219=CARTESIAN_POINT('Ctrl Pts',(-0.30763794160998,0.363589661298019,
-0.166485328269541));
#36220=CARTESIAN_POINT('Ctrl Pts',(-0.349767134015211,0.381305584475832,
-1.22476535109888E-16));
#36221=CARTESIAN_POINT('Ctrl Pts',(-0.30763794160998,0.399021507653645,
0.166485328269541));
#36222=CARTESIAN_POINT('Ctrl Pts',(-0.191304489312158,0.416737430831458,
0.292813319906457));
#36223=CARTESIAN_POINT('Ctrl Pts',(-0.0288860705827875,0.43445335400927,
0.348603015739585));
#36224=CARTESIAN_POINT('Ctrl Pts',(0.140499859509914,0.452169277187084,
0.320307411629721));
#36225=CARTESIAN_POINT('Ctrl Pts',(0.276039572030225,0.469885200364896,
0.214850227314704));
#36226=CARTESIAN_POINT('Ctrl Pts',(0.344996773771998,0.487601123542709,
0.0575697762899342));
#36227=CARTESIAN_POINT('Ctrl Pts',(0.330844729199832,0.505317046720522,
-0.113579140368499));
#36228=CARTESIAN_POINT('Ctrl Pts',(0.23689086160232,0.523032969898335,-0.257332050851972));
#36229=CARTESIAN_POINT('Ctrl Pts',(0.0858702124863545,0.540748893076148,
-0.339094018751721));
#36230=CARTESIAN_POINT('Ctrl Pts',(-0.0858626540853487,0.55846481625396,
-0.339064379015408));
#36231=CARTESIAN_POINT('Ctrl Pts',(-0.23691179145549,0.576180739431775,
-0.257354513587));
#36232=CARTESIAN_POINT('Ctrl Pts',(-0.330815408947634,0.593896662609586,
-0.113569299752606));
#36233=CARTESIAN_POINT('Ctrl Pts',(-0.345027786866192,0.611612585787399,
0.0575750283544989));
#36234=CARTESIAN_POINT('Ctrl Pts',(-0.276014008976891,0.629328508965212,
0.214831059389936));
#36235=CARTESIAN_POINT('Ctrl Pts',(-0.140515213206917,0.647044432143026,
0.320336235724583));
#36236=CARTESIAN_POINT('Ctrl Pts',(0.028888793584301,0.664760355320838,
0.348571160208686));
#36237=CARTESIAN_POINT('Ctrl Pts',(0.191309698322281,0.682476278498651,
0.292841849330559));
#36238=CARTESIAN_POINT('Ctrl Pts',(0.307632636214863,0.700192201676463,
0.166466110007902));
#36239=CARTESIAN_POINT('Ctrl Pts',(0.335700057265398,0.712002817128339,
0.0554935013777736));
#36240=CARTESIAN_POINT('Ctrl Pts',(0.335700057265398,0.717908124854276,
2.46668400362192E-16));
#36241=CARTESIAN_POINT('Ctrl Pts',(0.35,0.0149599650170943,0.));
#36242=CARTESIAN_POINT('Ctrl Pts',(0.35,0.0208652727430319,-0.0578968747192045));
#36243=CARTESIAN_POINT('Ctrl Pts',(0.32073713934932,0.0326758881949071,
-0.173532360654391));
#36244=CARTESIAN_POINT('Ctrl Pts',(0.199462516383644,0.0503918113727199,
-0.305336226477714));
#36245=CARTESIAN_POINT('Ctrl Pts',(0.0301198857631062,0.0681077345505328,
-0.363410385225793));
#36246=CARTESIAN_POINT('Ctrl Pts',(-0.14650513747463,0.0858236577283456,
-0.333993729441574));
#36247=CARTESIAN_POINT('Ctrl Pts',(-0.287768458809325,0.103539580906158,
-0.223978657062087));
#36248=CARTESIAN_POINT('Ctrl Pts',(-0.359734716770725,0.121255504083971,
-0.0600300125337997));
#36249=CARTESIAN_POINT('Ctrl Pts',(-0.344903853438262,0.138971427261784,
0.118406288871047));
#36250=CARTESIAN_POINT('Ctrl Pts',(-0.247010187112264,0.156687350439597,
0.268324018552409));
#36251=CARTESIAN_POINT('Ctrl Pts',(-0.089519288675517,0.174403273617409,
0.353504286317008));
#36252=CARTESIAN_POINT('Ctrl Pts',(0.0895304202339372,0.192119196795223,
0.353547835887281));
#36253=CARTESIAN_POINT('Ctrl Pts',(0.246979384181701,0.209835119973035,
0.268291130451645));
#36254=CARTESIAN_POINT('Ctrl Pts',(0.344946979250533,0.227551043150848,
0.118420433388797));
#36255=CARTESIAN_POINT('Ctrl Pts',(0.359689221401479,0.245266966328661,
-0.0600215042997194));
#36256=CARTESIAN_POINT('Ctrl Pts',(0.287805754703591,0.262982889506474,
-0.224008219982846));
#36257=CARTESIAN_POINT('Ctrl Pts',(0.1464833553917,0.280698812684287,-0.333948405333508));
#36258=CARTESIAN_POINT('Ctrl Pts',(-0.0301173391590991,0.298414735862099,
-0.36346221610724));
#36259=CARTESIAN_POINT('Ctrl Pts',(-0.199451611726333,0.316130659039913,
-0.305283418746421));
#36260=CARTESIAN_POINT('Ctrl Pts',(-0.320751005101307,0.333846582217725,
-0.173581763547288));
#36261=CARTESIAN_POINT('Ctrl Pts',(-0.36466273677553,0.351562505395538,
-1.59219495642854E-16));
#36262=CARTESIAN_POINT('Ctrl Pts',(-0.320751005101307,0.369278428573351,
0.173581763547288));
#36263=CARTESIAN_POINT('Ctrl Pts',(-0.199451611726333,0.386994351751164,
0.305283418746421));
#36264=CARTESIAN_POINT('Ctrl Pts',(-0.0301173391590995,0.404710274928977,
0.36346221610724));
#36265=CARTESIAN_POINT('Ctrl Pts',(0.1464833553917,0.422426198106789,0.333948405333509));
#36266=CARTESIAN_POINT('Ctrl Pts',(0.28780575470359,0.440142121284602,0.224008219982845));
#36267=CARTESIAN_POINT('Ctrl Pts',(0.359689221401479,0.457858044462415,
0.0600215042997194));
#36268=CARTESIAN_POINT('Ctrl Pts',(0.344946979250532,0.475573967640229,
-0.118420433388797));
#36269=CARTESIAN_POINT('Ctrl Pts',(0.246979384181702,0.49328989081804,-0.268291130451645));
#36270=CARTESIAN_POINT('Ctrl Pts',(0.0895304202339372,0.511005813995854,
-0.353547835887281));
#36271=CARTESIAN_POINT('Ctrl Pts',(-0.0895192886755167,0.528721737173666,
-0.353504286317008));
#36272=CARTESIAN_POINT('Ctrl Pts',(-0.247010187112265,0.54643766035148,
-0.268324018552409));
#36273=CARTESIAN_POINT('Ctrl Pts',(-0.344903853438262,0.564153583529292,
-0.118406288871046));
#36274=CARTESIAN_POINT('Ctrl Pts',(-0.359734716770725,0.581869506707105,
0.0600300125337994));
#36275=CARTESIAN_POINT('Ctrl Pts',(-0.287768458809324,0.599585429884918,
0.223978657062087));
#36276=CARTESIAN_POINT('Ctrl Pts',(-0.14650513747463,0.617301353062731,
0.333993729441574));
#36277=CARTESIAN_POINT('Ctrl Pts',(0.0301198857631064,0.635017276240543,
0.363410385225793));
#36278=CARTESIAN_POINT('Ctrl Pts',(0.199462516383644,0.652733199418356,
0.305336226477713));
#36279=CARTESIAN_POINT('Ctrl Pts',(0.320737139349319,0.670449122596169,
0.173532360654391));
#36280=CARTESIAN_POINT('Ctrl Pts',(0.35,0.682259738048044,0.0578968747192047));
#36281=CARTESIAN_POINT('Ctrl Pts',(0.35,0.688165045773982,2.57175827820944E-16));
#36282=CARTESIAN_POINT('Ctrl Pts',(0.35,6.12323399573676E-18,0.));
#36283=CARTESIAN_POINT('Ctrl Pts',(0.35,0.00590530772593762,-0.0578714436187594));
#36284=CARTESIAN_POINT('Ctrl Pts',(0.320737036978914,0.0177159231778128,
-0.173548309605457));
#36285=CARTESIAN_POINT('Ctrl Pts',(0.199460245847326,0.0354318463556257,
-0.305323295892745));
#36286=CARTESIAN_POINT('Ctrl Pts',(0.0301195604177668,0.0531477695334385,
-0.363416175774699));
#36287=CARTESIAN_POINT('Ctrl Pts',(-0.146502340124411,0.0708636927112515,
-0.333985996548453));
#36288=CARTESIAN_POINT('Ctrl Pts',(-0.287770405730312,0.088579615889064,
-0.223981002451209));
#36289=CARTESIAN_POINT('Ctrl Pts',(-0.359728502950795,0.106295539066877,
-0.0600284421673934));
#36290=CARTESIAN_POINT('Ctrl Pts',(-0.344906058802126,0.12401146224469,
0.118406781736645));
#36291=CARTESIAN_POINT('Ctrl Pts',(-0.247005954023888,0.141727385422503,
0.268319590417229));
#36292=CARTESIAN_POINT('Ctrl Pts',(-0.0895198614025972,0.159443308600316,
0.353506441262074));
#36293=CARTESIAN_POINT('Ctrl Pts',(0.0895288995299922,0.177159231778128,
0.353541847300449));
#36294=CARTESIAN_POINT('Ctrl Pts',(0.246980934267327,0.194875154955941,
0.268292799062886));
#36295=CARTESIAN_POINT('Ctrl Pts',(0.344941099461226,0.212591078133754,
0.118418424896554));
#36296=CARTESIAN_POINT('Ctrl Pts',(0.359691482037638,0.230307001311567,
-0.0600218865157286));
#36297=CARTESIAN_POINT('Ctrl Pts',(0.287800848035351,0.248022924489379,
-0.22400439780941));
#36298=CARTESIAN_POINT('Ctrl Pts',(0.146484276133641,0.265738847667193,
-0.33395050615258));
#36299=CARTESIAN_POINT('Ctrl Pts',(-0.0301168255445678,0.283454770845005,
-0.363456018331913));
#36300=CARTESIAN_POINT('Ctrl Pts',(-0.199452865725669,0.301170694022818,
-0.305285338376046));
#36301=CARTESIAN_POINT('Ctrl Pts',(-0.320745536260988,0.318886617200631,
-0.173578803829894));
#36302=CARTESIAN_POINT('Ctrl Pts',(-0.364665029422868,0.336602540378444,
-2.32705416708787E-16));
#36303=CARTESIAN_POINT('Ctrl Pts',(-0.320745536260988,0.354318463556256,
0.173578803829895));
#36304=CARTESIAN_POINT('Ctrl Pts',(-0.199452865725669,0.37203438673407,
0.305285338376046));
#36305=CARTESIAN_POINT('Ctrl Pts',(-0.0301168255445679,0.389750309911882,
0.363456018331913));
#36306=CARTESIAN_POINT('Ctrl Pts',(0.146484276133641,0.407466233089696,
0.33395050615258));
#36307=CARTESIAN_POINT('Ctrl Pts',(0.287800848035351,0.425182156267507,
0.224004397809409));
#36308=CARTESIAN_POINT('Ctrl Pts',(0.359691482037638,0.442898079445321,
0.0600218865157286));
#36309=CARTESIAN_POINT('Ctrl Pts',(0.344941099461226,0.460614002623134,
-0.118418424896554));
#36310=CARTESIAN_POINT('Ctrl Pts',(0.246980934267327,0.478329925800947,
-0.268292799062886));
#36311=CARTESIAN_POINT('Ctrl Pts',(0.0895288995299929,0.49604584897876,
-0.353541847300449));
#36312=CARTESIAN_POINT('Ctrl Pts',(-0.0895198614025975,0.513761772156572,
-0.353506441262075));
#36313=CARTESIAN_POINT('Ctrl Pts',(-0.247005954023888,0.531477695334385,
-0.268319590417228));
#36314=CARTESIAN_POINT('Ctrl Pts',(-0.344906058802126,0.549193618512198,
-0.118406781736645));
#36315=CARTESIAN_POINT('Ctrl Pts',(-0.359728502950795,0.56690954169001,
0.0600284421673935));
#36316=CARTESIAN_POINT('Ctrl Pts',(-0.287770405730312,0.584625464867824,
0.223981002451209));
#36317=CARTESIAN_POINT('Ctrl Pts',(-0.146502340124411,0.602341388045636,
0.333985996548453));
#36318=CARTESIAN_POINT('Ctrl Pts',(0.0301195604177669,0.62005731122345,
0.3634161757747));
#36319=CARTESIAN_POINT('Ctrl Pts',(0.199460245847326,0.637773234401262,
0.305323295892745));
#36320=CARTESIAN_POINT('Ctrl Pts',(0.320737036978914,0.655489157579075,
0.173548309605457));
#36321=CARTESIAN_POINT('Ctrl Pts',(0.35,0.66729977303095,0.0578714436187596));
#36322=CARTESIAN_POINT('Ctrl Pts',(0.35,0.673205080756888,2.57175827820944E-16));
#36323=CARTESIAN_POINT('',(0.35,-6.12323399573676E-18,0.));
#36324=CARTESIAN_POINT('Origin',(0.3,0.,0.));
#36325=CARTESIAN_POINT('',(0.35,0.673205080756888,2.57175827820944E-16));
#36326=CARTESIAN_POINT('Ctrl Pts',(0.35,6.12323399573676E-18,0.));
#36327=CARTESIAN_POINT('Ctrl Pts',(0.35,0.00590530772593762,-0.0578714436187594));
#36328=CARTESIAN_POINT('Ctrl Pts',(0.320737036978914,0.0177159231778128,
-0.173548309605457));
#36329=CARTESIAN_POINT('Ctrl Pts',(0.199460245847326,0.0354318463556257,
-0.305323295892745));
#36330=CARTESIAN_POINT('Ctrl Pts',(0.0301195604177668,0.0531477695334385,
-0.363416175774699));
#36331=CARTESIAN_POINT('Ctrl Pts',(-0.146502340124411,0.0708636927112515,
-0.333985996548453));
#36332=CARTESIAN_POINT('Ctrl Pts',(-0.287770405730312,0.088579615889064,
-0.223981002451209));
#36333=CARTESIAN_POINT('Ctrl Pts',(-0.359728502950795,0.106295539066877,
-0.0600284421673934));
#36334=CARTESIAN_POINT('Ctrl Pts',(-0.344906058802126,0.12401146224469,
0.118406781736645));
#36335=CARTESIAN_POINT('Ctrl Pts',(-0.247005954023888,0.141727385422503,
0.268319590417229));
#36336=CARTESIAN_POINT('Ctrl Pts',(-0.0895198614025972,0.159443308600316,
0.353506441262074));
#36337=CARTESIAN_POINT('Ctrl Pts',(0.0895288995299922,0.177159231778128,
0.353541847300449));
#36338=CARTESIAN_POINT('Ctrl Pts',(0.246980934267327,0.194875154955941,
0.268292799062886));
#36339=CARTESIAN_POINT('Ctrl Pts',(0.344941099461226,0.212591078133754,
0.118418424896554));
#36340=CARTESIAN_POINT('Ctrl Pts',(0.359691482037638,0.230307001311567,
-0.0600218865157286));
#36341=CARTESIAN_POINT('Ctrl Pts',(0.287800848035351,0.248022924489379,
-0.22400439780941));
#36342=CARTESIAN_POINT('Ctrl Pts',(0.146484276133641,0.265738847667193,
-0.33395050615258));
#36343=CARTESIAN_POINT('Ctrl Pts',(-0.0301168255445678,0.283454770845005,
-0.363456018331913));
#36344=CARTESIAN_POINT('Ctrl Pts',(-0.199452865725669,0.301170694022818,
-0.305285338376046));
#36345=CARTESIAN_POINT('Ctrl Pts',(-0.320745536260988,0.318886617200631,
-0.173578803829894));
#36346=CARTESIAN_POINT('Ctrl Pts',(-0.364665029422868,0.336602540378444,
-2.32705416708787E-16));
#36347=CARTESIAN_POINT('Ctrl Pts',(-0.320745536260988,0.354318463556256,
0.173578803829895));
#36348=CARTESIAN_POINT('Ctrl Pts',(-0.199452865725669,0.37203438673407,
0.305285338376046));
#36349=CARTESIAN_POINT('Ctrl Pts',(-0.0301168255445679,0.389750309911882,
0.363456018331913));
#36350=CARTESIAN_POINT('Ctrl Pts',(0.146484276133641,0.407466233089696,
0.33395050615258));
#36351=CARTESIAN_POINT('Ctrl Pts',(0.287800848035351,0.425182156267507,
0.224004397809409));
#36352=CARTESIAN_POINT('Ctrl Pts',(0.359691482037638,0.442898079445321,
0.0600218865157286));
#36353=CARTESIAN_POINT('Ctrl Pts',(0.344941099461226,0.460614002623134,
-0.118418424896554));
#36354=CARTESIAN_POINT('Ctrl Pts',(0.246980934267327,0.478329925800947,
-0.268292799062886));
#36355=CARTESIAN_POINT('Ctrl Pts',(0.0895288995299929,0.49604584897876,
-0.353541847300449));
#36356=CARTESIAN_POINT('Ctrl Pts',(-0.0895198614025975,0.513761772156572,
-0.353506441262075));
#36357=CARTESIAN_POINT('Ctrl Pts',(-0.247005954023888,0.531477695334385,
-0.268319590417228));
#36358=CARTESIAN_POINT('Ctrl Pts',(-0.344906058802126,0.549193618512198,
-0.118406781736645));
#36359=CARTESIAN_POINT('Ctrl Pts',(-0.359728502950795,0.56690954169001,
0.0600284421673935));
#36360=CARTESIAN_POINT('Ctrl Pts',(-0.287770405730312,0.584625464867824,
0.223981002451209));
#36361=CARTESIAN_POINT('Ctrl Pts',(-0.146502340124411,0.602341388045636,
0.333985996548453));
#36362=CARTESIAN_POINT('Ctrl Pts',(0.0301195604177669,0.62005731122345,
0.3634161757747));
#36363=CARTESIAN_POINT('Ctrl Pts',(0.199460245847326,0.637773234401262,
0.305323295892745));
#36364=CARTESIAN_POINT('Ctrl Pts',(0.320737036978914,0.655489157579075,
0.173548309605457));
#36365=CARTESIAN_POINT('Ctrl Pts',(0.35,0.66729977303095,0.0578714436187596));
#36366=CARTESIAN_POINT('Ctrl Pts',(0.35,0.673205080756888,2.57175827820944E-16));
#36367=CARTESIAN_POINT('Origin',(0.3,0.673205080756888,2.20436423846524E-16));
#36368=CARTESIAN_POINT('Origin',(0.3,0.673205080756888,2.20436423846524E-16));
#36369=CARTESIAN_POINT('Origin',(0.3,7.2280144832367E-19,0.));
#36370=CARTESIAN_POINT('',(0.,0.,0.));
#36371=CARTESIAN_POINT('Origin',(0.,0.,0.));
#36372=CARTESIAN_POINT('',(-0.195633559071744,0.00012731057411345,0.0225869692124231));
#36373=CARTESIAN_POINT('',(-0.195587799559821,0.000207186393275607,0.0124130307875758));
#36374=CARTESIAN_POINT('',(-0.1954,-2.39295984553393E-17,0.));
#36375=CARTESIAN_POINT('',(0.0861525859670522,0.175382131162755,0.));
#36376=CARTESIAN_POINT('Ctrl Pts',(-0.195633559071744,0.00012731057411345,
0.0225869692124231));
#36377=CARTESIAN_POINT('Ctrl Pts',(-0.195680032440099,0.00682557629313676,
0.0222037301306047));
#36378=CARTESIAN_POINT('Ctrl Pts',(-0.195365903766855,0.0135191473590706,
0.0218204910487863));
#36379=CARTESIAN_POINT('Ctrl Pts',(-0.194676806606145,0.0201735328972743,
0.0214372519669679));
#36380=CARTESIAN_POINT('Ctrl Pts',(-0.188017193281744,0.0844832371344698,
0.01773353028412));
#36381=CARTESIAN_POINT('Ctrl Pts',(-0.146336311091822,0.145133095416213,
0.0140298086012721));
#36382=CARTESIAN_POINT('Ctrl Pts',(-0.0886884671668765,0.17445317403525,
0.0103260869184242));
#36383=CARTESIAN_POINT('Ctrl Pts',(-0.0351138290053491,0.201701592986141,
0.00688405794561611));
#36384=CARTESIAN_POINT('Ctrl Pts',(0.0322511385444639,0.201891139473935,
0.00344202897280807));
#36385=CARTESIAN_POINT('Ctrl Pts',(0.0863567639152679,0.175641488315944,
2.92734586571086E-18));
#36386=CARTESIAN_POINT('',(-0.0861525859670574,0.175382131162752,1.38777878078145E-17));
#36387=CARTESIAN_POINT('Origin',(0.,0.,0.));
#36388=CARTESIAN_POINT('Ctrl Pts',(-0.0861525859670571,0.175382131162752,
2.28983498828939E-16));
#36389=CARTESIAN_POINT('Ctrl Pts',(-0.144496782441851,0.146721837385109,
0.00370621399437224));
#36390=CARTESIAN_POINT('Ctrl Pts',(-0.18691020329229,0.0869083656944534,
0.00741242798874424));
#36391=CARTESIAN_POINT('Ctrl Pts',(-0.194380023116171,0.0227435527544788,
0.0111186419831163));
#36392=CARTESIAN_POINT('Ctrl Pts',(-0.195249630318745,0.0152737362394887,
0.0115501049179361));
#36393=CARTESIAN_POINT('Ctrl Pts',(-0.195645657185248,0.00774494727773659,
0.0119815678527559));
#36394=CARTESIAN_POINT('Ctrl Pts',(-0.195587799559821,0.000207186393275607,
0.0124130307875758));
#36395=CARTESIAN_POINT('Origin',(0.,0.,0.));
#36396=CARTESIAN_POINT('',(-0.195128203910989,9.79727872364722E-5,0.092586969212423));
#36397=CARTESIAN_POINT('',(-0.195118672945361,9.16100096969453E-5,0.0824130307875757));
#36398=CARTESIAN_POINT('',(-0.1954,-2.39295984553393E-17,0.));
#36399=CARTESIAN_POINT('Ctrl Pts',(-0.195128203910989,9.79727872364722E-5,
0.092586969212423));
#36400=CARTESIAN_POINT('Ctrl Pts',(-0.19524730612105,0.0263901717292074,
0.0910927268943587));
#36401=CARTESIAN_POINT('Ctrl Pts',(-0.190305141123492,0.0526394079969068,
0.0895984845762944));
#36402=CARTESIAN_POINT('Ctrl Pts',(-0.180089049647467,0.0766440059940591,
0.0881042422582301));
#36403=CARTESIAN_POINT('Ctrl Pts',(-0.154766811710363,0.136143291361155,
0.0844005205753822));
#36404=CARTESIAN_POINT('Ctrl Pts',(-0.0970428066964404,0.181852045762203,
0.0806967988925343));
#36405=CARTESIAN_POINT('Ctrl Pts',(-0.0333230591869142,0.192861999489257,
0.0769930772096863));
#36406=CARTESIAN_POINT('Ctrl Pts',(0.030396688322612,0.20387195321631,0.0732893555268384));
#36407=CARTESIAN_POINT('Ctrl Pts',(0.100112178327742,0.18018310626937,0.0695856338439906));
#36408=CARTESIAN_POINT('Ctrl Pts',(0.143930998255098,0.132629143144902,
0.0658819121611426));
#36409=CARTESIAN_POINT('Ctrl Pts',(0.187749818182454,0.0850751800204342,
0.0621781904782947));
#36410=CARTESIAN_POINT('Ctrl Pts',(0.205671968032037,0.0136561007184397,
0.0584744687954468));
#36411=CARTESIAN_POINT('Ctrl Pts',(0.189499805994521,-0.0489512382298273,
0.0547707471125989));
#36412=CARTESIAN_POINT('Ctrl Pts',(0.173327643957006,-0.111558577178094,
0.051067025429751));
#36413=CARTESIAN_POINT('Ctrl Pts',(0.123061170032392,-0.165354175772633,
0.0473633037469032));
#36414=CARTESIAN_POINT('Ctrl Pts',(0.0616932989107385,-0.18573955796291,
0.0436595820640553));
#36415=CARTESIAN_POINT('Ctrl Pts',(0.000325427789084558,-0.206124940153187,
0.0399558603812074));
#36416=CARTESIAN_POINT('Ctrl Pts',(-0.0721438405296094,-0.193100105939202,
0.0362521386983595));
#36417=CARTESIAN_POINT('Ctrl Pts',(-0.122559302459517,-0.152602913735885,
0.0325484170155115));
#36418=CARTESIAN_POINT('Ctrl Pts',(-0.167758072371516,-0.11629613001496,
0.029227934414482));
#36419=CARTESIAN_POINT('Ctrl Pts',(-0.195230901779331,-0.0579081973692791,
0.0259074518134526));
#36420=CARTESIAN_POINT('Ctrl Pts',(-0.195633559071744,0.00012731057411345,
0.0225869692124231));
#36421=CARTESIAN_POINT('Ctrl Pts',(-0.195587799559821,0.000207186393275607,
0.0124130307875758));
#36422=CARTESIAN_POINT('Ctrl Pts',(-0.195148667238412,-0.0570034995103637,
0.015687781847128));
#36423=CARTESIAN_POINT('Ctrl Pts',(-0.168562951923343,-0.114731024226281,
0.0189625329066803));
#36424=CARTESIAN_POINT('Ctrl Pts',(-0.12444215732779,-0.151113938431406,
0.0222372839662326));
#36425=CARTESIAN_POINT('Ctrl Pts',(-0.0745082529182101,-0.192290462488019,
0.0259434979606046));
#36426=CARTESIAN_POINT('Ctrl Pts',(-0.00211422530173012,-0.20612735641195,
0.0296497119549767));
#36427=CARTESIAN_POINT('Ctrl Pts',(0.0595334795120667,-0.186428772433344,
0.0333559259493488));
#36428=CARTESIAN_POINT('Ctrl Pts',(0.121181184325864,-0.166730188454737,
0.0370621399437209));
#36429=CARTESIAN_POINT('Ctrl Pts',(0.172082566336977,-0.113496126573593,
0.040768353938093));
#36430=CARTESIAN_POINT('Ctrl Pts',(0.18894870924304,-0.0510370283185346,
0.0444745679324651));
#36431=CARTESIAN_POINT('Ctrl Pts',(0.205814852149104,0.0114220699365238,
0.0481807819268372));
#36432=CARTESIAN_POINT('Ctrl Pts',(0.188645755950116,0.0831062045654966,
0.0518869959212093));
#36433=CARTESIAN_POINT('Ctrl Pts',(0.145292142815886,0.131145007703775,
0.0555932099155814));
#36434=CARTESIAN_POINT('Ctrl Pts',(0.101938529681656,0.179183810842053,
0.0592994239099535));
#36435=CARTESIAN_POINT('Ctrl Pts',(0.0324003996121834,0.203577282489637,
0.0630056379043256));
#36436=CARTESIAN_POINT('Ctrl Pts',(-0.0314654015224673,0.193172336479658,
0.0667118518986976));
#36437=CARTESIAN_POINT('Ctrl Pts',(-0.0953312026571179,0.18276739046968,
0.0704180658930697));
#36438=CARTESIAN_POINT('Ctrl Pts',(-0.153524674856946,0.137564026802139,
0.0741242798874417));
#36439=CARTESIAN_POINT('Ctrl Pts',(-0.179395555636014,0.0782560471576942,
0.0778304938818138));
#36440=CARTESIAN_POINT('Ctrl Pts',(-0.190058212652462,0.0538123240897563,
0.0793580061837345));
#36441=CARTESIAN_POINT('Ctrl Pts',(-0.195230335199157,0.0269726953471863,
0.0808855184856551));
#36442=CARTESIAN_POINT('Ctrl Pts',(-0.195118672945361,9.16100096969453E-5,
0.0824130307875757));
#36443=CARTESIAN_POINT('Origin',(0.,0.,0.));
#36444=CARTESIAN_POINT('',(-0.195279554503994,-0.000168121501241181,0.162586969212423));
#36445=CARTESIAN_POINT('',(-0.195287184048439,-0.0001702989282844,0.152413030787576));
#36446=CARTESIAN_POINT('',(-0.1954,-2.39295984553393E-17,0.));
#36447=CARTESIAN_POINT('Ctrl Pts',(-0.195279554503994,-0.000168121501241181,
0.162586969212423));
#36448=CARTESIAN_POINT('Ctrl Pts',(-0.194903656010943,0.0455834752155161,
0.159981723658113));
#36449=CARTESIAN_POINT('Ctrl Pts',(-0.178856730317397,0.091572573117829,
0.157376478103802));
#36450=CARTESIAN_POINT('Ctrl Pts',(-0.149500760249196,0.126316552728133,
0.154771232549492));
#36451=CARTESIAN_POINT('Ctrl Pts',(-0.107767134532898,0.175709989142681,
0.151067510866644));
#36452=CARTESIAN_POINT('Ctrl Pts',(-0.039135122029848,0.202376358702057,
0.147363789183796));
#36453=CARTESIAN_POINT('Ctrl Pts',(0.0249990333148566,0.194116955279127,
0.143660067500948));
#36454=CARTESIAN_POINT('Ctrl Pts',(0.0891331886595613,0.185857551856197,
0.139956345818101));
#36455=CARTESIAN_POINT('Ctrl Pts',(0.14876948684592,0.142672375450961,0.136252624135253));
#36456=CARTESIAN_POINT('Ctrl Pts',(0.176626827046517,0.0843167597229759,
0.132548902452405));
#36457=CARTESIAN_POINT('Ctrl Pts',(0.204484167247113,0.0259611439949913,
0.128845180769557));
#36458=CARTESIAN_POINT('Ctrl Pts',(0.200562549461947,-0.0475649110557425,
0.125141459086709));
#36459=CARTESIAN_POINT('Ctrl Pts',(0.166655969053473,-0.102626219289756,
0.121437737403861));
#36460=CARTESIAN_POINT('Ctrl Pts',(0.132749388644999,-0.157687527523771,
0.117734015721013));
#36461=CARTESIAN_POINT('Ctrl Pts',(0.0688578456132156,-0.194284088941065,
0.114030294038165));
#36462=CARTESIAN_POINT('Ctrl Pts',(0.00420898544956178,-0.19567474659654,
0.110326572355317));
#36463=CARTESIAN_POINT('Ctrl Pts',(-0.0604398747140919,-0.197065404252014,
0.106622850672469));
#36464=CARTESIAN_POINT('Ctrl Pts',(-0.125846052009616,-0.16325015814567,
0.102919128989622));
#36465=CARTESIAN_POINT('Ctrl Pts',(-0.162088905227235,-0.109697626925925,
0.0992154073067737));
#36466=CARTESIAN_POINT('Ctrl Pts',(-0.183709816073764,-0.0777505145902677,
0.0970059279419901));
#36467=CARTESIAN_POINT('Ctrl Pts',(-0.194952091996443,-0.0387793032173158,
0.0947964485772066));
#36468=CARTESIAN_POINT('Ctrl Pts',(-0.195128203910989,9.79727872364722E-5,
0.092586969212423));
#36469=CARTESIAN_POINT('Ctrl Pts',(-0.195118672945361,9.16100096969453E-5,
0.0824130307875757));
#36470=CARTESIAN_POINT('Ctrl Pts',(-0.194959408276249,-0.0382490737583375,
0.0845917324800272));
#36471=CARTESIAN_POINT('Ctrl Pts',(-0.184051065227066,-0.0766740948347571,
0.0867704341724787));
#36472=CARTESIAN_POINT('Ctrl Pts',(-0.162993550876047,-0.10835175828476,
0.0889491358649302));
#36473=CARTESIAN_POINT('Ctrl Pts',(-0.127172375978705,-0.162238988461419,
0.0926553498593023));
#36474=CARTESIAN_POINT('Ctrl Pts',(-0.0619817368257128,-0.196600853193387,
0.0963615638536743));
#36475=CARTESIAN_POINT('Ctrl Pts',(0.0027186436745272,-0.195701720127518,
0.100067777848046));
#36476=CARTESIAN_POINT('Ctrl Pts',(0.0674190241747668,-0.194802587061648,
0.103773991842418));
#36477=CARTESIAN_POINT('Ctrl Pts',(0.131629146022255,-0.15864245619794,
0.107480205836791));
#36478=CARTESIAN_POINT('Ctrl Pts',(0.165939903784035,-0.103781956343241,
0.111186419831163));
#36479=CARTESIAN_POINT('Ctrl Pts',(0.200250661545815,-0.0489214564885407,
0.114892633825535));
#36480=CARTESIAN_POINT('Ctrl Pts',(0.204662055221888,0.0246394123571516,
0.118598847819907));
#36481=CARTESIAN_POINT('Ctrl Pts',(0.177153295980734,0.0832073910176122,
0.122305061814279));
#36482=CARTESIAN_POINT('Ctrl Pts',(0.149644536739581,0.141775369678073,
0.126011275808651));
#36483=CARTESIAN_POINT('Ctrl Pts',(0.0902156245812001,0.185350458153303,
0.129717489803023));
#36484=CARTESIAN_POINT('Ctrl Pts',(0.0260864347694114,0.193974733338565,
0.133423703797395));
#36485=CARTESIAN_POINT('Ctrl Pts',(-0.0380427550423769,0.202599008523827,
0.137129917791767));
#36486=CARTESIAN_POINT('Ctrl Pts',(-0.106872222507573,0.176272470419122,
0.140836131786139));
#36487=CARTESIAN_POINT('Ctrl Pts',(-0.148876654315921,0.127053027794487,
0.144542345780511));
#36488=CARTESIAN_POINT('Ctrl Pts',(-0.178610829781436,0.0922114770268632,
0.147165907449533));
#36489=CARTESIAN_POINT('Ctrl Pts',(-0.194903067523895,0.0458983666015645,
0.149789469118554));
#36490=CARTESIAN_POINT('Ctrl Pts',(-0.195287184048439,-0.0001702989282844,
0.152413030787576));
#36491=CARTESIAN_POINT('Origin',(0.,0.,0.));
#36492=CARTESIAN_POINT('',(-0.19571996697324,4.08272333451705E-6,0.232586969212423));
#36493=CARTESIAN_POINT('',(-0.195720915199432,4.37834080700025E-6,0.222413030787575));
#36494=CARTESIAN_POINT('',(-0.1954,-2.39295984553393E-17,0.));
#36495=CARTESIAN_POINT('Ctrl Pts',(-0.19571996697324,4.08272333451705E-6,
0.232586969212423));
#36496=CARTESIAN_POINT('Ctrl Pts',(-0.19573993069631,0.0648866965015804,
0.228870720421867));
#36497=CARTESIAN_POINT('Ctrl Pts',(-0.160252793092098,0.129750264469882,
0.225154471631311));
#36498=CARTESIAN_POINT('Ctrl Pts',(-0.105631192010051,0.164767712566922,
0.221438222840754));
#36499=CARTESIAN_POINT('Ctrl Pts',(-0.0511937149515876,0.19966712030426,
0.217734501157906));
#36500=CARTESIAN_POINT('Ctrl Pts',(0.0222490761444335,0.204921286910345,
0.214030779475058));
#36501=CARTESIAN_POINT('Ctrl Pts',(0.0811002035332165,0.178126653559889,
0.210327057792211));
#36502=CARTESIAN_POINT('Ctrl Pts',(0.139951330921999,0.151332020209433,
0.206623336109363));
#36503=CARTESIAN_POINT('Ctrl Pts',(0.184210794603544,0.0924885869024359,
0.202919614426515));
#36504=CARTESIAN_POINT('Ctrl Pts',(0.193631757329266,0.028514740055385,
0.199215892743667));
#36505=CARTESIAN_POINT('Ctrl Pts',(0.203052720054988,-0.0354591067916664,
0.195512171060819));
#36506=CARTESIAN_POINT('Ctrl Pts',(0.177635181824887,-0.104563367178771,
0.191808449377971));
#36507=CARTESIAN_POINT('Ctrl Pts',(0.129006594271768,-0.147185755477259,
0.188104727695123));
#36508=CARTESIAN_POINT('Ctrl Pts',(0.0803780067186484,-0.189808143775746,
0.184401006012275));
#36509=CARTESIAN_POINT('Ctrl Pts',(0.00853836984250916,-0.205948659985616,
0.180697284329427));
#36510=CARTESIAN_POINT('Ctrl Pts',(-0.0536487147273854,-0.188223703762279,
0.176993562646579));
#36511=CARTESIAN_POINT('Ctrl Pts',(-0.11583579929728,-0.170498747538942,
0.173289840963732));
#36512=CARTESIAN_POINT('Ctrl Pts',(-0.168370331560931,-0.118908318882399,
0.169586119280884));
#36513=CARTESIAN_POINT('Ctrl Pts',(-0.187219978227984,-0.0570528529192665,
0.165882397598036));
#36514=CARTESIAN_POINT('Ctrl Pts',(-0.192810540551016,-0.0387073187246384,
0.164783921469498));
#36515=CARTESIAN_POINT('Ctrl Pts',(-0.195438048401311,-0.0194588316428207,
0.163685445340961));
#36516=CARTESIAN_POINT('Ctrl Pts',(-0.195279554503994,-0.000168121501241181,
0.162586969212423));
#36517=CARTESIAN_POINT('Ctrl Pts',(-0.195287184048439,-0.0001702989282844,
0.152413030787576));
#36518=CARTESIAN_POINT('Ctrl Pts',(-0.195445695530526,-0.0191812291650776,
0.153495683112926));
#36519=CARTESIAN_POINT('Ctrl Pts',(-0.192895173588402,-0.0381505322742495,
0.154578335438277));
#36520=CARTESIAN_POINT('Ctrl Pts',(-0.187462310228399,-0.0562548805321496,
0.155660987763628));
#36521=CARTESIAN_POINT('Ctrl Pts',(-0.168864138181028,-0.118230999089587,
0.159367201758));
#36522=CARTESIAN_POINT('Ctrl Pts',(-0.116488397934787,-0.170070889059896,
0.163073415752372));
#36523=CARTESIAN_POINT('Ctrl Pts',(-0.0543243355780667,-0.188030816136644,
0.166779629746744));
#36524=CARTESIAN_POINT('Ctrl Pts',(0.0078397267786532,-0.205990743213392,
0.170485843741116));
#36525=CARTESIAN_POINT('Ctrl Pts',(0.0797921112458524,-0.190070707396579,
0.174192057735488));
#36526=CARTESIAN_POINT('Ctrl Pts',(0.128577075941843,-0.147562399010748,
0.17789827172986));
#36527=CARTESIAN_POINT('Ctrl Pts',(0.177362040637834,-0.105054090624917,
0.181604485724232));
#36528=CARTESIAN_POINT('Ctrl Pts',(0.202979585562615,-0.0359575096700667,
0.185310699718604));
#36529=CARTESIAN_POINT('Ctrl Pts',(0.193696313672928,0.028079594435252,
0.189016913712976));
#36530=CARTESIAN_POINT('Ctrl Pts',(0.184413041783241,0.0921166985405712,
0.192723127707349));
#36531=CARTESIAN_POINT('Ctrl Pts',(0.140228953079084,0.151094325796358,
0.196429341701721));
#36532=CARTESIAN_POINT('Ctrl Pts',(0.0813813216582781,0.177999452248681,
0.200135555696093));
#36533=CARTESIAN_POINT('Ctrl Pts',(0.0225336902374724,0.204904578701004,
0.203841769690465));
#36534=CARTESIAN_POINT('Ctrl Pts',(-0.0509774838999832,0.199737204349863,
0.207547983684837));
#36535=CARTESIAN_POINT('Ctrl Pts',(-0.105482489992153,0.164864094185095,
0.211254197679209));
#36536=CARTESIAN_POINT('Ctrl Pts',(-0.16018451812442,0.129864926401004,
0.214973808715331));
#36537=CARTESIAN_POINT('Ctrl Pts',(-0.195742302622205,0.0649448754401196,
0.218693419751453));
#36538=CARTESIAN_POINT('Ctrl Pts',(-0.195720915199432,4.37834080700025E-6,
0.222413030787575));
#36539=CARTESIAN_POINT('Origin',(0.,0.,0.));
#36540=CARTESIAN_POINT('',(-0.195267691385146,0.000165493661177622,0.302586969212423));
#36541=CARTESIAN_POINT('',(-0.195274315056508,0.000167675988910205,0.292413030787576));
#36542=CARTESIAN_POINT('',(-0.1954,-2.39295984553393E-17,0.));
#36543=CARTESIAN_POINT('Ctrl Pts',(-0.195267691385146,0.000165493661177622,
0.302586969212423));
#36544=CARTESIAN_POINT('Ctrl Pts',(-0.195426560914452,0.0198992208020636,
0.301463438868469));
#36545=CARTESIAN_POINT('Ctrl Pts',(-0.192675342506316,0.0395896803504792,
0.300339908524515));
#36546=CARTESIAN_POINT('Ctrl Pts',(-0.186830808103941,0.0583146374609883,
0.29921637818056));
#36547=CARTESIAN_POINT('Ctrl Pts',(-0.167564280138135,0.120041523640586,
0.295512656497712));
#36548=CARTESIAN_POINT('Ctrl Pts',(-0.114682887836242,0.171276357431471,
0.291808934814864));
#36549=CARTESIAN_POINT('Ctrl Pts',(-0.0523776367443795,0.188581364320311,
0.288105213132016));
#36550=CARTESIAN_POINT('Ctrl Pts',(0.00992761434748341,0.20588637120915,
0.284401491449168));
#36551=CARTESIAN_POINT('Ctrl Pts',(0.0816567242293159,0.189261551195942,
0.280697769766321));
#36552=CARTESIAN_POINT('Ctrl Pts',(0.129996651882171,0.146312057934516,
0.276994048083473));
#36553=CARTESIAN_POINT('Ctrl Pts',(0.178336579535026,0.103362564673089,
0.273290326400625));
#36554=CARTESIAN_POINT('Ctrl Pts',(0.203287324958903,0.0340883981634439,
0.269586604717777));
#36555=CARTESIAN_POINT('Ctrl Pts',(0.193434974962867,-0.0298204336020968,
0.265882883034929));
#36556=CARTESIAN_POINT('Ctrl Pts',(0.183582624966831,-0.0937292653676373,
0.262179161352081));
#36557=CARTESIAN_POINT('Ctrl Pts',(0.138927179550881,-0.152272762389073,
0.258475439669233));
#36558=CARTESIAN_POINT('Ctrl Pts',(0.0798966206784796,-0.178669745083631,
0.254771717986385));
#36559=CARTESIAN_POINT('Ctrl Pts',(0.0208660618060775,-0.205066727778188,
0.251067996303538));
#36560=CARTESIAN_POINT('Ctrl Pts',(-0.0525396105227766,-0.199317196145866,
0.24736427462069));
#36561=CARTESIAN_POINT('Ctrl Pts',(-0.10674039873032,-0.16405131839538,
0.243660552937842));
#36562=CARTESIAN_POINT('Ctrl Pts',(-0.160757863467609,-0.128904720517098,
0.239969358362702));
#36563=CARTESIAN_POINT('Ctrl Pts',(-0.195700137841649,-0.0644411052866131,
0.236278163787563));
#36564=CARTESIAN_POINT('Ctrl Pts',(-0.19571996697324,4.08272333451705E-6,
0.232586969212423));
#36565=CARTESIAN_POINT('Ctrl Pts',(-0.195720915199432,4.37834080700025E-6,
0.222413030787575));
#36566=CARTESIAN_POINT('Ctrl Pts',(-0.195699681840184,-0.0644683222376,
0.226105847740198));
#36567=CARTESIAN_POINT('Ctrl Pts',(-0.160725113883781,-0.128960760246236,
0.22979866469282));
#36568=CARTESIAN_POINT('Ctrl Pts',(-0.106669244200308,-0.164098742623895,
0.233491481645442));
#36569=CARTESIAN_POINT('Ctrl Pts',(-0.0524172671136578,-0.199364200861572,
0.237197695639814));
#36570=CARTESIAN_POINT('Ctrl Pts',(0.0210547116140745,-0.205061829112049,
0.240903909634186));
#36571=CARTESIAN_POINT('Ctrl Pts',(0.0800949322066953,-0.178581989384044,
0.244610123628558));
#36572=CARTESIAN_POINT('Ctrl Pts',(0.139135152799316,-0.152102149656038,
0.24831633762293));
#36573=CARTESIAN_POINT('Ctrl Pts',(0.183743615256826,-0.0934448419495488,
0.252022551617302));
#36574=CARTESIAN_POINT('Ctrl Pts',(0.193488676008295,-0.0294763859316313,
0.255728765611674));
#36575=CARTESIAN_POINT('Ctrl Pts',(0.203233736759764,0.0344920700862864,
0.259434979606046));
#36576=CARTESIAN_POINT('Ctrl Pts',(0.178115395805193,0.103771674415633,
0.263141193600418));
#36577=CARTESIAN_POINT('Ctrl Pts',(0.129638398231036,0.146630865646616,
0.26684740759479));
#36578=CARTESIAN_POINT('Ctrl Pts',(0.0811614006568792,0.1894900568776,0.270553621589162));
#36579=CARTESIAN_POINT('Ctrl Pts',(0.00932574646313782,0.205928835010221,
0.274259835583535));
#36580=CARTESIAN_POINT('Ctrl Pts',(-0.0529662765081927,0.188417882975093,
0.277966049577907));
#36581=CARTESIAN_POINT('Ctrl Pts',(-0.115258299479523,0.170906930939964,
0.281672263572279));
#36582=CARTESIAN_POINT('Ctrl Pts',(-0.168006691228442,0.119446248737086,
0.285378477566651));
#36583=CARTESIAN_POINT('Ctrl Pts',(-0.187051544101399,0.0576059451476712,
0.289084691561023));
#36584=CARTESIAN_POINT('Ctrl Pts',(-0.192752575844056,0.0390941962730205,
0.290194137969874));
#36585=CARTESIAN_POINT('Ctrl Pts',(-0.195433466869055,0.0196523398123763,
0.291303584378725));
#36586=CARTESIAN_POINT('Ctrl Pts',(-0.195274315056508,0.000167675988910205,
0.292413030787576));
#36587=CARTESIAN_POINT('Origin',(0.,0.,0.));
#36588=CARTESIAN_POINT('',(-0.195135107115213,-0.000103745302926256,0.372586969212423));
#36589=CARTESIAN_POINT('',(-0.195125983814034,-9.67513988672578E-5,0.362413030787576));
#36590=CARTESIAN_POINT('',(-0.1954,-2.39295984553393E-17,0.));
#36591=CARTESIAN_POINT('Ctrl Pts',(-0.195135107115213,-0.000103745302926256,
0.372586969212423));
#36592=CARTESIAN_POINT('Ctrl Pts',(-0.19494564270682,0.0392108141373472,
0.370352435632223));
#36593=CARTESIAN_POINT('Ctrl Pts',(-0.183428685915158,0.078627490539017,
0.368117902052023));
#36594=CARTESIAN_POINT('Ctrl Pts',(-0.161345116677478,0.110788542383069,
0.365883368471823));
#36595=CARTESIAN_POINT('Ctrl Pts',(-0.124741775852795,0.164095230684139,
0.362179646788975));
#36596=CARTESIAN_POINT('Ctrl Pts',(-0.0591089924893776,0.197468687095231,
0.358475925106126));
#36597=CARTESIAN_POINT('Ctrl Pts',(0.00552900452708404,0.195641963566092,
0.354772203423278));
#36598=CARTESIAN_POINT('Ctrl Pts',(0.0701670015435453,0.193815240036952,
0.351068481740431));
#36599=CARTESIAN_POINT('Ctrl Pts',(0.13381021221305,0.156788336567581,0.347364760057583));
#36600=CARTESIAN_POINT('Ctrl Pts',(0.16734455320356,0.101499499073225,0.343661038374735));
#36601=CARTESIAN_POINT('Ctrl Pts',(0.20087889419407,0.0462106615788698,
0.339957316691887));
#36602=CARTESIAN_POINT('Ctrl Pts',(0.204304365505584,-0.0273401099404705,
0.336253595009039));
#36603=CARTESIAN_POINT('Ctrl Pts',(0.176053958557416,-0.0855064411333041,
0.332549873326191));
#36604=CARTESIAN_POINT('Ctrl Pts',(0.147803551609248,-0.143672772326139,
0.328846151643343));
#36605=CARTESIAN_POINT('Ctrl Pts',(0.0878772664013962,-0.186454663192466,
0.325142429960495));
#36606=CARTESIAN_POINT('Ctrl Pts',(0.0236888497103484,-0.194281203925035,
0.321438708277648));
#36607=CARTESIAN_POINT('Ctrl Pts',(-0.0404995669806982,-0.202107744657604,
0.3177349865948));
#36608=CARTESIAN_POINT('Ctrl Pts',(-0.108950115154941,-0.174978935256416,
0.314031264911952));
#36609=CARTESIAN_POINT('Ctrl Pts',(-0.150349557427203,-0.125305061271667,
0.310327543229104));
#36610=CARTESIAN_POINT('Ctrl Pts',(-0.179190407667273,-0.0906998424134863,
0.30774735189021));
#36611=CARTESIAN_POINT('Ctrl Pts',(-0.194902846959061,-0.0451530792879088,
0.305167160551317));
#36612=CARTESIAN_POINT('Ctrl Pts',(-0.195267691385146,0.000165493661177622,
0.302586969212423));
#36613=CARTESIAN_POINT('Ctrl Pts',(-0.195274315056508,0.000167675988910205,
0.292413030787576));
#36614=CARTESIAN_POINT('Ctrl Pts',(-0.194901804708373,-0.045438081105706,
0.295009798373097));
#36615=CARTESIAN_POINT('Ctrl Pts',(-0.178970412039892,-0.0912783539307832,
0.297606565958618));
#36616=CARTESIAN_POINT('Ctrl Pts',(-0.149789482266332,-0.125975537577289,
0.300203333544139));
#36617=CARTESIAN_POINT('Ctrl Pts',(-0.108141253561316,-0.175496791736879,
0.303909547538511));
#36618=CARTESIAN_POINT('Ctrl Pts',(-0.03950348215429,-0.202319375080107,
0.307615761532883));
#36619=CARTESIAN_POINT('Ctrl Pts',(0.0246862437687336,-0.194157962588032,
0.311321975527255));
#36620=CARTESIAN_POINT('Ctrl Pts',(0.0888759696917571,-0.185996550095957,
0.315028189521628));
#36621=CARTESIAN_POINT('Ctrl Pts',(0.148617650130778,-0.14285114176858,
0.318734403516));
#36622=CARTESIAN_POINT('Ctrl Pts',(0.176548299529208,-0.084483270534745,
0.322440617510372));
#36623=CARTESIAN_POINT('Ctrl Pts',(0.204478948927638,-0.0261153993009101,
0.326146831504744));
#36624=CARTESIAN_POINT('Ctrl Pts',(0.200598567285476,0.0474749348393822,
0.329853045499116));
#36625=CARTESIAN_POINT('Ctrl Pts',(0.166684453569178,0.102581762536563,
0.333559259493488));
#36626=CARTESIAN_POINT('Ctrl Pts',(0.13277033985288,0.157688590233743,0.33726547348786));
#36627=CARTESIAN_POINT('Ctrl Pts',(0.0688224940624468,0.194311911487812,
0.340971687482232));
#36628=CARTESIAN_POINT('Ctrl Pts',(0.00413041672205065,0.195677450731496,
0.344677901476604));
#36629=CARTESIAN_POINT('Ctrl Pts',(-0.0605616606183457,0.19704298997518,
0.348384115470976));
#36630=CARTESIAN_POINT('Ctrl Pts',(-0.125997969508704,0.163150747208479,
0.352090329465349));
#36631=CARTESIAN_POINT('Ctrl Pts',(-0.162207261036362,0.109524104808107,
0.355796543459721));
#36632=CARTESIAN_POINT('Ctrl Pts',(-0.183754705311226,0.0776119342016343,
0.358002039235672));
#36633=CARTESIAN_POINT('Ctrl Pts',(-0.194952253842872,0.0387114015523011,
0.360207535011624));
#36634=CARTESIAN_POINT('Ctrl Pts',(-0.195125983814034,-9.67513988672578E-5,
0.362413030787576));
#36635=CARTESIAN_POINT('Origin',(0.,0.,0.));
#36636=CARTESIAN_POINT('',(-0.195645574651684,-0.000107576288577632,0.442586969212423));
#36637=CARTESIAN_POINT('',(-0.195628130950281,-0.000119277919923279,0.432413030787576));
#36638=CARTESIAN_POINT('',(-0.1954,-2.39295984553393E-17,0.));
#36639=CARTESIAN_POINT('Ctrl Pts',(-0.195645574651684,-0.000107576288577632,
0.442586969212423));
#36640=CARTESIAN_POINT('Ctrl Pts',(-0.195258201164419,0.0583617837825317,
0.439241432395977));
#36641=CARTESIAN_POINT('Ctrl Pts',(-0.167312331125722,0.117152394520949,
0.435895895579531));
#36642=CARTESIAN_POINT('Ctrl Pts',(-0.121525966387556,0.153420296221226,
0.432550358763085));
#36643=CARTESIAN_POINT('Ctrl Pts',(-0.070837553387317,0.193571166257503,
0.428846637080237));
#36644=CARTESIAN_POINT('Ctrl Pts',(0.00171598407939347,0.206118438706562,
0.425142915397389));
#36645=CARTESIAN_POINT('Ctrl Pts',(0.0629444641593513,0.18532226587955,
0.421439193714541));
#36646=CARTESIAN_POINT('Ctrl Pts',(0.124172944239309,0.164526093052537,
0.417735472031693));
#36647=CARTESIAN_POINT('Ctrl Pts',(0.174076366932515,0.110386474949453,
0.414031750348845));
#36648=CARTESIAN_POINT('Ctrl Pts',(0.189826022128925,0.0476700023258525,
0.410328028665997));
#36649=CARTESIAN_POINT('Ctrl Pts',(0.205575677325334,-0.0150464702977478,
0.406624306983149));
#36650=CARTESIAN_POINT('Ctrl Pts',(0.187171565024948,-0.086339797441863,
0.402920585300301));
#36651=CARTESIAN_POINT('Ctrl Pts',(0.143032790007833,-0.133596290298842,
0.399216863617453));
#36652=CARTESIAN_POINT('Ctrl Pts',(0.0988940149907184,-0.180852783155821,
0.395513141934605));
#36653=CARTESIAN_POINT('Ctrl Pts',(0.0290205772568748,-0.204072441725662,
0.391809420251758));
#36654=CARTESIAN_POINT('Ctrl Pts',(-0.0346233738762281,-0.192633252011348,
0.38810569856891));
#36655=CARTESIAN_POINT('Ctrl Pts',(-0.0982673250093302,-0.181194062297035,
0.384401976886062));
#36656=CARTESIAN_POINT('Ctrl Pts',(-0.155681789541692,-0.135096024298568,
0.380698255203214));
#36657=CARTESIAN_POINT('Ctrl Pts',(-0.1806020726649,-0.0754270452038098,
0.376994533520366));
#36658=CARTESIAN_POINT('Ctrl Pts',(-0.190487422217158,-0.0517576224744695,
0.375525345417718));
#36659=CARTESIAN_POINT('Ctrl Pts',(-0.19525967846073,-0.0259527562563923,
0.374056157315071));
#36660=CARTESIAN_POINT('Ctrl Pts',(-0.195135107115213,-0.000103745302926256,
0.372586969212423));
#36661=CARTESIAN_POINT('Ctrl Pts',(-0.195125983814034,-9.67513988672578E-5,
0.362413030787576));
#36662=CARTESIAN_POINT('Ctrl Pts',(-0.195244197476311,-0.0265035587897937,
0.363913749005996));
#36663=CARTESIAN_POINT('Ctrl Pts',(-0.190258326051973,-0.0528675939020291,
0.365414467224416));
#36664=CARTESIAN_POINT('Ctrl Pts',(-0.1799560505048,-0.0769580726996389,
0.366915185442837));
#36665=CARTESIAN_POINT('Ctrl Pts',(-0.154513274280624,-0.136452565772967,
0.370621399437209));
#36666=CARTESIAN_POINT('Ctrl Pts',(-0.0966454476673152,-0.18208050988558,
0.374327613431581));
#36667=CARTESIAN_POINT('Ctrl Pts',(-0.0328572905191125,-0.192943316874967,
0.378033827425953));
#36668=CARTESIAN_POINT('Ctrl Pts',(0.0309308666290907,-0.203806123864353,
0.381740041420325));
#36669=CARTESIAN_POINT('Ctrl Pts',(0.100639354312189,-0.179903793730513,
0.385446255414697));
#36670=CARTESIAN_POINT('Ctrl Pts',(0.144340173058911,-0.132184112162819,
0.389152469409069));
#36671=CARTESIAN_POINT('Ctrl Pts',(0.188040991805633,-0.0844644305951239,
0.392858683403441));
#36672=CARTESIAN_POINT('Ctrl Pts',(0.205734141615979,-0.0129273975935752,
0.396564897397814));
#36673=CARTESIAN_POINT('Ctrl Pts',(0.189315776078089,0.0496614739501458,
0.400271111392186));
#36674=CARTESIAN_POINT('Ctrl Pts',(0.172897410540198,0.112250345493866,
0.403977325386558));
#36675=CARTESIAN_POINT('Ctrl Pts',(0.122367529654071,0.165891055579759,
0.40768353938093));
#36676=CARTESIAN_POINT('Ctrl Pts',(0.0608699149567017,0.186014995417357,
0.411389753375302));
#36677=CARTESIAN_POINT('Ctrl Pts',(-0.000627699740667481,0.206138935254955,
0.415095967369674));
#36678=CARTESIAN_POINT('Ctrl Pts',(-0.0730930482492791,0.19274610484426,
0.418802181364046));
#36679=CARTESIAN_POINT('Ctrl Pts',(-0.123335429038162,0.151970711029871,
0.422508395358418));
#36680=CARTESIAN_POINT('Ctrl Pts',(-0.168092015819396,0.115647443240051,
0.425809940501471));
#36681=CARTESIAN_POINT('Ctrl Pts',(-0.195213599025838,0.0575947822566119,
0.429111485644523));
#36682=CARTESIAN_POINT('Ctrl Pts',(-0.195628130950281,-0.000119277919923279,
0.432413030787576));
#36683=CARTESIAN_POINT('Origin',(0.,0.,0.));
#36684=CARTESIAN_POINT('',(-0.195458266482996,0.000173443779922018,0.512586969212423));
#36685=CARTESIAN_POINT('',(-0.195491180920002,0.000168629508682236,0.502413030787576));
#36686=CARTESIAN_POINT('',(-0.1954,-2.39295984553393E-17,0.));
#36687=CARTESIAN_POINT('Ctrl Pts',(-0.195458266482996,0.000173443779922018,
0.512586969212423));
#36688=CARTESIAN_POINT('Ctrl Pts',(-0.195579683437623,0.013363129532035,
0.511834150842579));
#36689=CARTESIAN_POINT('Ctrl Pts',(-0.194358523444966,0.0265304620125551,
0.511081332472735));
#36690=CARTESIAN_POINT('Ctrl Pts',(-0.191712292268468,0.0394048828472761,
0.510328514102891));
#36691=CARTESIAN_POINT('Ctrl Pts',(-0.178693343503641,0.10274455880328,
0.506624792420043));
#36692=CARTESIAN_POINT('Ctrl Pts',(-0.131181246839585,0.158994452273665,
0.502921070737195));
#36693=CARTESIAN_POINT('Ctrl Pts',(-0.0709107816346671,0.18242261056952,
0.499217349054347));
#36694=CARTESIAN_POINT('Ctrl Pts',(-0.0106403164297495,0.205850768865374,
0.495513627371499));
#36695=CARTESIAN_POINT('Ctrl Pts',(0.0623885173160298,0.196457191986698,
0.491809905688651));
#36696=CARTESIAN_POINT('Ctrl Pts',(0.114768109757825,0.158539044975217,
0.488106184005803));
#36697=CARTESIAN_POINT('Ctrl Pts',(0.167147702199619,0.120620897963737,
0.484402462322955));
#36698=CARTESIAN_POINT('Ctrl Pts',(0.19887805333743,0.0541781808194522,
0.480698740640107));
#36699=CARTESIAN_POINT('Ctrl Pts',(0.195443866449662,-0.0103943670439598,
0.476995018957259));
#36700=CARTESIAN_POINT('Ctrl Pts',(0.192009679561895,-0.0749669149073727,
0.473291297274411));
#36701=CARTESIAN_POINT('Ctrl Pts',(0.153410954648549,-0.137669293489913,
0.469587575591563));
#36702=CARTESIAN_POINT('Ctrl Pts',(0.0973049796091196,-0.169817810439032,
0.465883853908716));
#36703=CARTESIAN_POINT('Ctrl Pts',(0.0411990045696909,-0.20196632738815,
0.462180132225868));
#36704=CARTESIAN_POINT('Ctrl Pts',(-0.0324142205958206,-0.203560982703848,
0.45847641054302));
#36705=CARTESIAN_POINT('Ctrl Pts',(-0.0898597516275757,-0.17387228886878,
0.454772688860172));
#36706=CARTESIAN_POINT('Ctrl Pts',(-0.147305282659331,-0.144183595033712,
0.451068967177324));
#36707=CARTESIAN_POINT('Ctrl Pts',(-0.18858311955733,-0.0832115520478776,
0.447365245494476));
#36708=CARTESIAN_POINT('Ctrl Pts',(-0.194810393739446,-0.0188482967432128,
0.443661523811628));
#36709=CARTESIAN_POINT('Ctrl Pts',(-0.19541262996613,-0.0126237620787308,
0.443303338945226));
#36710=CARTESIAN_POINT('Ctrl Pts',(-0.195687048211354,-0.00636751036633503,
0.442945154078825));
#36711=CARTESIAN_POINT('Ctrl Pts',(-0.195645574651684,-0.000107576288577632,
0.442586969212423));
#36712=CARTESIAN_POINT('Ctrl Pts',(-0.195628130950281,-0.000119277919923279,
0.432413030787576));
#36713=CARTESIAN_POINT('Ctrl Pts',(-0.195678939935296,-0.00719326340995119,
0.432817699638895));
#36714=CARTESIAN_POINT('Ctrl Pts',(-0.195328521122814,-0.014262162001596,
0.433222368490215));
#36715=CARTESIAN_POINT('Ctrl Pts',(-0.194560169264522,-0.0212853377401693,
0.433627037341534));
#36716=CARTESIAN_POINT('Ctrl Pts',(-0.187523115632842,-0.0856080354777335,
0.437333251335906));
#36717=CARTESIAN_POINT('Ctrl Pts',(-0.145429595300328,-0.146095473734778,
0.441039465330279));
#36718=CARTESIAN_POINT('Ctrl Pts',(-0.0875593536694013,-0.175043093699665,
0.444745679324651));
#36719=CARTESIAN_POINT('Ctrl Pts',(-0.0296891120384743,-0.203990713664554,
0.448451893319023));
#36720=CARTESIAN_POINT('Ctrl Pts',(0.0439578508908652,-0.201398515337285,
0.452158107313395));
#36721=CARTESIAN_POINT('Ctrl Pts',(0.09964962855145,-0.168453781781564,
0.455864321307767));
#36722=CARTESIAN_POINT('Ctrl Pts',(0.155341406212034,-0.135509048225843,
0.459570535302139));
#36723=CARTESIAN_POINT('Ctrl Pts',(0.193077998603865,-0.072211779441669,
0.463276749296511));
#36724=CARTESIAN_POINT('Ctrl Pts',(0.195575227831571,-0.00755349757277263,
0.466982963290883));
#36725=CARTESIAN_POINT('Ctrl Pts',(0.198072457059277,0.0571047842961237,
0.470689177285256));
#36726=CARTESIAN_POINT('Ctrl Pts',(0.16533032312286,0.123124079249743,0.474395391279627));
#36727=CARTESIAN_POINT('Ctrl Pts',(0.112345433605614,0.160266118112717,
0.478101605273999));
#36728=CARTESIAN_POINT('Ctrl Pts',(0.059360544088369,0.197408156975691,
0.481807819268371));
#36729=CARTESIAN_POINT('Ctrl Pts',(-0.0138671010097046,0.20567293974802,
0.485514033262744));
#36730=CARTESIAN_POINT('Ctrl Pts',(-0.0737976517839776,0.181275016640803,
0.489220247257116));
#36731=CARTESIAN_POINT('Ctrl Pts',(-0.133728202558251,0.156877093533586,
0.492926461251488));
#36732=CARTESIAN_POINT('Ctrl Pts',(-0.180361659008724,0.0998164645468222,
0.49663267524586));
#36733=CARTESIAN_POINT('Ctrl Pts',(-0.192338886510923,0.0362281355122108,
0.500338889240232));
#36734=CARTESIAN_POINT('Ctrl Pts',(-0.194573194011967,0.0243659678682544,
0.501030269756014));
#36735=CARTESIAN_POINT('Ctrl Pts',(-0.195601481281436,0.0122766393772507,
0.501721650271795));
#36736=CARTESIAN_POINT('Ctrl Pts',(-0.195491180920002,0.000168629508682236,
0.502413030787576));
#36737=CARTESIAN_POINT('Origin',(0.,0.,0.));
#36738=CARTESIAN_POINT('',(-0.19507978584999,-3.45334863967226E-6,0.582586969212423));
#36739=CARTESIAN_POINT('',(-0.195080468396925,1.8981806121043E-5,0.572413030787576));
#36740=CARTESIAN_POINT('',(-0.1954,-2.39295984553393E-17,0.));
#36741=CARTESIAN_POINT('Ctrl Pts',(-0.195079815420139,-3.45302974047446E-6,
0.582586969212423));
#36742=CARTESIAN_POINT('Ctrl Pts',(-0.195074640707532,0.0328120037045956,
0.580723147606333));
#36743=CARTESIAN_POINT('Ctrl Pts',(-0.187237758907749,0.0656297824114404,
0.578859326000243));
#36744=CARTESIAN_POINT('Ctrl Pts',(-0.1715829951129,0.0941574404236039,
0.576995504394152));
#36745=CARTESIAN_POINT('Ctrl Pts',(-0.14047439120071,0.150846613462089,
0.573291782711304));
#36746=CARTESIAN_POINT('Ctrl Pts',(-0.0784943311216198,0.190594846094957,
0.569588061028457));
#36747=CARTESIAN_POINT('Ctrl Pts',(-0.0139960769924853,0.195218999146749,
0.565884339345609));
#36748=CARTESIAN_POINT('Ctrl Pts',(0.0505021771366483,0.199843152198542,
0.562180617662761));
#36749=CARTESIAN_POINT('Ctrl Pts',(0.117518625315826,0.169343225669258,
0.558476895979913));
#36750=CARTESIAN_POINT('Ctrl Pts',(0.156396070392606,0.117671648942254,
0.554773174297065));
#36751=CARTESIAN_POINT('Ctrl Pts',(0.195273515469386,0.0660000722152496,
0.551069452614217));
#36752=CARTESIAN_POINT('Ctrl Pts',(0.206011957443768,-0.00684315470947738,
0.547365730931369));
#36753=CARTESIAN_POINT('Ctrl Pts',(0.183699012241942,-0.0675353292756691,
0.543662009248521));
#36754=CARTESIAN_POINT('Ctrl Pts',(0.161386067040115,-0.128227503841861,
0.539958287565673));
#36755=CARTESIAN_POINT('Ctrl Pts',(0.106021734662079,-0.176768626049519,
0.536254565882826));
#36756=CARTESIAN_POINT('Ctrl Pts',(0.0429328609649713,-0.190953180775813,
0.532550844199978));
#36757=CARTESIAN_POINT('Ctrl Pts',(-0.0201560127321352,-0.205137735502108,
0.52884712251713));
#36758=CARTESIAN_POINT('Ctrl Pts',(-0.0909694277483132,-0.184965722747041,
0.525143400834282));
#36759=CARTESIAN_POINT('Ctrl Pts',(-0.137113234823603,-0.139664987148696,
0.521439679151434));
#36760=CARTESIAN_POINT('Ctrl Pts',(-0.173877852911313,-0.103572077852157,
0.51848877583843));
#36761=CARTESIAN_POINT('Ctrl Pts',(-0.194982335358017,-0.0515275892214865,
0.515537872525427));
#36762=CARTESIAN_POINT('Ctrl Pts',(-0.195458266482996,0.000173443779922018,
0.512586969212423));
#36763=CARTESIAN_POINT('Ctrl Pts',(-0.195491180920002,0.000168629508682236,
0.502413030787576));
#36764=CARTESIAN_POINT('Ctrl Pts',(-0.195010205227512,-0.0526295513449078,
0.505427864266167));
#36765=CARTESIAN_POINT('Ctrl Pts',(-0.172879182329996,-0.105782955367232,
0.508442697744757));
#36766=CARTESIAN_POINT('Ctrl Pts',(-0.134689356786549,-0.142005289462677,
0.511457531223348));
#36767=CARTESIAN_POINT('Ctrl Pts',(-0.0877416010060499,-0.186534356320495,
0.51516374521772));
#36768=CARTESIAN_POINT('Ctrl Pts',(-0.0165250908911267,-0.205476460953673,
0.518869959212092));
#36769=CARTESIAN_POINT('Ctrl Pts',(0.0463414671012952,-0.190155708549211,
0.522576173206464));
#36770=CARTESIAN_POINT('Ctrl Pts',(0.109208025093718,-0.174834956144749,
0.526282387200837));
#36771=CARTESIAN_POINT('Ctrl Pts',(0.163724630963639,-0.125251346702646,
0.529988601195209));
#36772=CARTESIAN_POINT('Ctrl Pts',(0.184921496651671,-0.0641152489120857,
0.533694815189581));
#36773=CARTESIAN_POINT('Ctrl Pts',(0.206118362339704,-0.00297915112152539,
0.537401029183953));
#36774=CARTESIAN_POINT('Ctrl Pts',(0.193995487845847,0.0697094350174917,
0.541107243178325));
#36775=CARTESIAN_POINT('Ctrl Pts',(0.154105412656959,0.120657560296821,
0.544813457172697));
#36776=CARTESIAN_POINT('Ctrl Pts',(0.114215337468071,0.171605685576151,
0.548519671167069));
#36777=CARTESIAN_POINT('Ctrl Pts',(0.0465580615841514,0.200813349995792,
0.552225885161441));
#36778=CARTESIAN_POINT('Ctrl Pts',(-0.0178779150223708,0.194902809680635,
0.555932099155813));
#36779=CARTESIAN_POINT('Ctrl Pts',(-0.0823138916288934,0.188992269365477,
0.559638313150186));
#36780=CARTESIAN_POINT('Ctrl Pts',(-0.143528568958019,0.14796352431552,
0.563344527144558));
#36781=CARTESIAN_POINT('Ctrl Pts',(-0.173484296927877,0.0906086297567353,
0.56705074113893));
#36782=CARTESIAN_POINT('Ctrl Pts',(-0.187931321146693,0.0629475576708828,
0.568838171021812));
#36783=CARTESIAN_POINT('Ctrl Pts',(-0.195107725773013,0.031489133949035,
0.570625600904694));
#36784=CARTESIAN_POINT('Ctrl Pts',(-0.195080468396925,1.8981806121043E-5,
0.572413030787576));
#36785=CARTESIAN_POINT('Origin',(0.,0.,0.));
#36786=CARTESIAN_POINT('',(-0.195470932084261,-0.000171584046685047,0.652586969212424));
#36787=CARTESIAN_POINT('',(-0.195421427783755,-0.000177812761388513,0.642413030787576));
#36788=CARTESIAN_POINT('',(-0.1954,-2.39295984553393E-17,0.));
#36789=CARTESIAN_POINT('Ctrl Pts',(-0.195470932084261,-0.000171584046685047,
0.652586969212424));
#36790=CARTESIAN_POINT('Ctrl Pts',(-0.194992946923152,0.0519398730151351,
0.649612144370087));
#36791=CARTESIAN_POINT('Ctrl Pts',(-0.173506994162404,0.104399306729571,
0.64663731952775));
#36792=CARTESIAN_POINT('Ctrl Pts',(-0.136210733975536,0.140545308526766,
0.643662494685414));
#36793=CARTESIAN_POINT('Ctrl Pts',(-0.0897760782010601,0.185547867567989,
0.639958773002566));
#36794=CARTESIAN_POINT('Ctrl Pts',(-0.0188341937200331,0.205263315093338,
0.636255051319719));
#36795=CARTESIAN_POINT('Ctrl Pts',(0.0441620008484366,0.190672665791667,
0.632551329636871));
#36796=CARTESIAN_POINT('Ctrl Pts',(0.107158195416906,0.176082016489995,
0.628847607954023));
#36797=CARTESIAN_POINT('Ctrl Pts',(0.162208700072817,0.127185270361303,
0.625143886271175));
#36798=CARTESIAN_POINT('Ctrl Pts',(0.184130231899333,0.0663506254660481,
0.621440164588327));
#36799=CARTESIAN_POINT('Ctrl Pts',(0.20605176372585,0.00551598057079281,
0.617736442905479));
#36800=CARTESIAN_POINT('Ctrl Pts',(0.194844322722972,-0.0672565630910262,
0.614032721222632));
#36801=CARTESIAN_POINT('Ctrl Pts',(0.155634840229719,-0.118676637573315,
0.610328999539784));
#36802=CARTESIAN_POINT('Ctrl Pts',(0.116425357736466,-0.170096712055603,
0.606625277856936));
#36803=CARTESIAN_POINT('Ctrl Pts',(0.0492138337528384,-0.200164317358361,
0.602921556174087));
#36804=CARTESIAN_POINT('Ctrl Pts',(-0.0152532956197894,-0.195124792816734,
0.59921783449124));
#36805=CARTESIAN_POINT('Ctrl Pts',(-0.0797204249924167,-0.190085268275106,
0.595514112808392));
#36806=CARTESIAN_POINT('Ctrl Pts',(-0.141443159754043,-0.149938613889095,
0.591810391125544));
#36807=CARTESIAN_POINT('Ctrl Pts',(-0.172185953262212,-0.0930502299740384,
0.588106669442696));
#36808=CARTESIAN_POINT('Ctrl Pts',(-0.187458069522289,-0.0647897528391999,
0.586266769365939));
#36809=CARTESIAN_POINT('Ctrl Pts',(-0.195084923717034,-0.0323977343102287,
0.584426869289181));
#36810=CARTESIAN_POINT('Ctrl Pts',(-0.195079815420139,-3.45302974047446E-6,
0.582586969212423));
#36811=CARTESIAN_POINT('Ctrl Pts',(-0.195080468396925,1.8981806121043E-5,
0.572413030787576));
#36812=CARTESIAN_POINT('Ctrl Pts',(-0.195051207937167,-0.0337638415069996,
0.574331814899066));
#36813=CARTESIAN_POINT('Ctrl Pts',(-0.186720620393942,-0.0675601803708791,
0.576250599010555));
#36814=CARTESIAN_POINT('Ctrl Pts',(-0.170171536425399,-0.0966869859783203,
0.578169383122045));
#36815=CARTESIAN_POINT('Ctrl Pts',(-0.138206269342473,-0.15294666308698,
0.581875597116418));
#36816=CARTESIAN_POINT('Ctrl Pts',(-0.0755789565660301,-0.191784973236686,
0.585581811110791));
#36817=CARTESIAN_POINT('Ctrl Pts',(-0.0109742658556152,-0.195413127900566,
0.589288025105163));
#36818=CARTESIAN_POINT('Ctrl Pts',(0.0536304248547996,-0.199041282564447,
0.592994239099535));
#36819=CARTESIAN_POINT('Ctrl Pts',(0.120212493499187,-0.1674592817425,0.596700453093906));
#36820=CARTESIAN_POINT('Ctrl Pts',(0.158275908344154,-0.115132366886058,
0.600406667088278));
#36821=CARTESIAN_POINT('Ctrl Pts',(0.19633932318912,-0.0628054520296152,
0.60411288108265));
#36822=CARTESIAN_POINT('Ctrl Pts',(0.205884084234667,0.0102663768613233,
0.607819095077022));
#36823=CARTESIAN_POINT('Ctrl Pts',(0.182538483877546,0.0706146370849535,
0.611525309071394));
#36824=CARTESIAN_POINT('Ctrl Pts',(0.159192883520425,0.130962897308584,
0.615231523065767));
#36825=CARTESIAN_POINT('Ctrl Pts',(0.102956921760636,0.178587588864905,
0.618937737060139));
#36826=CARTESIAN_POINT('Ctrl Pts',(0.0395878889512919,0.191675569949154,
0.622643951054511));
#36827=CARTESIAN_POINT('Ctrl Pts',(-0.0237811438580523,0.204763551033402,
0.626350165048883));
#36828=CARTESIAN_POINT('Ctrl Pts',(-0.0942832477169518,0.183314821645578,
0.630056379043255));
#36829=CARTESIAN_POINT('Ctrl Pts',(-0.139626929730598,0.137153365109863,
0.633762593037627));
#36830=CARTESIAN_POINT('Ctrl Pts',(-0.17490486198241,0.101239194403086,
0.63664607228761));
#36831=CARTESIAN_POINT('Ctrl Pts',(-0.194954331224527,0.0503663409317413,
0.639529551537593));
#36832=CARTESIAN_POINT('Ctrl Pts',(-0.195421427783755,-0.000177812761388513,
0.642413030787576));
#36833=CARTESIAN_POINT('Origin',(0.,0.,0.));
#36834=CARTESIAN_POINT('',(-0.195636369417486,0.000113518110994186,0.722586969212423));
#36835=CARTESIAN_POINT('',(-0.195675615924934,8.51174274233985E-5,0.712413030787576));
#36836=CARTESIAN_POINT('',(-0.1954,-2.39295984553393E-17,0.));
#36837=CARTESIAN_POINT('Ctrl Pts',(-0.195636369417486,0.000113518110994186,
0.722586969212423));
#36838=CARTESIAN_POINT('Ctrl Pts',(-0.195682546989371,0.00679235189129894,
0.722204862816689));
#36839=CARTESIAN_POINT('Ctrl Pts',(-0.195370156992351,0.0134668159558925,
0.721822756420955));
#36840=CARTESIAN_POINT('Ctrl Pts',(-0.194684940168549,0.0201027826582277,
0.72144065002522));
#36841=CARTESIAN_POINT('Ctrl Pts',(-0.188043197355288,0.0844245894546327,
0.717736928342373));
#36842=CARTESIAN_POINT('Ctrl Pts',(-0.146373463610807,0.145129475044757,
0.714033206659525));
#36843=CARTESIAN_POINT('Ctrl Pts',(-0.0887378837876281,0.174447515831938,
0.710329484976677));
#36844=CARTESIAN_POINT('Ctrl Pts',(-0.031102303964449,0.203765556619118,
0.706625763293829));
#36845=CARTESIAN_POINT('Ctrl Pts',(0.0424991219374283,0.201696752603353,
0.702922041610981));
#36846=CARTESIAN_POINT('Ctrl Pts',(0.0983968473233738,0.169187494324663,
0.699218319928133));
#36847=CARTESIAN_POINT('Ctrl Pts',(0.154294572709319,0.136678236045973,
0.695514598245285));
#36848=CARTESIAN_POINT('Ctrl Pts',(0.192488597579333,0.0737285235043576,
0.691810876562437));
#36849=CARTESIAN_POINT('Ctrl Pts',(0.195506767226643,0.00913519390189264,
0.68810715487959));
#36850=CARTESIAN_POINT('Ctrl Pts',(0.198524936873952,-0.0554581357005719,
0.684403433196742));
#36851=CARTESIAN_POINT('Ctrl Pts',(0.166367251298559,-0.121695082363886,
0.680699711513894));
#36852=CARTESIAN_POINT('Ctrl Pts',(0.113744494695038,-0.159275037986524,
0.676995989831046));
#36853=CARTESIAN_POINT('Ctrl Pts',(0.0611217380915185,-0.196854993609162,
0.673292268148198));
#36854=CARTESIAN_POINT('Ctrl Pts',(-0.0119660895401274,-0.205777958191125,
0.669588546465349));
#36855=CARTESIAN_POINT('Ctrl Pts',(-0.072084391141631,-0.181962051958034,
0.665884824782502));
#36856=CARTESIAN_POINT('Ctrl Pts',(-0.132202692743136,-0.158146145724943,
0.662181103099654));
#36857=CARTESIAN_POINT('Ctrl Pts',(-0.179351468314497,-0.101591368676797,
0.658477381416807));
#36858=CARTESIAN_POINT('Ctrl Pts',(-0.191962142566216,-0.0381691448741754,
0.654773659733959));
#36859=CARTESIAN_POINT('Ctrl Pts',(-0.19444393828574,-0.0256875756563692,
0.654044762893447));
#36860=CARTESIAN_POINT('Ctrl Pts',(-0.195588048853217,-0.0129400253566584,
0.653315866052935));
#36861=CARTESIAN_POINT('Ctrl Pts',(-0.195470932084261,-0.000171584046685047,
0.652586969212424));
#36862=CARTESIAN_POINT('Ctrl Pts',(-0.195421427783755,-0.000177812761388513,
0.642413030787576));
#36863=CARTESIAN_POINT('Ctrl Pts',(-0.195554703085897,-0.0145994290672205,
0.643235765531965));
#36864=CARTESIAN_POINT('Ctrl Pts',(-0.194093747105224,-0.0289942854151266,
0.644058500276354));
#36865=CARTESIAN_POINT('Ctrl Pts',(-0.190937423221194,-0.0430072724152966,
0.644881235020743));
#36866=CARTESIAN_POINT('Ctrl Pts',(-0.17671897452975,-0.106132269721135,
0.648587449015115));
#36867=CARTESIAN_POINT('Ctrl Pts',(-0.128096816978468,-0.161508080649208,
0.652293663009487));
#36868=CARTESIAN_POINT('Ctrl Pts',(-0.067340953434779,-0.183771382585667,
0.65599987700386));
#36869=CARTESIAN_POINT('Ctrl Pts',(-0.00658508989108841,-0.206034684522128,
0.659706090998232));
#36870=CARTESIAN_POINT('Ctrl Pts',(0.06630447964501,-0.195185477466974,
0.663412304992604));
#36871=CARTESIAN_POINT('Ctrl Pts',(0.117942751209788,-0.156192933591821,
0.667118518986976));
#36872=CARTESIAN_POINT('Ctrl Pts',(0.169581022774564,-0.117200389716668,
0.670824732981348));
#36873=CARTESIAN_POINT('Ctrl Pts',(0.19996799636802,-0.0500645090215166,
0.67453094697572));
#36874=CARTESIAN_POINT('Ctrl Pts',(0.195185778931935,0.0144650188277344,
0.678237160970092));
#36875=CARTESIAN_POINT('Ctrl Pts',(0.190403561495849,0.0789945466769872,
0.681943374964464));
#36876=CARTESIAN_POINT('Ctrl Pts',(0.15045215303022,0.14091772168034,0.685649588958836));
#36877=CARTESIAN_POINT('Ctrl Pts',(0.0936301652358751,0.171872386452436,
0.689355802953208));
#36878=CARTESIAN_POINT('Ctrl Pts',(0.0368081774415317,0.202827051224532,
0.69306201694758));
#36879=CARTESIAN_POINT('Ctrl Pts',(-0.0368843896815252,0.202813205765373,
0.696768230941953));
#36880=CARTESIAN_POINT('Ctrl Pts',(-0.0936947418561655,0.171837191595589,
0.700474444936325));
#36881=CARTESIAN_POINT('Ctrl Pts',(-0.150505094030807,0.140861177425805,
0.704180658930697));
#36882=CARTESIAN_POINT('Ctrl Pts',(-0.190433231257031,0.078922994545395,
0.707886872925069));
#36883=CARTESIAN_POINT('Ctrl Pts',(-0.195191200566454,0.0143916742729559,
0.711593086919441));
#36884=CARTESIAN_POINT('Ctrl Pts',(-0.195542076848464,0.00963281429343837,
0.711866401542153));
#36885=CARTESIAN_POINT('Ctrl Pts',(-0.195701686505733,0.00485985200318871,
0.712139716164864));
#36886=CARTESIAN_POINT('Ctrl Pts',(-0.195675615924934,8.51174274233985E-5,
0.712413030787576));
#36887=CARTESIAN_POINT('Origin',(0.,0.,0.));
#36888=CARTESIAN_POINT('',(-0.195128545551857,9.80157954364874E-5,0.792586969212424));
#36889=CARTESIAN_POINT('',(-0.195166123101285,0.000126544742759004,0.782413030787576));
#36890=CARTESIAN_POINT('',(-0.1954,-2.39295984553393E-17,0.));
#36891=CARTESIAN_POINT('Ctrl Pts',(-0.195128545551857,9.80157954364874E-5,
0.792586969212424));
#36892=CARTESIAN_POINT('Ctrl Pts',(-0.195247914943593,0.0263701155015296,
0.791093859580443));
#36893=CARTESIAN_POINT('Ctrl Pts',(-0.190313505751618,0.0525992349613935,
0.789600749948463));
#36894=CARTESIAN_POINT('Ctrl Pts',(-0.180112460177197,0.0765888339627252,
0.788107640316483));
#36895=CARTESIAN_POINT('Ctrl Pts',(-0.154808334564134,0.136096050365993,
0.784403918633635));
#36896=CARTESIAN_POINT('Ctrl Pts',(-0.0970981193167941,0.181823294990903,
0.780700196950786));
#36897=CARTESIAN_POINT('Ctrl Pts',(-0.0333818027149729,0.192852282969788,
0.776996475267938));
#36898=CARTESIAN_POINT('Ctrl Pts',(0.0303345138868501,0.203881270948674,
0.773292753585091));
#36899=CARTESIAN_POINT('Ctrl Pts',(0.100056931843154,0.180212002281536,
0.769589031902244));
#36900=CARTESIAN_POINT('Ctrl Pts',(0.143890387011628,0.132672168613705,
0.765885310219396));
#36901=CARTESIAN_POINT('Ctrl Pts',(0.187723842180101,0.0851323349458752,
0.762181588536548));
#36902=CARTESIAN_POINT('Ctrl Pts',(0.205668334560742,0.013721936277351,
0.758477866853699));
#36903=CARTESIAN_POINT('Ctrl Pts',(0.18951501609247,-0.0488917833023672,
0.754774145170851));
#36904=CARTESIAN_POINT('Ctrl Pts',(0.173361697624198,-0.111505502882086,
0.751070423488003));
#36905=CARTESIAN_POINT('Ctrl Pts',(0.123110568307013,-0.165322543373001,
0.747366701805156));
#36906=CARTESIAN_POINT('Ctrl Pts',(0.061749399359133,-0.185723879665063,
0.743662980122308));
#36907=CARTESIAN_POINT('Ctrl Pts',(0.000388230411252383,-0.206125215957126,
0.73995925843946));
#36908=CARTESIAN_POINT('Ctrl Pts',(-0.072082978167322,-0.193110848050335,
0.736255536756612));
#36909=CARTESIAN_POINT('Ctrl Pts',(-0.122511706515588,-0.152634300095596,
0.732551815073764));
#36910=CARTESIAN_POINT('Ctrl Pts',(-0.16773779241913,-0.116333645789233,
0.72923019978665));
#36911=CARTESIAN_POINT('Ctrl Pts',(-0.195234952088687,-0.0579449614967985,
0.725908584499537));
#36912=CARTESIAN_POINT('Ctrl Pts',(-0.195636369417486,0.000113518110994186,
0.722586969212423));
#36913=CARTESIAN_POINT('Ctrl Pts',(-0.195675615924934,8.51174274233985E-5,
0.712413030787576));
#36914=CARTESIAN_POINT('Ctrl Pts',(-0.195348162971424,-0.0598867317271105,
0.715845930159236));
#36915=CARTESIAN_POINT('Ctrl Pts',(-0.165727828481393,-0.120138176331325,
0.719278829530897));
#36916=CARTESIAN_POINT('Ctrl Pts',(-0.117884051406102,-0.156237241050387,
0.722711728902558));
#36917=CARTESIAN_POINT('Ctrl Pts',(-0.0662311315437018,-0.195210378436822,
0.72641794289693));
#36918=CARTESIAN_POINT('Ctrl Pts',(0.00666250957372189,-0.206032195545224,
0.730124156891302));
#36919=CARTESIAN_POINT('Ctrl Pts',(0.0674100031098693,-0.183746065393738,
0.733830370885674));
#36920=CARTESIAN_POINT('Ctrl Pts',(0.128157496646017,-0.161459935242253,
0.737536584880046));
#36921=CARTESIAN_POINT('Ctrl Pts',(0.176758842600887,-0.10606585783088,
0.741242798874417));
#36922=CARTESIAN_POINT('Ctrl Pts',(0.19095357026966,-0.0429355222190436,
0.744949012868789));
#36923=CARTESIAN_POINT('Ctrl Pts',(0.205148297938434,0.0201948133927931,
0.748655226863161));
#36924=CARTESIAN_POINT('Ctrl Pts',(0.184936407321109,0.0910614072050953,
0.752361440857534));
#36925=CARTESIAN_POINT('Ctrl Pts',(0.139575382755531,0.137205822017881,
0.756067654851907));
#36926=CARTESIAN_POINT('Ctrl Pts',(0.0942143581899539,0.183350236830666,
0.759773868846279));
#36927=CARTESIAN_POINT('Ctrl Pts',(0.0237041996761252,0.204772472643938,
0.76348008284065));
#36928=CARTESIAN_POINT('Ctrl Pts',(-0.0396599106844383,0.191660680765389,
0.767186296835022));
#36929=CARTESIAN_POINT('Ctrl Pts',(-0.103024021045003,0.178548888886839,
0.770892510829394));
#36930=CARTESIAN_POINT('Ctrl Pts',(-0.159242083252301,0.130903069316467,
0.774598724823766));
#36931=CARTESIAN_POINT('Ctrl Pts',(-0.182565005336597,0.0705460409477194,
0.778304938818139));
#36932=CARTESIAN_POINT('Ctrl Pts',(-0.19118230851659,0.0482454556858425,
0.779674302807951));
#36933=CARTESIAN_POINT('Ctrl Pts',(-0.195308968355645,0.0242096139413284,
0.781043666797764));
#36934=CARTESIAN_POINT('Ctrl Pts',(-0.195166123101285,0.000126544742759004,
0.782413030787576));
#36935=CARTESIAN_POINT('Origin',(0.,0.,0.));
#36936=CARTESIAN_POINT('',(-0.195279013340439,-0.000168009551267251,0.862586969212423));
#36937=CARTESIAN_POINT('',(-0.195215444869335,-0.000150235120299324,0.852413030787576));
#36938=CARTESIAN_POINT('',(-0.1954,-2.39295984553393E-17,0.));
#36939=CARTESIAN_POINT('Ctrl Pts',(-0.195279013340439,-0.000168009551267251,
0.862586969212423));
#36940=CARTESIAN_POINT('Ctrl Pts',(-0.194903607268958,0.0455640131522026,
0.859982856344197));
#36941=CARTESIAN_POINT('Ctrl Pts',(-0.178871895344458,0.0915331173731693,
0.857378743475971));
#36942=CARTESIAN_POINT('Ctrl Pts',(-0.149539281844263,0.126270942713959,
0.854774630607745));
#36943=CARTESIAN_POINT('Ctrl Pts',(-0.107820722729247,0.175677110357261,
0.851070908924897));
#36944=CARTESIAN_POINT('Ctrl Pts',(-0.0391968436807465,0.202364430724413,
0.847367187242049));
#36945=CARTESIAN_POINT('Ctrl Pts',(0.024939826400162,0.194124580780539,
0.843663465559201));
#36946=CARTESIAN_POINT('Ctrl Pts',(0.0890764964810705,0.185884730836666,
0.839959743876352));
#36947=CARTESIAN_POINT('Ctrl Pts',(0.148725957594388,0.142717710581768,
0.836256022193505));
#36948=CARTESIAN_POINT('Ctrl Pts',(0.176601098282085,0.0843706103134459,
0.832552300510657));
#36949=CARTESIAN_POINT('Ctrl Pts',(0.204476238969783,0.0260235100451228,
0.828848578827809));
#36950=CARTESIAN_POINT('Ctrl Pts',(0.200577059231861,-0.0475036702366233,
0.825144857144961));
#36951=CARTESIAN_POINT('Ctrl Pts',(0.166687269277466,-0.102575348200379,
0.821441135462114));
#36952=CARTESIAN_POINT('Ctrl Pts',(0.132797479323072,-0.157647026164133,
0.817737413779266));
#36953=CARTESIAN_POINT('Ctrl Pts',(0.0689170791522051,-0.194263201809897,
0.814033692096418));
#36954=CARTESIAN_POINT('Ctrl Pts',(0.00426865627857745,-0.195673519857469,
0.81032997041357));
#36955=CARTESIAN_POINT('Ctrl Pts',(-0.060379766595052,-0.197083837905041,
0.806626248730722));
#36956=CARTESIAN_POINT('Ctrl Pts',(-0.125796212171444,-0.16328829835442,
0.802922527047874));
#36957=CARTESIAN_POINT('Ctrl Pts',(-0.162055416970245,-0.109746934488294,
0.799218805365026));
#36958=CARTESIAN_POINT('Ctrl Pts',(-0.183697171385623,-0.0777901098892797,
0.797008193314158));
#36959=CARTESIAN_POINT('Ctrl Pts',(-0.194951814111497,-0.0387989405753114,
0.794797581263291));
#36960=CARTESIAN_POINT('Ctrl Pts',(-0.195128545551857,9.80157954364874E-5,
0.792586969212424));
#36961=CARTESIAN_POINT('Ctrl Pts',(-0.195166123101285,0.000126544742759004,
0.782413030787576));
#36962=CARTESIAN_POINT('Ctrl Pts',(-0.194922354508138,-0.0409717467160323,
0.784749880792136));
#36963=CARTESIAN_POINT('Ctrl Pts',(-0.182244856716882,-0.0822075748123473,
0.787086730796695));
#36964=CARTESIAN_POINT('Ctrl Pts',(-0.158232634722073,-0.115191832939155,
0.789423580801255));
#36965=CARTESIAN_POINT('Ctrl Pts',(-0.120149560061961,-0.167504441290151,
0.793129794795627));
#36966=CARTESIAN_POINT('Ctrl Pts',(-0.0535556287804454,-0.199061420825021,
0.796836008789999));
#36967=CARTESIAN_POINT('Ctrl Pts',(0.0110476940437387,-0.195408990384897,
0.800542222784371));
#36968=CARTESIAN_POINT('Ctrl Pts',(0.0756510168679237,-0.191756559944773,
0.804248436778743));
#36969=CARTESIAN_POINT('Ctrl Pts',(0.138263731234777,-0.152894719529654,
0.807954650773115));
#36970=CARTESIAN_POINT('Ctrl Pts',(0.170207855773424,-0.0966230350379699,
0.811660864767488));
#36971=CARTESIAN_POINT('Ctrl Pts',(0.202151980312072,-0.0403513505462853,
0.81536707876186));
#36972=CARTESIAN_POINT('Ctrl Pts',(0.203427515022513,0.0333301780219651,
0.819073292756232));
#36973=CARTESIAN_POINT('Ctrl Pts',(0.173450237337761,0.0906738122863988,
0.822779506750604));
#36974=CARTESIAN_POINT('Ctrl Pts',(0.143472959653009,0.148017446550833,
0.826485720744976));
#36975=CARTESIAN_POINT('Ctrl Pts',(0.0822428695730641,0.189023186511451,
0.830191934739348));
#36976=CARTESIAN_POINT('Ctrl Pts',(0.0178046765554912,0.194909513773745,
0.83389814873372));
#36977=CARTESIAN_POINT('Ctrl Pts',(-0.0466335164620799,0.200795841036038,
0.837604362728092));
#36978=CARTESIAN_POINT('Ctrl Pts',(-0.114279812417278,0.171562755600011,
0.841310576722464));
#36979=CARTESIAN_POINT('Ctrl Pts',(-0.154150740386038,0.120599644714809,
0.845016790716836));
#36980=CARTESIAN_POINT('Ctrl Pts',(-0.180673309918174,0.0866984359672774,
0.84748220407375));
#36981=CARTESIAN_POINT('Ctrl Pts',(-0.194905131081074,0.0431815751432988,
0.849947617430663));
#36982=CARTESIAN_POINT('Ctrl Pts',(-0.195215444869335,-0.000150235120299324,
0.852413030787576));
#36983=CARTESIAN_POINT('Origin',(0.,0.,0.));
#36984=CARTESIAN_POINT('',(-0.195719986784682,3.71606954582295E-6,0.932586969212424));
#36985=CARTESIAN_POINT('',(-0.195707453392556,-4.66568259871601E-5,0.922413030787576));
#36986=CARTESIAN_POINT('',(-0.1954,-2.39295984553393E-17,0.));
#36987=CARTESIAN_POINT('Ctrl Pts',(-0.195719986784682,3.71606954582295E-6,
0.932586969212424));
#36988=CARTESIAN_POINT('Ctrl Pts',(-0.195738156138108,0.0648665395087412,
0.928871853107952));
#36989=CARTESIAN_POINT('Ctrl Pts',(-0.160275715576186,0.129712057687137,
0.925156737003479));
#36990=CARTESIAN_POINT('Ctrl Pts',(-0.10568144211536,0.164735485073218,
0.921441620899007));
#36991=CARTESIAN_POINT('Ctrl Pts',(-0.0512546116502832,0.199651494094127,
0.917737899216159));
#36992=CARTESIAN_POINT('Ctrl Pts',(0.0221865722997436,0.204928064005996,
0.914034177533311));
#36993=CARTESIAN_POINT('Ctrl Pts',(0.0810458692323854,0.178151382429043,
0.910330455850463));
#36994=CARTESIAN_POINT('Ctrl Pts',(0.139905166165026,0.151374700852089,
0.906626734167615));
#36995=CARTESIAN_POINT('Ctrl Pts',(0.184182576080283,0.0925447677863139,
0.902923012484767));
#36996=CARTESIAN_POINT('Ctrl Pts',(0.193623051178265,0.0285737974246437,
0.899219290801919));
#36997=CARTESIAN_POINT('Ctrl Pts',(0.203063526276248,-0.0353971729370283,
0.895515569119071));
#36998=CARTESIAN_POINT('Ctrl Pts',(0.177667066556955,-0.104509180594595,
0.891811847436224));
#36999=CARTESIAN_POINT('Ctrl Pts',(0.129051481285208,-0.147146399547075,
0.888108125753376));
#37000=CARTESIAN_POINT('Ctrl Pts',(0.0804358960134615,-0.189783618499555,
0.884404404070528));
#37001=CARTESIAN_POINT('Ctrl Pts',(0.00860118518926115,-0.205946048746948,
0.88070068238768));
#37002=CARTESIAN_POINT('Ctrl Pts',(-0.0535913025040727,-0.188240059832962,
0.876996960704832));
#37003=CARTESIAN_POINT('Ctrl Pts',(-0.115783790197406,-0.170534070918976,
0.873293239021984));
#37004=CARTESIAN_POINT('Ctrl Pts',(-0.168334054759872,-0.118959662843613,
0.869589517339136));
#37005=CARTESIAN_POINT('Ctrl Pts',(-0.187202567450341,-0.0571099513462054,
0.865885795656288));
#37006=CARTESIAN_POINT('Ctrl Pts',(-0.192804495632289,-0.0387472087407564,
0.864786186841667));
#37007=CARTESIAN_POINT('Ctrl Pts',(-0.195437531748109,-0.0194787452297348,
0.863686578027045));
#37008=CARTESIAN_POINT('Ctrl Pts',(-0.195279013340439,-0.000168009551267251,
0.862586969212423));
#37009=CARTESIAN_POINT('Ctrl Pts',(-0.195215444869335,-0.000150235120299324,
0.852413030787576));
#37010=CARTESIAN_POINT('Ctrl Pts',(-0.195371620524508,-0.021958398707372,
0.853653831425035));
#37011=CARTESIAN_POINT('Ctrl Pts',(-0.192001564940553,-0.0437196901383431,
0.854894632062494));
#37012=CARTESIAN_POINT('Ctrl Pts',(-0.184897391479539,-0.0641847309864828,
0.856135432699953));
#37013=CARTESIAN_POINT('Ctrl Pts',(-0.163677554621959,-0.125312859468192,
0.859841646694325));
#37014=CARTESIAN_POINT('Ctrl Pts',(-0.10914232092448,-0.174875980097234,
0.863547860688697));
#37015=CARTESIAN_POINT('Ctrl Pts',(-0.0462700104058479,-0.190173108515756,
0.867254074683069));
#37016=CARTESIAN_POINT('Ctrl Pts',(0.0166023001127845,-0.205470236934278,
0.870960288677441));
#37017=CARTESIAN_POINT('Ctrl Pts',(0.0878116874525705,-0.186501373142281,
0.874666502671813));
#37018=CARTESIAN_POINT('Ctrl Pts',(0.134742707561642,-0.141954668207959,
0.878372716666185));
#37019=CARTESIAN_POINT('Ctrl Pts',(0.181673727670714,-0.0974079632736377,
0.882078930660557));
#37020=CARTESIAN_POINT('Ctrl Pts',(0.204326380549072,-0.0272834171969915,
0.885785144654929));
#37021=CARTESIAN_POINT('Ctrl Pts',(0.192325259761237,0.0363004067433246,
0.889491358649301));
#37022=CARTESIAN_POINT('Ctrl Pts',(0.180324138973402,0.0998842306836407,
0.893197572643673));
#37023=CARTESIAN_POINT('Ctrl Pts',(0.133669244519374,0.156927332487627,
0.896903786638045));
#37024=CARTESIAN_POINT('Ctrl Pts',(0.0737295301650971,0.181302734225987,
0.900610000632418));
#37025=CARTESIAN_POINT('Ctrl Pts',(0.0137898158108199,0.205678135964346,
0.90431621462679));
#37026=CARTESIAN_POINT('Ctrl Pts',(-0.059434718443707,0.19738583763708,
0.908022428621162));
#37027=CARTESIAN_POINT('Ctrl Pts',(-0.112405647662483,0.160223891616111,
0.911728642615534));
#37028=CARTESIAN_POINT('Ctrl Pts',(-0.163307724594775,0.124513356361944,
0.915290105339548));
#37029=CARTESIAN_POINT('Ctrl Pts',(-0.195507366281261,0.0621442230158499,
0.918851568063562));
#37030=CARTESIAN_POINT('Ctrl Pts',(-0.195707453392556,-4.66568259871601E-5,
0.922413030787576));
#37031=CARTESIAN_POINT('Origin',(0.,0.,0.));
#37032=CARTESIAN_POINT('',(-0.195268202714777,0.000165579016441021,1.00258696921242));
#37033=CARTESIAN_POINT('',(-0.19535343393295,0.000178280253715055,0.992413030787576));
#37034=CARTESIAN_POINT('',(-0.1954,-2.39295984553393E-17,0.));
#37035=CARTESIAN_POINT('Ctrl Pts',(-0.195268202714777,0.000165579016441021,
1.00258696921242));
#37036=CARTESIAN_POINT('Ctrl Pts',(-0.19542709496717,0.0198793394721131,
1.00146457155455));
#37037=CARTESIAN_POINT('Ctrl Pts',(-0.192681564478375,0.0395498739780043,
1.00034217389668));
#37038=CARTESIAN_POINT('Ctrl Pts',(-0.186848643290836,0.0582577638715851,
0.999219776238813));
#37039=CARTESIAN_POINT('Ctrl Pts',(-0.167600993827966,0.11999062383733,
0.995516054555966));
#37040=CARTESIAN_POINT('Ctrl Pts',(-0.114735119634562,0.171241362792136,
0.991812332873117));
#37041=CARTESIAN_POINT('Ctrl Pts',(-0.0524351231736321,0.18856531990772,
0.988108611190269));
#37042=CARTESIAN_POINT('Ctrl Pts',(0.00986487328729629,0.205889277023303,
0.984404889507421));
#37043=CARTESIAN_POINT('Ctrl Pts',(0.0815989920157509,0.189286452299667,
0.980701167824573));
#37044=CARTESIAN_POINT('Ctrl Pts',(0.129952003507049,0.146351732792493,
0.976997446141725));
#37045=CARTESIAN_POINT('Ctrl Pts',(0.178305014998348,0.103417013285319,
0.973293724458878));
#37046=CARTESIAN_POINT('Ctrl Pts',(0.20327691925249,0.0341503989946047,
0.969590002776029));
#37047=CARTESIAN_POINT('Ctrl Pts',(0.19344406978275,-0.0297614493697593,
0.965886281093181));
#37048=CARTESIAN_POINT('Ctrl Pts',(0.18361122031301,-0.0936732977341234,
0.962182559410334));
#37049=CARTESIAN_POINT('Ctrl Pts',(0.138973617119388,-0.152230380172138,
0.958478837727486));
#37050=CARTESIAN_POINT('Ctrl Pts',(0.0799511084736072,-0.178645358874384,
0.954775116044638));
#37051=CARTESIAN_POINT('Ctrl Pts',(0.0209285998278261,-0.20506033757663,
0.95107139436179));
#37052=CARTESIAN_POINT('Ctrl Pts',(-0.0524788142701144,-0.199333212543108,
0.947367672678942));
#37053=CARTESIAN_POINT('Ctrl Pts',(-0.106690354347858,-0.16408387214268,
0.943663950996094));
#37054=CARTESIAN_POINT('Ctrl Pts',(-0.160735113766186,-0.128942975594381,
0.93997162373487));
#37055=CARTESIAN_POINT('Ctrl Pts',(-0.195701928883641,-0.0644612332051665,
0.936279296473647));
#37056=CARTESIAN_POINT('Ctrl Pts',(-0.195719986784682,3.71606954582295E-6,
0.932586969212424));
#37057=CARTESIAN_POINT('Ctrl Pts',(-0.195707453392556,-4.66568259871601E-5,
0.922413030787576));
#37058=CARTESIAN_POINT('Ctrl Pts',(-0.195715585687005,-0.00257432861687418,
0.922557782057934));
#37059=CARTESIAN_POINT('Ctrl Pts',(-0.195670857405051,-0.00510170594794435,
0.922702533328292));
#37060=CARTESIAN_POINT('Ctrl Pts',(-0.195572375776859,-0.00762698699047084,
0.92284728459865));
#37061=CARTESIAN_POINT('Ctrl Pts',(-0.193050850489432,-0.0722843258614067,
0.926553498593022));
#37062=CARTESIAN_POINT('Ctrl Pts',(-0.155290475731554,-0.135567409888606,
0.930259712587394));
#37063=CARTESIAN_POINT('Ctrl Pts',(-0.0995863227266852,-0.168491214354887,
0.933965926581766));
#37064=CARTESIAN_POINT('Ctrl Pts',(-0.0438821697218168,-0.201415018821168,
0.937672140576139));
#37065=CARTESIAN_POINT('Ctrl Pts',(0.0297657615300397,-0.203979543726533,
0.94137835457051));
#37066=CARTESIAN_POINT('Ctrl Pts',(0.0876251218790847,-0.175010180082627,
0.945084568564882));
#37067=CARTESIAN_POINT('Ctrl Pts',(0.145484482228131,-0.146040816438721,
0.948790782559255));
#37068=CARTESIAN_POINT('Ctrl Pts',(0.187555271674363,-0.0855375642455424,
0.952496996553627));
#37069=CARTESIAN_POINT('Ctrl Pts',(0.194568154283725,-0.021212227253196,
0.956203210547999));
#37070=CARTESIAN_POINT('Ctrl Pts',(0.201581036893087,0.0431131097391505,
0.959909424542371));
#37071=CARTESIAN_POINT('Ctrl Pts',(0.173536012665579,0.111260531530666,
0.963615638536743));
#37072=CARTESIAN_POINT('Ctrl Pts',(0.123278314419194,0.152017044141902,
0.967321852531115));
#37073=CARTESIAN_POINT('Ctrl Pts',(0.0730206161728088,0.192773556753138,
0.971028066525487));
#37074=CARTESIAN_POINT('Ctrl Pts',(0.000550243907548716,0.206139160184095,
0.974734280519859));
#37075=CARTESIAN_POINT('Ctrl Pts',(-0.0609398062732146,0.185992111567971,
0.978440494514231));
#37076=CARTESIAN_POINT('Ctrl Pts',(-0.122429856453979,0.165845062951848,
0.982146708508603));
#37077=CARTESIAN_POINT('Ctrl Pts',(-0.172939584550245,0.112185362288641,
0.985852922502976));
#37078=CARTESIAN_POINT('Ctrl Pts',(-0.189334427223443,0.0495903289718102,
0.989559136497348));
#37079=CARTESIAN_POINT('Ctrl Pts',(-0.193542598326109,0.0335236538822793,
0.990510434594091));
#37080=CARTESIAN_POINT('Ctrl Pts',(-0.195503184094814,0.0168682937546108,
0.991461732690834));
#37081=CARTESIAN_POINT('Ctrl Pts',(-0.19535343393295,0.000178280253715055,
0.992413030787576));
#37082=CARTESIAN_POINT('Origin',(0.,0.,0.));
#37083=CARTESIAN_POINT('',(-0.195129684289216,-0.000113636086278679,1.07258696921242));
#37084=CARTESIAN_POINT('',(-0.195093054978418,-5.50606481354719E-5,1.06241303078758));
#37085=CARTESIAN_POINT('',(-0.1954,-2.39295984553393E-17,0.));
#37086=CARTESIAN_POINT('Ctrl Pts',(-0.195129684289216,-0.000113636086278679,
1.07258696921242));
#37087=CARTESIAN_POINT('Ctrl Pts',(-0.194942963316978,0.0391854106201406,
1.07035356831831));
#37088=CARTESIAN_POINT('Ctrl Pts',(-0.183442754086643,0.0785903964976412,
1.06812016742419));
#37089=CARTESIAN_POINT('Ctrl Pts',(-0.161381630858742,0.110744756631717,
1.06588676653008));
#37090=CARTESIAN_POINT('Ctrl Pts',(-0.124796949325566,0.164067382739912,
1.06218304484723));
#37091=CARTESIAN_POINT('Ctrl Pts',(-0.0591690439027595,0.197450300329055,
1.05847932316438));
#37092=CARTESIAN_POINT('Ctrl Pts',(0.00547076636758263,0.195640786233593,
1.05477560148153));
#37093=CARTESIAN_POINT('Ctrl Pts',(0.0701105766379276,0.19383127213813,
1.05107187979868));
#37094=CARTESIAN_POINT('Ctrl Pts',(0.133762291755807,0.156829326358058,
1.04736815811584));
#37095=CARTESIAN_POINT('Ctrl Pts',(0.167312833478204,0.101552035674769,
1.04366443643299));
#37096=CARTESIAN_POINT('Ctrl Pts',(0.200863375200599,0.0462747449914819,
1.03996071475014));
#37097=CARTESIAN_POINT('Ctrl Pts',(0.204312743527515,-0.0272778905950186,
1.03625699306729));
#37098=CARTESIAN_POINT('Ctrl Pts',(0.17608042651717,-0.0854535269464722,
1.03255327138444));
#37099=CARTESIAN_POINT('Ctrl Pts',(0.147848109506825,-0.143629163297926,
1.0288495497016));
#37100=CARTESIAN_POINT('Ctrl Pts',(0.0879341071592168,-0.186427800414334,
1.02514582801875));
#37101=CARTESIAN_POINT('Ctrl Pts',(0.0237478981470821,-0.194273555725334,
1.0214421063359));
#37102=CARTESIAN_POINT('Ctrl Pts',(-0.0404383108650536,-0.202119311036335,
1.01773838465305));
#37103=CARTESIAN_POINT('Ctrl Pts',(-0.108896726541717,-0.175012184541928,
1.0140346629702));
#37104=CARTESIAN_POINT('Ctrl Pts',(-0.15031122201388,-0.125351130806383,
1.01033094128736));
#37105=CARTESIAN_POINT('Ctrl Pts',(-0.17917522457641,-0.0907396556226723,
1.00774961726238));
#37106=CARTESIAN_POINT('Ctrl Pts',(-0.194902777514884,-0.0451727225472274,
1.0051682932374));
#37107=CARTESIAN_POINT('Ctrl Pts',(-0.195268202714777,0.000165579016441021,
1.00258696921242));
#37108=CARTESIAN_POINT('Ctrl Pts',(-0.19535343393295,0.000178280253715055,
0.992413030787576));
#37109=CARTESIAN_POINT('Ctrl Pts',(-0.194919764294582,-0.0481552375812319,
0.995167946685205));
#37110=CARTESIAN_POINT('Ctrl Pts',(-0.176787653021499,-0.0967793777264111,
0.997922862582834));
#37111=CARTESIAN_POINT('Ctrl Pts',(-0.144290486192301,-0.132238333502052,
1.00067777848046));
#37112=CARTESIAN_POINT('Ctrl Pts',(-0.100571745237828,-0.179941596688631,
1.00438399247484));
#37113=CARTESIAN_POINT('Ctrl Pts',(-0.0308543060787511,-0.203817757091334,
1.00809020646921));
#37114=CARTESIAN_POINT('Ctrl Pts',(0.0329297761185238,-0.192930969998698,
1.01179642046358));
#37115=CARTESIAN_POINT('Ctrl Pts',(0.0967138583157977,-0.182044182906063,
1.01550263445795));
#37116=CARTESIAN_POINT('Ctrl Pts',(0.15456458355127,-0.136394448318089,
1.01920884845232));
#37117=CARTESIAN_POINT('Ctrl Pts',(0.179984980484802,-0.076890421197536,
1.0229150624467));
#37118=CARTESIAN_POINT('Ctrl Pts',(0.205405377418334,-0.0173863940769825,
1.02662127644107));
#37119=CARTESIAN_POINT('Ctrl Pts',(0.198395446049928,0.05597192557615,1.03032749043544));
#37120=CARTESIAN_POINT('Ctrl Pts',(0.162166047466929,0.109585000349956,
1.03403370442981));
#37121=CARTESIAN_POINT('Ctrl Pts',(0.12593664888393,0.163198075123761,1.03773991842419));
#37122=CARTESIAN_POINT('Ctrl Pts',(0.0604877830863377,0.19706590501824,
1.04144613241856));
#37123=CARTESIAN_POINT('Ctrl Pts',(-0.0042038551539475,0.195675976549601,
1.04515234641293));
#37124=CARTESIAN_POINT('Ctrl Pts',(-0.0688954933942345,0.194286048080962,
1.0488585604073));
#37125=CARTESIAN_POINT('Ctrl Pts',(-0.132829904077215,0.157638361249205,
1.05256477440167));
#37126=CARTESIAN_POINT('Ctrl Pts',(-0.166723158702796,0.102518946943711,
1.05627098839605));
#37127=CARTESIAN_POINT('Ctrl Pts',(-0.185446111291195,0.0720704641366568,
1.05831833585989));
#37128=CARTESIAN_POINT('Ctrl Pts',(-0.195001820365716,0.0359852200961074,
1.06036568332373));
#37129=CARTESIAN_POINT('Ctrl Pts',(-0.195093054978418,-5.50606481354719E-5,
1.06241303078758));
#37130=CARTESIAN_POINT('Origin',(0.,0.,-0.129405622560369));
#37131=CARTESIAN_POINT('',(-0.155334812646815,-9.04610707407963E-5,1.09559437743963));
#37132=CARTESIAN_POINT('',(-0.155659711405804,-0.000105088068675666,1.10940562256037));
#37133=CARTESIAN_POINT('',(-0.15555,-2.01987159101623E-14,-0.129405622560369));
#37134=CARTESIAN_POINT('',(0.0499806597877791,0.147301514408978,1.14445));
#37135=CARTESIAN_POINT('Ctrl Pts',(-0.155334812646815,-9.04610707408108E-5,
1.09559437743963));
#37136=CARTESIAN_POINT('Ctrl Pts',(-0.155432667860164,-0.0206859868644216,
1.09706469822836));
#37137=CARTESIAN_POINT('Ctrl Pts',(-0.142041322258558,-0.0930327919713715,
1.10223874069994));
#37138=CARTESIAN_POINT('Ctrl Pts',(-0.0324962964057439,-0.180887727526569,
1.11111650485437));
#37139=CARTESIAN_POINT('Ctrl Pts',(0.134445241673909,-0.125560970886474,
1.12222766990291));
#37140=CARTESIAN_POINT('Ctrl Pts',(0.178171768593789,0.0450698535437549,
1.13333883495146));
#37141=CARTESIAN_POINT('Ctrl Pts',(0.0989503531151977,0.130685679928735,
1.14074627831715));
#37142=CARTESIAN_POINT('Ctrl Pts',(0.0499806597877626,0.147301514408983,
1.14445));
#37143=CARTESIAN_POINT('',(0.155548765964692,0.000619602180124784,1.14445));
#37144=CARTESIAN_POINT('Origin',(0.,0.,1.14445));
#37145=CARTESIAN_POINT('Ctrl Pts',(-0.155659711405804,-0.00010508806867568,
1.10940562256037));
#37146=CARTESIAN_POINT('Ctrl Pts',(-0.155726922058417,-0.0079449137192624,
1.1099684397238));
#37147=CARTESIAN_POINT('Ctrl Pts',(-0.151630179095532,-0.0673453815214831,
1.1142374708816));
#37148=CARTESIAN_POINT('Ctrl Pts',(-0.075277483453787,-0.167898453189698,
1.12221271603377));
#37149=CARTESIAN_POINT('Ctrl Pts',(0.100462758039806,-0.153944373403644,
1.13333135801688));
#37150=CARTESIAN_POINT('Ctrl Pts',(0.155754888396286,-0.0511266487217653,
1.14074378600563));
#37151=CARTESIAN_POINT('Ctrl Pts',(0.155548765964692,0.000619602180124784,
1.14445));
#37152=CARTESIAN_POINT('Origin',(0.,0.,-0.129405622560369));
#37153=CARTESIAN_POINT('',(-0.155445081536763,0.000131810726739325,1.02559437743963));
#37154=CARTESIAN_POINT('',(-0.155305653540906,-4.38315446397164E-5,1.03940562256037));
#37155=CARTESIAN_POINT('',(-0.15555,-2.01987159101623E-14,-0.129405622560369));
#37156=CARTESIAN_POINT('Ctrl Pts',(-0.155445081536763,0.000131810726739319,
1.02559437743963));
#37157=CARTESIAN_POINT('Ctrl Pts',(-0.155154181384031,-0.0359601688445403,
1.02817570146461));
#37158=CARTESIAN_POINT('Ctrl Pts',(-0.124670140973274,-0.124280598265434,
1.03446074717243));
#37159=CARTESIAN_POINT('Ctrl Pts',(0.0223056668548975,-0.182477852394609,
1.04444951456311));
#37160=CARTESIAN_POINT('Ctrl Pts',(0.165390974917898,-0.0802670846854376,
1.05556067961165));
#37161=CARTESIAN_POINT('Ctrl Pts',(0.157153269033781,0.0953897085409752,
1.06667184466019));
#37162=CARTESIAN_POINT('Ctrl Pts',(0.00514163720288116,0.183756944970195,
1.07778300970874));
#37163=CARTESIAN_POINT('Ctrl Pts',(-0.130849536725084,0.114582374749785,
1.08742385396855));
#37164=CARTESIAN_POINT('Ctrl Pts',(-0.155186171668149,0.0311939131113674,
1.09336097654551));
#37165=CARTESIAN_POINT('Ctrl Pts',(-0.155334812646815,-9.04610707408108E-5,
1.09559437743963));
#37166=CARTESIAN_POINT('Ctrl Pts',(-0.155305653540906,-4.38315446397077E-5,
1.03940562256037));
#37167=CARTESIAN_POINT('Ctrl Pts',(-0.155364500629154,-0.0232901140548306,
1.0410644890909));
#37168=CARTESIAN_POINT('Ctrl Pts',(-0.139557528484751,-0.0983968830408974,
1.0464295696158));
#37169=CARTESIAN_POINT('Ctrl Pts',(-0.0231259578302998,-0.182421227428175,
1.05550086413507));
#37170=CARTESIAN_POINT('Ctrl Pts',(0.140774638007895,-0.11829694620695,
1.06661950611819));
#37171=CARTESIAN_POINT('Ctrl Pts',(0.175706993010233,0.0541796064983141,
1.07773814810131));
#37172=CARTESIAN_POINT('Ctrl Pts',(0.0497080432048737,0.177049779856472,
1.08885679008442));
#37173=CARTESIAN_POINT('Ctrl Pts',(-0.113185991314487,0.139680492671116,
1.09941261490411));
#37174=CARTESIAN_POINT('Ctrl Pts',(-0.155284332390808,0.0436812153822664,
1.10626222572943));
#37175=CARTESIAN_POINT('Ctrl Pts',(-0.155659711405804,-0.00010508806867568,
1.10940562256037));
#37176=CARTESIAN_POINT('Origin',(0.,0.,-0.129405622560369));
#37177=CARTESIAN_POINT('',(-0.155804728476752,2.95821195149996E-6,0.95559437743963));
#37178=CARTESIAN_POINT('',(-0.155512930646214,0.000141921665610299,0.969405622560371));
#37179=CARTESIAN_POINT('',(-0.15555,-2.01987159101623E-14,-0.129405622560369));
#37180=CARTESIAN_POINT('Ctrl Pts',(-0.155804728476752,2.95821195150548E-6,
0.95559437743963));
#37181=CARTESIAN_POINT('Ctrl Pts',(-0.155790353315504,-0.0513149683984934,
0.959286704700854));
#37182=CARTESIAN_POINT('Ctrl Pts',(-0.100033131917675,-0.154135965233235,
0.966682753644926));
#37183=CARTESIAN_POINT('Ctrl Pts',(0.0750970673805211,-0.167799333720618,
0.977782524271844));
#37184=CARTESIAN_POINT('Ctrl Pts',(0.181699613594968,-0.0279545920640164,
0.988893689320389));
#37185=CARTESIAN_POINT('Ctrl Pts',(0.122062258834496,0.137466418983892,
1.00000485436893));
#37186=CARTESIAN_POINT('Ctrl Pts',(-0.0492515922639386,0.177116921324136,
1.01111601941748));
#37187=CARTESIAN_POINT('Ctrl Pts',(-0.146173837715872,0.0831558022400444,
1.01964586044104));
#37188=CARTESIAN_POINT('Ctrl Pts',(-0.155571569202373,0.015825134364817,
1.02447197978176));
#37189=CARTESIAN_POINT('Ctrl Pts',(-0.155445081536763,0.000131810726739319,
1.02559437743963));
#37190=CARTESIAN_POINT('Ctrl Pts',(-0.155512930646214,0.000141921665610296,
0.969405622560371));
#37191=CARTESIAN_POINT('Ctrl Pts',(-0.155167703869094,-0.0383344278698275,
0.972160538458));
#37192=CARTESIAN_POINT('Ctrl Pts',(-0.121314953523015,-0.129115961930375,
0.97862166835));
#37193=CARTESIAN_POINT('Ctrl Pts',(0.0309373610575528,-0.181257875466721,
0.988789012236375));
#37194=CARTESIAN_POINT('Ctrl Pts',(0.169095195914933,-0.0722381792257861,
0.999907654219489));
#37195=CARTESIAN_POINT('Ctrl Pts',(0.152354231364944,0.102954552944809,
1.01102629620261));
#37196=CARTESIAN_POINT('Ctrl Pts',(-0.00394931635484403,0.183836962465064,
1.02214493818572));
#37197=CARTESIAN_POINT('Ctrl Pts',(-0.133855689695156,0.109373648628768,
1.03160471363831));
#37198=CARTESIAN_POINT('Ctrl Pts',(-0.15523302537302,0.0286463714736223,
1.03735827509653));
#37199=CARTESIAN_POINT('Ctrl Pts',(-0.155305653540906,-4.38315446397077E-5,
1.03940562256037));
#37200=CARTESIAN_POINT('Origin',(0.,0.,-0.129405622560369));
#37201=CARTESIAN_POINT('',(-0.155453687436568,-0.000133745576774406,0.885594377439631));
#37202=CARTESIAN_POINT('',(-0.155794751152569,-3.71416033132788E-5,0.899405622560372));
#37203=CARTESIAN_POINT('',(-0.15555,-2.01987159101623E-14,-0.129405622560369));
#37204=CARTESIAN_POINT('Ctrl Pts',(-0.155453687436568,-0.000133745576774402,
0.885594377439631));
#37205=CARTESIAN_POINT('Ctrl Pts',(-0.155579877499581,-0.0155062375664632,
0.886693986254252));
#37206=CARTESIAN_POINT('Ctrl Pts',(-0.146423861786649,-0.0825096309536398,
0.891497316751722));
#37207=CARTESIAN_POINT('Ctrl Pts',(-0.0503376402892206,-0.17681153483915,
0.900004368932038));
#37208=CARTESIAN_POINT('Ctrl Pts',(0.12121644264892,-0.138212772940753,
0.911115533980582));
#37209=CARTESIAN_POINT('Ctrl Pts',(0.181867711471885,0.026839009932345,
0.922226699029127));
#37210=CARTESIAN_POINT('Ctrl Pts',(0.0761253709552246,0.167335367481701,
0.933337864077668));
#37211=CARTESIAN_POINT('Ctrl Pts',(-0.099265255914171,0.154733978795034,
0.944449029126215));
#37212=CARTESIAN_POINT('Ctrl Pts',(-0.155732851093913,0.0517959404958592,
0.951867866913534));
#37213=CARTESIAN_POINT('Ctrl Pts',(-0.155804772838109,0.000161323939398619,
0.955582983018006));
#37214=CARTESIAN_POINT('Ctrl Pts',(-0.155804728476752,2.95821195150548E-6,
0.95559437743963));
#37215=CARTESIAN_POINT('Ctrl Pts',(-0.155794751152569,-3.71416033132616E-5,
0.899405622560372));
#37216=CARTESIAN_POINT('Ctrl Pts',(-0.155801224941728,-0.0020493184051098,
0.899550373830729));
#37217=CARTESIAN_POINT('Ctrl Pts',(-0.154853952527048,-0.055575068168544,
0.903401339095459));
#37218=CARTESIAN_POINT('Ctrl Pts',(-0.0935609375970031,-0.15829679799695,
0.91095851835456));
#37219=CARTESIAN_POINT('Ctrl Pts',(0.0823234386500799,-0.164421340203127,
0.922077160337675));
#37220=CARTESIAN_POINT('Ctrl Pts',(0.182795976495949,-0.0199287985657338,
0.933195802320793));
#37221=CARTESIAN_POINT('Ctrl Pts',(0.115819463928053,0.142819381470141,
0.944314444303908));
#37222=CARTESIAN_POINT('Ctrl Pts',(-0.0572526917402423,0.174738822826618,
0.955433086287024));
#37223=CARTESIAN_POINT('Ctrl Pts',(-0.147990815776177,0.0783419353749631,
0.963796812372513));
#37224=CARTESIAN_POINT('Ctrl Pts',(-0.15563214066504,0.01342816322173,0.968454324463628));
#37225=CARTESIAN_POINT('Ctrl Pts',(-0.155512930646214,0.000141921665610296,
0.969405622560371));
#37226=CARTESIAN_POINT('Origin',(0.,0.,-0.129405622560369));
#37227=CARTESIAN_POINT('',(-0.155333906144275,7.80263919018194E-5,0.815594377439631));
#37228=CARTESIAN_POINT('',(-0.155403083159801,-0.000119596074553197,0.829405622560371));
#37229=CARTESIAN_POINT('',(-0.15555,-2.01987159101623E-14,-0.129405622560369));
#37230=CARTESIAN_POINT('Ctrl Pts',(-0.155333906144275,7.80263919018167E-5,
0.815594377439631));
#37231=CARTESIAN_POINT('Ctrl Pts',(-0.155193217426013,-0.0308862600127516,
0.817804989490498));
#37232=CARTESIAN_POINT('Ctrl Pts',(-0.13122308335565,-0.113929638534857,
0.823719323224213));
#37233=CARTESIAN_POINT('Ctrl Pts',(0.00400949547363229,-0.183793690702293,
0.833337378640777));
#37234=CARTESIAN_POINT('Ctrl Pts',(0.156567267939011,-0.0963477420579929,
0.844448543689319));
#37235=CARTESIAN_POINT('Ctrl Pts',(0.165879203582308,0.0792482593671729,
0.855559708737864));
#37236=CARTESIAN_POINT('Ctrl Pts',(0.0234256671005791,0.182338791618694,
0.866670873786407));
#37237=CARTESIAN_POINT('Ctrl Pts',(-0.124241507899534,0.124912116508194,
0.87668243002033));
#37238=CARTESIAN_POINT('Ctrl Pts',(-0.155154841917538,0.0362716593952071,
0.882990264571404));
#37239=CARTESIAN_POINT('Ctrl Pts',(-0.155453687436568,-0.000133745576774402,
0.885594377439631));
#37240=CARTESIAN_POINT('Ctrl Pts',(-0.155403083159801,-0.000119596074553188,
0.829405622560371));
#37241=CARTESIAN_POINT('Ctrl Pts',(-0.155527408252746,-0.017480188940304,
0.830646423197829));
#37242=CARTESIAN_POINT('Ctrl Pts',(-0.14483135129372,-0.0865473027753662,
0.83559343782966));
#37243=CARTESIAN_POINT('Ctrl Pts',(-0.0434704832044991,-0.178666848096071,
0.844246666455862));
#37244=CARTESIAN_POINT('Ctrl Pts',(0.126590215885116,-0.133365823077974,
0.855365308438979));
#37245=CARTESIAN_POINT('Ctrl Pts',(0.18068878531032,0.0341040818691465,
0.866483950422094));
#37246=CARTESIAN_POINT('Ctrl Pts',(0.069268588294083,0.170333168137465,
0.877602592405212));
#37247=CARTESIAN_POINT('Ctrl Pts',(-0.103328002592178,0.150787500329959,
0.888576483117969));
#37248=CARTESIAN_POINT('Ctrl Pts',(-0.155635469933735,0.0494704907375218,
0.895844159836357));
#37249=CARTESIAN_POINT('Ctrl Pts',(-0.155794751152569,-3.71416033132616E-5,
0.899405622560372));
#37250=CARTESIAN_POINT('Origin',(0.,0.,-0.129405622560369));
#37251=CARTESIAN_POINT('',(-0.155738164088485,9.0367155389158E-5,0.745594377439631));
#37252=CARTESIAN_POINT('',(-0.155363820104426,0.000100737127591941,0.759405622560371));
#37253=CARTESIAN_POINT('',(-0.15555,-2.01987159101623E-14,-0.129405622560369));
#37254=CARTESIAN_POINT('Ctrl Pts',(-0.155738164088485,9.03671553891608E-5,
0.745594377439631));
#37255=CARTESIAN_POINT('Ctrl Pts',(-0.155418612064456,-0.0461276292775272,
0.748915992726744));
#37256=CARTESIAN_POINT('Ctrl Pts',(-0.109121796390773,-0.144436334125619,
0.755941329696705));
#37257=CARTESIAN_POINT('Ctrl Pts',(0.0580004387659595,-0.174448118065669,
0.766670388349515));
#37258=CARTESIAN_POINT('Ctrl Pts',(0.17800908511122,-0.0459234407622611,
0.777781553398057));
#37259=CARTESIAN_POINT('Ctrl Pts',(0.135154441460109,0.124617309179735,
0.788892718446602));
#37260=CARTESIAN_POINT('Ctrl Pts',(-0.0313551099181417,0.181143738163968,
0.800003883495145));
#37261=CARTESIAN_POINT('Ctrl Pts',(-0.141757073229054,0.0936656796997624,
0.808904436492822));
#37262=CARTESIAN_POINT('Ctrl Pts',(-0.155428931266511,0.0209921774117757,
0.81410126780765));
#37263=CARTESIAN_POINT('Ctrl Pts',(-0.155333906144275,7.80263919018167E-5,
0.815594377439631));
#37264=CARTESIAN_POINT('Ctrl Pts',(-0.155363820104426,0.000100737127591942,
0.759405622560371));
#37265=CARTESIAN_POINT('Ctrl Pts',(-0.155169765832855,-0.0326159426902871,
0.76174247256493));
#37266=CARTESIAN_POINT('Ctrl Pts',(-0.129071878250434,-0.117503987929593,
0.767785536563862));
#37267=CARTESIAN_POINT('Ctrl Pts',(0.0103792628149562,-0.18358593744105,
0.777534814557165));
#37268=CARTESIAN_POINT('Ctrl Pts',(0.159909575810308,-0.0907769413831382,
0.78865345654028));
#37269=CARTESIAN_POINT('Ctrl Pts',(0.162955779866738,0.0851876712390422,
0.799772098523398));
#37270=CARTESIAN_POINT('Ctrl Pts',(0.0167274199086701,0.183116681231986,
0.810890740506512));
#37271=CARTESIAN_POINT('Ctrl Pts',(-0.126795424285233,0.121093838634352,
0.820768581852172));
#37272=CARTESIAN_POINT('Ctrl Pts',(-0.155156054962447,0.0343750973057136,
0.826940209203457));
#37273=CARTESIAN_POINT('Ctrl Pts',(-0.155403083159801,-0.000119596074553188,
0.829405622560371));
#37274=CARTESIAN_POINT('Origin',(0.,0.,-0.129405622560369));
#37275=CARTESIAN_POINT('',(-0.155606466149984,-0.000136591087330588,0.67559437743963));
#37276=CARTESIAN_POINT('',(-0.155769406638298,6.77585252333857E-5,0.689405622560371));
#37277=CARTESIAN_POINT('',(-0.15555,-2.01987159101623E-14,-0.129405622560369));
#37278=CARTESIAN_POINT('Ctrl Pts',(-0.155606466149984,-0.000136591087330577,
0.67559437743963));
#37279=CARTESIAN_POINT('Ctrl Pts',(-0.155699698050756,-0.010301028373747,
0.676323274280142));
#37280=CARTESIAN_POINT('Ctrl Pts',(-0.150160999329305,-0.0720125819190329,
0.680755892803501));
#37281=CARTESIAN_POINT('Ctrl Pts',(-0.0677079673289082,-0.170914680334463,
0.68889223300971));
#37282=CARTESIAN_POINT('Ctrl Pts',(0.106838781720774,-0.149605051766532,
0.700003398058251));
#37283=CARTESIAN_POINT('Ctrl Pts',(0.183637062036826,0.00858057341481814,
0.711114563106797));
#37284=CARTESIAN_POINT('Ctrl Pts',(0.0924229284360449,0.1589156980696,0.722225728155339));
#37285=CARTESIAN_POINT('Ctrl Pts',(-0.0833503847528551,0.163856370505402,
0.733336893203883));
#37286=CARTESIAN_POINT('Ctrl Pts',(-0.153115801604342,0.0622214122864029,
0.741126442965314));
#37287=CARTESIAN_POINT('Ctrl Pts',(-0.155774924177056,0.00540711533618156,
0.745212271043896));
#37288=CARTESIAN_POINT('Ctrl Pts',(-0.155738164088485,9.03671553891608E-5,
0.745594377439631));
#37289=CARTESIAN_POINT('Ctrl Pts',(-0.155769406638298,6.77585252333878E-5,
0.689405622560371));
#37290=CARTESIAN_POINT('Ctrl Pts',(-0.155508734647919,-0.0476733936548398,
0.692838521932031));
#37291=CARTESIAN_POINT('Ctrl Pts',(-0.106472330039144,-0.147419539900055,
0.699977635298063));
#37292=CARTESIAN_POINT('Ctrl Pts',(0.0633314188332071,-0.172628667698419,
0.710822962658467));
#37293=CARTESIAN_POINT('Ctrl Pts',(0.17940008868909,-0.0403377453646542,
0.721941604641583));
#37294=CARTESIAN_POINT('Ctrl Pts',(0.131130494233742,0.128904301731096,
0.733060246624699));
#37295=CARTESIAN_POINT('Ctrl Pts',(-0.0372603218894873,0.180064416072257,
0.744178888607816));
#37296=CARTESIAN_POINT('Ctrl Pts',(-0.143301362666466,0.0901927254173143,
0.752960680586373));
#37297=CARTESIAN_POINT('Ctrl Pts',(-0.155477533406966,0.0192722899107996,
0.758036258570558));
#37298=CARTESIAN_POINT('Ctrl Pts',(-0.155363820104426,0.000100737127591942,
0.759405622560371));
#37299=CARTESIAN_POINT('Origin',(0.,0.,-0.129405622560369));
#37300=CARTESIAN_POINT('',(-0.155295085115974,-2.74912889200857E-6,0.60559437743963));
#37301=CARTESIAN_POINT('',(-0.155567057787938,-0.000141549514015751,0.619405622560371));
#37302=CARTESIAN_POINT('',(-0.15555,-2.01987159101623E-14,-0.129405622560369));
#37303=CARTESIAN_POINT('Ctrl Pts',(-0.155295114066544,-2.74881667468134E-6,
0.60559437743963));
#37304=CARTESIAN_POINT('Ctrl Pts',(-0.155299180574127,-0.0257905198155464,
0.607434277516388));
#37305=CARTESIAN_POINT('Ctrl Pts',(-0.137005956536857,-0.103483686203599,
0.612977899275993));
#37306=CARTESIAN_POINT('Ctrl Pts',(-0.0143272298638598,-0.183278278249422,
0.622225242718446));
#37307=CARTESIAN_POINT('Ctrl Pts',(0.146185859526926,-0.111471481859797,
0.63333640776699));
#37308=CARTESIAN_POINT('Ctrl Pts',(0.172951224644592,0.0623223129190563,
0.644447572815534));
#37309=CARTESIAN_POINT('Ctrl Pts',(0.0414808152398764,0.179096450999678,
0.655558737864077));
#37310=CARTESIAN_POINT('Ctrl Pts',(-0.11682689842466,0.135101180160119,
0.66594100607211));
#37311=CARTESIAN_POINT('Ctrl Pts',(-0.155225961585962,0.0413472223515983,
0.672619552597294));
#37312=CARTESIAN_POINT('Ctrl Pts',(-0.155606466149984,-0.000136591087330577,
0.67559437743963));
#37313=CARTESIAN_POINT('Ctrl Pts',(-0.155567057787938,-0.000141549514015748,
0.619405622560371));
#37314=CARTESIAN_POINT('Ctrl Pts',(-0.155673152840384,-0.011622012238534,
0.62022835730476));
#37315=CARTESIAN_POINT('Ctrl Pts',(-0.149271086742403,-0.0747018195902368,
0.62475730604352));
#37316=CARTESIAN_POINT('Ctrl Pts',(-0.0632665469493242,-0.172652453095426,
0.632992468776653));
#37317=CARTESIAN_POINT('Ctrl Pts',(0.110806726459172,-0.146742614445027,
0.644111110759769));
#37318=CARTESIAN_POINT('Ctrl Pts',(0.183376231205259,0.0135898253011021,
0.655229752742886));
#37319=CARTESIAN_POINT('Ctrl Pts',(0.0879651525947856,0.161473395492061,
0.666348394726001));
#37320=CARTESIAN_POINT('Ctrl Pts',(-0.0880258220622017,0.161440330069759,
0.677467036709119));
#37321=CARTESIAN_POINT('Ctrl Pts',(-0.153940153309356,0.0591912849892102,
0.685152779320574));
#37322=CARTESIAN_POINT('Ctrl Pts',(-0.155790160368306,0.00386873070159844,
0.689132307937659));
#37323=CARTESIAN_POINT('Ctrl Pts',(-0.155769406638298,6.77585252333878E-5,
0.689405622560371));
#37324=CARTESIAN_POINT('Origin',(0.,0.,-0.129405622560369));
#37325=CARTESIAN_POINT('',(-0.155596383579478,0.000138071545366175,0.53559437743963));
#37326=CARTESIAN_POINT('',(-0.15529563387483,1.51106445085702E-5,0.549405622560371));
#37327=CARTESIAN_POINT('',(-0.15555,-2.01987159101623E-14,-0.129405622560369));
#37328=CARTESIAN_POINT('Ctrl Pts',(-0.155596383579478,0.000138071545366179,
0.53559437743963));
#37329=CARTESIAN_POINT('Ctrl Pts',(-0.155217514150148,-0.0410190199764792,
0.538545280752634));
#37330=CARTESIAN_POINT('Ctrl Pts',(-0.117330640529453,-0.134449549172498,
0.545199905748485));
#37331=CARTESIAN_POINT('Ctrl Pts',(0.0403262995152723,-0.179359935217008,
0.555558252427184));
#37332=CARTESIAN_POINT('Ctrl Pts',(0.172546185411942,-0.0634350903950841,
0.566669417475728));
#37333=CARTESIAN_POINT('Ctrl Pts',(0.146900873501267,0.11052750860401,0.577780582524271));
#37334=CARTESIAN_POINT('Ctrl Pts',(-0.013146340126236,0.183366765077345,
0.588891747572816));
#37335=CARTESIAN_POINT('Ctrl Pts',(-0.136655195880861,0.104159698732297,
0.598163012544601));
#37336=CARTESIAN_POINT('Ctrl Pts',(-0.155290994688111,0.0261203028467153,
0.60373055583354));
#37337=CARTESIAN_POINT('Ctrl Pts',(-0.155295114066544,-2.74881667468134E-6,
0.60559437743963));
#37338=CARTESIAN_POINT('Ctrl Pts',(-0.15529563387483,1.51106445085633E-5,
0.549405622560371));
#37339=CARTESIAN_POINT('Ctrl Pts',(-0.155272340811799,-0.0268780222436924,
0.55132440667186));
#37340=CARTESIAN_POINT('Ctrl Pts',(-0.135831396530156,-0.105747938365068,
0.556949404777722));
#37341=CARTESIAN_POINT('Ctrl Pts',(-0.0103102773360761,-0.183589824620028,
0.566280616877956));
#37342=CARTESIAN_POINT('Ctrl Pts',(0.14869956060099,-0.108166382022474,
0.577399258861071));
#37343=CARTESIAN_POINT('Ctrl Pts',(0.171494149863546,0.0663421591850832,
0.588517900844189));
#37344=CARTESIAN_POINT('Ctrl Pts',(0.0371926577693494,0.180078404398782,
0.599636542827304));
#37345=CARTESIAN_POINT('Ctrl Pts',(-0.118720103315053,0.132645343006727,
0.609932450066032));
#37346=CARTESIAN_POINT('Ctrl Pts',(-0.155195221197423,0.040094597399841,
0.616522143310387));
#37347=CARTESIAN_POINT('Ctrl Pts',(-0.155567057787938,-0.000141549514015748,
0.619405622560371));
#37348=CARTESIAN_POINT('Origin',(0.,0.,-0.129405622560369));
#37349=CARTESIAN_POINT('',(-0.155745492001379,-8.56371120316567E-5,0.46559437743963));
#37350=CARTESIAN_POINT('',(-0.155622585425313,0.000134239099646036,0.479405622560371));
#37351=CARTESIAN_POINT('',(-0.15555,-2.01987159101623E-14,-0.129405622560369));
#37352=CARTESIAN_POINT('Ctrl Pts',(-0.155745492001379,-8.56371120316864E-5,
0.465594377439631));
#37353=CARTESIAN_POINT('Ctrl Pts',(-0.15577850741697,-0.00506891626144068,
0.465952562306032));
#37354=CARTESIAN_POINT('Ctrl Pts',(-0.153301192978291,-0.0615473136307116,
0.470014468855281));
#37355=CARTESIAN_POINT('Ctrl Pts',(-0.0844041411881997,-0.163316067010957,
0.477780097087378));
#37356=CARTESIAN_POINT('Ctrl Pts',(0.0913973507436636,-0.159507746114991,
0.488891262135923));
#37357=CARTESIAN_POINT('Ctrl Pts',(0.183577980123458,-0.00976329900371924,
0.500002427184466));
#37358=CARTESIAN_POINT('Ctrl Pts',(0.10780025055099,0.148913742733129,0.51111359223301));
#37359=CARTESIAN_POINT('Ctrl Pts',(-0.0666056105926533,0.17134727727987,
0.522224757281553));
#37360=CARTESIAN_POINT('Ctrl Pts',(-0.149938299705611,0.0726891414718789,
0.530385019017093));
#37361=CARTESIAN_POINT('Ctrl Pts',(-0.155693038683329,0.0106378444150779,
0.534841559069786));
#37362=CARTESIAN_POINT('Ctrl Pts',(-0.155596383579478,0.000138071545366179,
0.53559437743963));
#37363=CARTESIAN_POINT('Ctrl Pts',(-0.155622585425313,0.000134239099646029,
0.479405622560371));
#37364=CARTESIAN_POINT('Ctrl Pts',(-0.155239700220769,-0.0418962472451577,
0.482420456038961));
#37365=CARTESIAN_POINT('Ctrl Pts',(-0.115964303797854,-0.136226320639006,
0.489141503511923));
#37366=CARTESIAN_POINT('Ctrl Pts',(0.0435376164803608,-0.17865050090601,
0.499568764979258));
#37367=CARTESIAN_POINT('Ctrl Pts',(0.173732980498774,-0.0602360109052031,
0.510687406962374));
#37368=CARTESIAN_POINT('Ctrl Pts',(0.144781397169404,0.113357278356683,
0.521806048945491));
#37369=CARTESIAN_POINT('Ctrl Pts',(-0.0167962271460079,0.183110382765203,
0.532924690928607));
#37370=CARTESIAN_POINT('Ctrl Pts',(-0.137758975876034,0.102035875886683,
0.542124548800234));
#37371=CARTESIAN_POINT('Ctrl Pts',(-0.155317332364345,0.0250672199885809,
0.547618192677488));
#37372=CARTESIAN_POINT('Ctrl Pts',(-0.15529563387483,1.51106445085633E-5,
0.549405622560371));
#37373=CARTESIAN_POINT('Origin',(0.,0.,-0.129405622560369));
#37374=CARTESIAN_POINT('',(-0.155339129538237,-8.2587420025254E-5,0.39559437743963));
#37375=CARTESIAN_POINT('',(-0.15573160577951,-9.4952305265919E-5,0.409405622560371));
#37376=CARTESIAN_POINT('',(-0.15555,-2.01987159101623E-14,-0.129405622560369));
#37377=CARTESIAN_POINT('Ctrl Pts',(-0.155339129538237,-8.25874200252562E-5,
0.39559437743963));
#37378=CARTESIAN_POINT('Ctrl Pts',(-0.155438295724494,-0.0206599346759669,
0.397063565542278));
#37379=CARTESIAN_POINT('Ctrl Pts',(-0.142062281789543,-0.0929876204718288,
0.402236475327773));
#37380=CARTESIAN_POINT('Ctrl Pts',(-0.0325213021862407,-0.180938005122649,
0.411113106796117));
#37381=CARTESIAN_POINT('Ctrl Pts',(0.134348911316817,-0.125485325124609,
0.42222427184466));
#37382=CARTESIAN_POINT('Ctrl Pts',(0.178301209192838,0.0447758371671112,
0.433335436893204));
#37383=CARTESIAN_POINT('Ctrl Pts',(0.0591229481908682,0.174070887258225,
0.444446601941748));
#37384=CARTESIAN_POINT('Ctrl Pts',(-0.10856218085317,0.145071736103991,
0.455199582123889));
#37385=CARTESIAN_POINT('Ctrl Pts',(-0.155437119708937,0.0464594445617744,
0.462248840623184));
#37386=CARTESIAN_POINT('Ctrl Pts',(-0.155745492001379,-8.56371120316864E-5,
0.465594377439631));
#37387=CARTESIAN_POINT('Ctrl Pts',(-0.15573160577951,-9.49523052659442E-5,
0.40940562256037));
#37388=CARTESIAN_POINT('Ctrl Pts',(-0.155772052747877,-0.00572626470532979,
0.40981029141169));
#37389=CARTESIAN_POINT('Ctrl Pts',(-0.152938259291224,-0.0628915705084586,
0.413921174257381));
#37390=CARTESIAN_POINT('Ctrl Pts',(-0.0822616502622442,-0.164452261823584,
0.421738271097444));
#37391=CARTESIAN_POINT('Ctrl Pts',(0.0936204134582059,-0.158261630557358,
0.43285691308056));
#37392=CARTESIAN_POINT('Ctrl Pts',(0.183742116834086,-0.00709647969689106,
0.443975555063676));
#37393=CARTESIAN_POINT('Ctrl Pts',(0.10554806974386,0.150569354438759,0.455094197046793));
#37394=CARTESIAN_POINT('Ctrl Pts',(-0.0693325883166112,0.170307127625589,
0.466212839029909));
#37395=CARTESIAN_POINT('Ctrl Pts',(-0.150503746143118,0.0709862178387775,
0.474316647534435));
#37396=CARTESIAN_POINT('Ctrl Pts',(-0.155710391061042,0.00977293375193425,
0.478714242044589));
#37397=CARTESIAN_POINT('Ctrl Pts',(-0.155622585425313,0.000134239099646029,
0.479405622560371));
#37398=CARTESIAN_POINT('Origin',(0.,0.,-0.129405622560369));
#37399=CARTESIAN_POINT('',(-0.155444674488022,0.000131742778884735,0.32559437743963));
#37400=CARTESIAN_POINT('',(-0.15533186684889,-7.70198572060954E-5,0.339405622560371));
#37401=CARTESIAN_POINT('',(-0.15555,-2.01987159101623E-14,-0.129405622560369));
#37402=CARTESIAN_POINT('Ctrl Pts',(-0.155444674488022,0.000131742778884739,
0.32559437743963));
#37403=CARTESIAN_POINT('Ctrl Pts',(-0.155154236665719,-0.0359445316439912,
0.328174568778523));
#37404=CARTESIAN_POINT('Ctrl Pts',(-0.124691611905359,-0.124248704432008,
0.334458481800264));
#37405=CARTESIAN_POINT('Ctrl Pts',(0.0222506403513669,-0.18248590575151,
0.344446116504855));
#37406=CARTESIAN_POINT('Ctrl Pts',(0.165365282072159,-0.0803151310699741,
0.355557281553397));
#37407=CARTESIAN_POINT('Ctrl Pts',(0.157184646516792,0.0953372104320743,
0.366668446601942));
#37408=CARTESIAN_POINT('Ctrl Pts',(0.00519332482321354,0.183764050268212,
0.377779611650485));
#37409=CARTESIAN_POINT('Ctrl Pts',(-0.130823935507303,0.114600960175539,
0.387421588596382));
#37410=CARTESIAN_POINT('Ctrl Pts',(-0.155188304621527,0.0312141358191517,
0.39335984385943));
#37411=CARTESIAN_POINT('Ctrl Pts',(-0.155339129538237,-8.25874200252562E-5,
0.39559437743963));
#37412=CARTESIAN_POINT('Ctrl Pts',(-0.15533186684889,-7.70198572060919E-5,
0.339405622560371));
#37413=CARTESIAN_POINT('Ctrl Pts',(-0.155425971941861,-0.0210984061911746,
0.34090634077879));
#37414=CARTESIAN_POINT('Ctrl Pts',(-0.141654850766895,-0.0939166341982764,
0.346113272991582));
#37415=CARTESIAN_POINT('Ctrl Pts',(-0.0308692884081366,-0.181269447386996,
0.355026419198746));
#37416=CARTESIAN_POINT('Ctrl Pts',(0.135606994996762,-0.124186426112907,
0.366145061181863));
#37417=CARTESIAN_POINT('Ctrl Pts',(0.177861387826841,0.0466567491694538,
0.377263703164979));
#37418=CARTESIAN_POINT('Ctrl Pts',(0.0571870330903418,0.174760318061885,
0.388382345148095));
#37419=CARTESIAN_POINT('Ctrl Pts',(-0.109574509035902,0.143939945308724,
0.399096318279893));
#37420=CARTESIAN_POINT('Ctrl Pts',(-0.155401613758806,0.0458488658137791,
0.406104077417318));
#37421=CARTESIAN_POINT('Ctrl Pts',(-0.15573160577951,-9.49523052659442E-5,
0.40940562256037));
#37422=CARTESIAN_POINT('Origin',(0.,0.,-0.129405622560369));
#37423=CARTESIAN_POINT('',(-0.155804712705668,3.25009013604671E-6,0.25559437743963));
#37424=CARTESIAN_POINT('',(-0.155449947323643,0.000133480041304715,0.269405622560371));
#37425=CARTESIAN_POINT('',(-0.15555,-2.01987159101623E-14,-0.129405622560369));
#37426=CARTESIAN_POINT('Ctrl Pts',(-0.155804712705668,3.25009013604029E-6,
0.25559437743963));
#37427=CARTESIAN_POINT('Ctrl Pts',(-0.155788927539753,-0.0512989453804214,
0.259285572014769));
#37428=CARTESIAN_POINT('Ctrl Pts',(-0.10006227616332,-0.154106832868198,
0.266680488272757));
#37429=CARTESIAN_POINT('Ctrl Pts',(0.0750458968510211,-0.167822257683237,
0.277779126213592));
#37430=CARTESIAN_POINT('Ctrl Pts',(0.181691053470019,-0.0280099604209337,
0.288890291262136));
#37431=CARTESIAN_POINT('Ctrl Pts',(0.122104229764526,0.137429086670804,
0.30000145631068));
#37432=CARTESIAN_POINT('Ctrl Pts',(-0.0491976593161155,0.177132117679823,
0.311112621359223));
#37433=CARTESIAN_POINT('Ctrl Pts',(-0.146161229246342,0.0831876851886141,
0.319643595068874));
#37434=CARTESIAN_POINT('Ctrl Pts',(-0.155571144064704,0.0158409610837222,
0.324470847095676));
#37435=CARTESIAN_POINT('Ctrl Pts',(-0.155444674488022,0.000131742778884739,
0.32559437743963));
#37436=CARTESIAN_POINT('Ctrl Pts',(-0.155449947323643,0.000133480041304701,
0.269405622560371));
#37437=CARTESIAN_POINT('Ctrl Pts',(-0.155153406972295,-0.0361714100102126,
0.272002390145891));
#37438=CARTESIAN_POINT('Ctrl Pts',(-0.12437032104418,-0.124745277135715,
0.278305371725784));
#37439=CARTESIAN_POINT('Ctrl Pts',(0.0231926238140432,-0.182410602009977,
0.288314567300049));
#37440=CARTESIAN_POINT('Ctrl Pts',(0.165866396469461,-0.0793716828903688,
0.299433209283165));
#37441=CARTESIAN_POINT('Ctrl Pts',(0.156599354026699,0.096375141196464,
0.310551851266282));
#37442=CARTESIAN_POINT('Ctrl Pts',(0.00388050940998321,0.183838154825996,
0.321670493249398));
#37443=CARTESIAN_POINT('Ctrl Pts',(-0.131300314367493,0.113822266482633,
0.331288417014094));
#37444=CARTESIAN_POINT('Ctrl Pts',(-0.155193567478298,0.0308165737536199,
0.337200126784418));
#37445=CARTESIAN_POINT('Ctrl Pts',(-0.15533186684889,-7.70198572060919E-5,
0.339405622560371));
#37446=CARTESIAN_POINT('Origin',(0.,0.,-0.129405622560369));
#37447=CARTESIAN_POINT('',(-0.155454118234884,-0.000133834695600709,0.18559437743963));
#37448=CARTESIAN_POINT('',(-0.155805467550008,3.4854191793785E-6,0.19940562256037));
#37449=CARTESIAN_POINT('',(-0.15555,-2.01987159101623E-14,-0.129405622560369));
#37450=CARTESIAN_POINT('Ctrl Pts',(-0.155454118234884,-0.000133834695600729,
0.18559437743963));
#37451=CARTESIAN_POINT('Ctrl Pts',(-0.155580288786201,-0.0154903851691022,
0.186692853568168));
#37452=CARTESIAN_POINT('Ctrl Pts',(-0.146436232298065,-0.0824775316270878,
0.191495051379553));
#37453=CARTESIAN_POINT('Ctrl Pts',(-0.0503915664640746,-0.176796168665343,
0.200000970873786));
#37454=CARTESIAN_POINT('Ctrl Pts',(0.121174280763407,-0.138249741391359,
0.21111213592233));
#37455=CARTESIAN_POINT('Ctrl Pts',(0.181875888824183,0.0267835396201195,
0.222223300970874));
#37456=CARTESIAN_POINT('Ctrl Pts',(0.0761764071097843,0.167312138149853,
0.233334466019417));
#37457=CARTESIAN_POINT('Ctrl Pts',(-0.0992180579104728,0.154764252547341,
0.244445631067961));
#37458=CARTESIAN_POINT('Ctrl Pts',(-0.155725669913861,0.0518277207581445,
0.251865601541365));
#37459=CARTESIAN_POINT('Ctrl Pts',(-0.155804766277071,0.00017735852989955,
0.255581850331921));
#37460=CARTESIAN_POINT('Ctrl Pts',(-0.155804712705668,3.25009013604029E-6,
0.25559437743963));
#37461=CARTESIAN_POINT('Ctrl Pts',(-0.155805467550008,3.48541917938314E-6,
0.19940562256037));
#37462=CARTESIAN_POINT('Ctrl Pts',(-0.155788564535512,-0.0513206116891616,
0.203098439512992));
#37463=CARTESIAN_POINT('Ctrl Pts',(-0.100003893378143,-0.154186484140614,
0.210497470459985));
#37464=CARTESIAN_POINT('Ctrl Pts',(0.0752488571272716,-0.167777039880966,
0.221602715401351));
#37465=CARTESIAN_POINT('Ctrl Pts',(0.181781810074028,-0.0276929424335053,
0.232721357384467));
#37466=CARTESIAN_POINT('Ctrl Pts',(0.121794738393109,0.137759091140133,
0.243839999367584));
#37467=CARTESIAN_POINT('Ctrl Pts',(-0.0497615974795104,0.177017821004958,
0.2549586413507));
#37468=CARTESIAN_POINT('Ctrl Pts',(-0.146313162187878,0.0828233020270418,
0.263480515748296));
#37469=CARTESIAN_POINT('Ctrl Pts',(-0.155576641614544,0.0156444291597347,
0.268296176151519));
#37470=CARTESIAN_POINT('Ctrl Pts',(-0.155449947323643,0.000133480041304701,
0.269405622560371));
#37471=CARTESIAN_POINT('Origin',(0.,0.,-0.129405622560369));
#37472=CARTESIAN_POINT('',(-0.155333634177863,7.79921548230329E-5,0.11559437743963));
#37473=CARTESIAN_POINT('',(-0.155460191805193,-0.000135568056800359,0.12940562256037));
#37474=CARTESIAN_POINT('',(-0.15555,-2.01987159101623E-14,-0.129405622560369));
#37475=CARTESIAN_POINT('Ctrl Pts',(-0.155333634177863,7.79921548230561E-5,
0.11559437743963));
#37476=CARTESIAN_POINT('Ctrl Pts',(-0.155193438638927,-0.0308706275100063,
0.117803856804414));
#37477=CARTESIAN_POINT('Ctrl Pts',(-0.131241956589738,-0.11389814578602,
0.123717057852045));
#37478=CARTESIAN_POINT('Ctrl Pts',(0.00395347168138628,-0.183794704008407,
0.133333980582524));
#37479=CARTESIAN_POINT('Ctrl Pts',(0.156537855283131,-0.0963955976349113,
0.144445145631068));
#37480=CARTESIAN_POINT('Ctrl Pts',(0.165903376979378,0.0791977165381959,
0.155556310679611));
#37481=CARTESIAN_POINT('Ctrl Pts',(0.0234812759114929,0.182331608910266,
0.166667475728155));
#37482=CARTESIAN_POINT('Ctrl Pts',(-0.124220109658982,0.124943524423025,
0.176680164648161));
#37483=CARTESIAN_POINT('Ctrl Pts',(-0.155154880719052,0.0362871523529771,
0.18298913188532));
#37484=CARTESIAN_POINT('Ctrl Pts',(-0.155454118234884,-0.000133834695600729,
0.18559437743963));
#37485=CARTESIAN_POINT('Ctrl Pts',(-0.155460191805193,-0.000135568056800364,
0.12940562256037));
#37486=CARTESIAN_POINT('Ctrl Pts',(-0.15558637635503,-0.0152693971168416,
0.130488274885721));
#37487=CARTESIAN_POINT('Ctrl Pts',(-0.146605510259419,-0.0820638709603335,
0.135277141205443));
#37488=CARTESIAN_POINT('Ctrl Pts',(-0.0510374815939226,-0.176654153931159,
0.143772221519537));
#37489=CARTESIAN_POINT('Ctrl Pts',(0.120797626960931,-0.138634273102519,
0.154890863502654));
#37490=CARTESIAN_POINT('Ctrl Pts',(0.181976886629041,0.0263806680570579,
0.16600950548577));
#37491=CARTESIAN_POINT('Ctrl Pts',(0.0764574137846417,0.167229745635935,
0.177128147468886));
#37492=CARTESIAN_POINT('Ctrl Pts',(-0.0991003621173195,0.154889135395602,
0.188246789452002));
#37493=CARTESIAN_POINT('Ctrl Pts',(-0.15572087700955,0.0518861158146895,
0.195672614482497));
#37494=CARTESIAN_POINT('Ctrl Pts',(-0.155805528871865,0.000189682319971778,
0.19939222551862));
#37495=CARTESIAN_POINT('Ctrl Pts',(-0.155805467550008,3.48541917938314E-6,
0.19940562256037));
#37496=CARTESIAN_POINT('Origin',(0.,0.,-0.129405622560369));
#37497=CARTESIAN_POINT('',(-0.155735926886437,0.000101346774827271,0.0455943774396301));
#37498=CARTESIAN_POINT('',(-0.155326046963413,7.29270061605516E-5,0.0594056225603705));
#37499=CARTESIAN_POINT('',(-0.15555,-2.01987159101623E-14,-0.129405622560369));
#37500=CARTESIAN_POINT('Ctrl Pts',(-0.155735926886437,0.000101346774827265,
0.0455943774396301));
#37501=CARTESIAN_POINT('Ctrl Pts',(-0.15541538777776,-0.0460983628495037,
0.0489148600406595));
#37502=CARTESIAN_POINT('Ctrl Pts',(-0.109151218308356,-0.144423481489054,
0.0559390643245367));
#37503=CARTESIAN_POINT('Ctrl Pts',(0.0579488995883613,-0.174456230311225,
0.0666669902912619));
#37504=CARTESIAN_POINT('Ctrl Pts',(0.177994191588978,-0.0459827600750814,
0.0777781553398056));
#37505=CARTESIAN_POINT('Ctrl Pts',(0.135192905881154,0.124578720765632,
0.0888893203883492));
#37506=CARTESIAN_POINT('Ctrl Pts',(-0.0313001003158473,0.181151906168851,
0.100000485436893));
#37507=CARTESIAN_POINT('Ctrl Pts',(-0.141742497137191,0.093698092273704,
0.108902171120653));
#37508=CARTESIAN_POINT('Ctrl Pts',(-0.155428446607623,0.0210081433596544,
0.114100135121566));
#37509=CARTESIAN_POINT('Ctrl Pts',(-0.155333634177863,7.79921548230561E-5,
0.11559437743963));
#37510=CARTESIAN_POINT('Ctrl Pts',(-0.155326046963413,7.29270061605551E-5,
0.0594056225603705));
#37511=CARTESIAN_POINT('Ctrl Pts',(-0.155199262831984,-0.0304485333833814,
0.0615843242528215));
#37512=CARTESIAN_POINT('Ctrl Pts',(-0.131743653601245,-0.113071739766558,
0.0674692399396446));
#37513=CARTESIAN_POINT('Ctrl Pts',(0.00255447675030308,-0.183860034663711,
0.0770603696208398));
#37514=CARTESIAN_POINT('Ctrl Pts',(0.155899683301632,-0.0975032021788082,
0.0881790116039561));
#37515=CARTESIAN_POINT('Ctrl Pts',(0.166434877052597,0.0781732535368643,
0.0992976535870723));
#37516=CARTESIAN_POINT('Ctrl Pts',(0.0245080507541896,0.182238325373942,
0.110416295570189));
#37517=CARTESIAN_POINT('Ctrl Pts',(-0.123863138927055,0.125487925833816,
0.120452285227955));
#37518=CARTESIAN_POINT('Ctrl Pts',(-0.155154412248428,0.0365378245899198,
0.126782060891349));
#37519=CARTESIAN_POINT('Ctrl Pts',(-0.155460191805193,-0.000135568056800364,
0.12940562256037));
#37520=CARTESIAN_POINT('Origin',(0.,0.,1.15));
#37521=CARTESIAN_POINT('',(-0.177892626630995,-0.00012009523392913,1.12223275485995));
#37522=CARTESIAN_POINT('Ctrl Pts',(0.155548765964692,0.000619602180104872,
1.14445));
#37523=CARTESIAN_POINT('Ctrl Pts',(0.156083861551471,-0.0102125174737046,
1.14395805623115));
#37524=CARTESIAN_POINT('Ctrl Pts',(0.15539846640382,-0.0210404421466269,
1.14347026853365));
#37525=CARTESIAN_POINT('Ctrl Pts',(0.153608590638952,-0.0317127652002419,
1.14298392615444));
#37526=CARTESIAN_POINT('Ctrl Pts',(0.152914716720618,-0.0358500616318106,
1.14279538776594));
#37527=CARTESIAN_POINT('Ctrl Pts',(0.152054287987853,-0.0399640361908485,
1.14260706658696));
#37528=CARTESIAN_POINT('Ctrl Pts',(0.151032028551573,-0.0440458121014301,
1.1424188046881));
#37529=CARTESIAN_POINT('Ctrl Pts',(0.150071136707034,-0.0478825535826186,
1.14224184440107));
#37530=CARTESIAN_POINT('Ctrl Pts',(0.148969254907822,-0.0516824965112672,
1.14206531990211));
#37531=CARTESIAN_POINT('Ctrl Pts',(0.147732675525468,-0.0554351396328931,
1.14188926057926));
#37532=CARTESIAN_POINT('Ctrl Pts',(0.144705099540774,-0.0646229138722882,
1.14145820618411));
#37533=CARTESIAN_POINT('Ctrl Pts',(0.14087037084284,-0.0735342808861364,
1.14102963880076));
#37534=CARTESIAN_POINT('Ctrl Pts',(0.136287966367236,-0.0820616333277537,
1.14060170770949));
#37535=CARTESIAN_POINT('Ctrl Pts',(0.134099734044687,-0.0861336938230361,
1.1403973580824));
#37536=CARTESIAN_POINT('Ctrl Pts',(0.131738457084688,-0.090120565054425,
1.14019301071694));
#37537=CARTESIAN_POINT('Ctrl Pts',(0.129223539536337,-0.0939888668888786,
1.1399895855729));
#37538=CARTESIAN_POINT('Ctrl Pts',(0.123841150615535,-0.102267748615928,
1.1395542181223));
#37539=CARTESIAN_POINT('Ctrl Pts',(0.117747056171278,-0.110025200831312,
1.1391220629978));
#37540=CARTESIAN_POINT('Ctrl Pts',(0.11100116606729,-0.117148456023219,
1.13869123413476));
#37541=CARTESIAN_POINT('Ctrl Pts',(0.106906026602935,-0.121472677586479,
1.13842969647966));
#37542=CARTESIAN_POINT('Ctrl Pts',(0.102570142764087,-0.125562999006382,
1.13816864757596));
#37543=CARTESIAN_POINT('Ctrl Pts',(0.0980025572591369,-0.129390839920029,
1.13790766548932));
#37544=CARTESIAN_POINT('Ctrl Pts',(0.0956731876101781,-0.131342955854285,
1.13777457027942));
#37545=CARTESIAN_POINT('Ctrl Pts',(0.0932817165779503,-0.133228060285772,
1.13764139558094));
#37546=CARTESIAN_POINT('Ctrl Pts',(0.0908350990518728,-0.135037587415829,
1.1375084117344));
#37547=CARTESIAN_POINT('Ctrl Pts',(0.0901763381324703,-0.135524809363345,
1.13747260533636));
#37548=CARTESIAN_POINT('Ctrl Pts',(0.0895137718121014,-0.136006421121091,
1.1374368229172));
#37549=CARTESIAN_POINT('Ctrl Pts',(0.0888474357058895,-0.136482361432558,
1.13740106343829));
#37550=CARTESIAN_POINT('Ctrl Pts',(0.0798411198483208,-0.142915254284167,
1.1369177320399));
#37551=CARTESIAN_POINT('Ctrl Pts',(0.0701492813036541,-0.148315340119806,
1.1364385915245));
#37552=CARTESIAN_POINT('Ctrl Pts',(0.059971176200061,-0.152699426079087,
1.13596107719954));
#37553=CARTESIAN_POINT('Ctrl Pts',(0.0530631196487977,-0.155674981295315,
1.13563697994103));
#37554=CARTESIAN_POINT('Ctrl Pts',(0.0459300802687867,-0.158181722966519,
1.13531363179894));
#37555=CARTESIAN_POINT('Ctrl Pts',(0.0386275637501033,-0.16021396300419,
1.13499023090658));
#37556=CARTESIAN_POINT('Ctrl Pts',(0.0351988940876516,-0.161168138149998,
1.13483838806916));
#37557=CARTESIAN_POINT('Ctrl Pts',(0.0317324236549294,-0.162017357570902,
1.13468652012024));
#37558=CARTESIAN_POINT('Ctrl Pts',(0.028249074324747,-0.162757963065587,
1.13453519958799));
#37559=CARTESIAN_POINT('Ctrl Pts',(0.0167982212800381,-0.165192563755867,
1.13403776191718));
#37560=CARTESIAN_POINT('Ctrl Pts',(0.00512774808450533,-0.166468890755321,
1.13354451715097));
#37561=CARTESIAN_POINT('Ctrl Pts',(-0.00655533748915361,-0.166579173106486,
1.13305265956701));
#37562=CARTESIAN_POINT('Ctrl Pts',(-0.0141044995850598,-0.166650433334789,
1.1327348400487));
#37563=CARTESIAN_POINT('Ctrl Pts',(-0.0216594951399176,-0.166233867742642,
1.13241759971353));
#37564=CARTESIAN_POINT('Ctrl Pts',(-0.0291655735035569,-0.165315833865676,
1.13210018160962));
#37565=CARTESIAN_POINT('Ctrl Pts',(-0.0327092118793667,-0.164882427775424,
1.13195032772857));
#37566=CARTESIAN_POINT('Ctrl Pts',(-0.0362323925945039,-0.164338226995567,
1.13180083633464));
#37567=CARTESIAN_POINT('Ctrl Pts',(-0.0397271405986897,-0.163683459359474,
1.13165172827032));
#37568=CARTESIAN_POINT('Ctrl Pts',(-0.0499359232133337,-0.16177076624055,
1.13121615700369));
#37569=CARTESIAN_POINT('Ctrl Pts',(-0.0599087164806791,-0.158916175424461,
1.13078358684414));
#37570=CARTESIAN_POINT('Ctrl Pts',(-0.0695044280650932,-0.155097228857054,
1.13035212687658));
#37571=CARTESIAN_POINT('Ctrl Pts',(-0.0757996376989387,-0.152591831627178,
1.1300690701256));
#37572=CARTESIAN_POINT('Ctrl Pts',(-0.0819325841193579,-0.149670688079838,
1.12978649119439));
#37573=CARTESIAN_POINT('Ctrl Pts',(-0.0878818038415969,-0.146365274834167,
1.12950385616925));
#37574=CARTESIAN_POINT('Ctrl Pts',(-0.0910874459297812,-0.144584205666465,
1.12935156279727));
#37575=CARTESIAN_POINT('Ctrl Pts',(-0.09424019426452,-0.142690781721644,
1.129199221353));
#37576=CARTESIAN_POINT('Ctrl Pts',(-0.0973230172632952,-0.140698989172901,
1.12904742410559));
#37577=CARTESIAN_POINT('Ctrl Pts',(-0.107217543799977,-0.134306197813512,
1.12856022069066));
#37578=CARTESIAN_POINT('Ctrl Pts',(-0.116428399613608,-0.126885604548101,
1.12807698662012));
#37579=CARTESIAN_POINT('Ctrl Pts',(-0.124852487683086,-0.118613771136687,
1.12759508954235));
#37580=CARTESIAN_POINT('Ctrl Pts',(-0.129034307879819,-0.114507532011624,
1.12735586994778));
#37581=CARTESIAN_POINT('Ctrl Pts',(-0.133021908645802,-0.110190752518543,
1.12711697982177));
#37582=CARTESIAN_POINT('Ctrl Pts',(-0.136799920681752,-0.105681293454548,
1.12687809715289));
#37583=CARTESIAN_POINT('Ctrl Pts',(-0.139913092404994,-0.101965391993263,
1.12668125215535));
#37584=CARTESIAN_POINT('Ctrl Pts',(-0.142886395744951,-0.0981144149624532,
1.12648421657965));
#37585=CARTESIAN_POINT('Ctrl Pts',(-0.145693560119959,-0.0941626751454851,
1.12628802354802));
#37586=CARTESIAN_POINT('Ctrl Pts',(-0.152880478586678,-0.0840454080131806,
1.12578572901386));
#37587=CARTESIAN_POINT('Ctrl Pts',(-0.15900482121196,-0.0732463252276768,
1.12528759909576));
#37588=CARTESIAN_POINT('Ctrl Pts',(-0.163934147646496,-0.0619414999212126,
1.12479074962784));
#37589=CARTESIAN_POINT('Ctrl Pts',(-0.166135734382546,-0.0568924219632783,
1.1245688415816));
#37590=CARTESIAN_POINT('Ctrl Pts',(-0.168098373685913,-0.0517419572379162,
1.12434718895784));
#37591=CARTESIAN_POINT('Ctrl Pts',(-0.169806974463718,-0.0465039785200352,
1.12412553479695));
#37592=CARTESIAN_POINT('Ctrl Pts',(-0.171302024805205,-0.0419206715400791,
1.12393158420695));
#37593=CARTESIAN_POINT('Ctrl Pts',(-0.172603159720904,-0.037265702966286,
1.12373744627196));
#37594=CARTESIAN_POINT('Ctrl Pts',(-0.173693332107248,-0.0325769359939504,
1.12354412603317));
#37595=CARTESIAN_POINT('Ctrl Pts',(-0.174146803491923,-0.0306265823819912,
1.12346371196521));
#37596=CARTESIAN_POINT('Ctrl Pts',(-0.174564098410947,-0.0286695573112724,
1.12338340400172));
#37597=CARTESIAN_POINT('Ctrl Pts',(-0.174944665354966,-0.0267065873422436,
1.12330319031487));
#37598=CARTESIAN_POINT('Ctrl Pts',(-0.176644787249262,-0.0179373332737037,
1.1229448485109));
#37599=CARTESIAN_POINT('Ctrl Pts',(-0.177613299278372,-0.00904985393428815,
1.12258838819752));
#37600=CARTESIAN_POINT('Ctrl Pts',(-0.177892626630995,-0.00012009523392913,
1.12223275485995));
#37601=CARTESIAN_POINT('',(0.188128289424299,-0.051655738433239,1.1046));
#37602=CARTESIAN_POINT('Ctrl Pts',(0.188079991776263,-0.0516378774142054,
1.1046));
#37603=CARTESIAN_POINT('Ctrl Pts',(0.189767230432996,-0.0390669740826218,
1.10628778184834));
#37604=CARTESIAN_POINT('Ctrl Pts',(0.190280594088308,-0.0264116239428061,
1.10798825493552));
#37605=CARTESIAN_POINT('Ctrl Pts',(0.189578785198131,-0.013858618669063,
1.10971174069725));
#37606=CARTESIAN_POINT('Ctrl Pts',(0.189002564675101,-0.00355196771938053,
1.11112680950153));
#37607=CARTESIAN_POINT('Ctrl Pts',(0.187606197243972,0.00668612269204304,
1.11255739169934));
#37608=CARTESIAN_POINT('Ctrl Pts',(0.185342457317502,0.0167394104911895,
1.1140092000994));
#37609=CARTESIAN_POINT('Ctrl Pts',(0.184551132811226,0.0202536891903846,
1.1145167016688));
#37610=CARTESIAN_POINT('Ctrl Pts',(0.183655673454389,0.0237360512197014,
1.1150254747949));
#37611=CARTESIAN_POINT('Ctrl Pts',(0.18265534113529,0.0271808706561584,
1.11553563926267));
#37612=CARTESIAN_POINT('Ctrl Pts',(0.18094879298457,0.0330576679230306,
1.11640597026411));
#37613=CARTESIAN_POINT('Ctrl Pts',(0.178936945382248,0.038826456249319,
1.11728051290445));
#37614=CARTESIAN_POINT('Ctrl Pts',(0.176612263817241,0.0444636415640588,
1.1181607012295));
#37615=CARTESIAN_POINT('Ctrl Pts',(0.172529449099474,0.0543641731105064,
1.11970656708142));
#37616=CARTESIAN_POINT('Ctrl Pts',(0.167482382247398,0.0638604192469179,
1.12126984735358));
#37617=CARTESIAN_POINT('Ctrl Pts',(0.161567727140847,0.0728508334626257,
1.12285831080443));
#37618=CARTESIAN_POINT('Ctrl Pts',(0.159791310571961,0.0755510282307451,
1.12333539234888));
#37619=CARTESIAN_POINT('Ctrl Pts',(0.157935831204718,0.07820633305328,1.12381491808146));
#37620=CARTESIAN_POINT('Ctrl Pts',(0.156005857937656,0.080810555607592,
1.12429655968642));
#37621=CARTESIAN_POINT('Ctrl Pts',(0.149084780910453,0.0901495579668382,
1.12602377461955));
#37622=CARTESIAN_POINT('Ctrl Pts',(0.141258220296783,0.0987686403112959,
1.12776582990404));
#37623=CARTESIAN_POINT('Ctrl Pts',(0.132662596065602,0.106547632773669,
1.12953438681126));
#37624=CARTESIAN_POINT('Ctrl Pts',(0.125865807878512,0.11269868854969,1.13093283169111));
#37625=CARTESIAN_POINT('Ctrl Pts',(0.11858709408701,0.11832389399092,1.13234784666969));
#37626=CARTESIAN_POINT('Ctrl Pts',(0.110887722236713,0.123341541992538,
1.13378519708595));
#37627=CARTESIAN_POINT('Ctrl Pts',(0.108018415924993,0.125211456754541,
1.13432085099405));
#37628=CARTESIAN_POINT('Ctrl Pts',(0.105090557092059,0.126996521585399,
1.13485961189033));
#37629=CARTESIAN_POINT('Ctrl Pts',(0.102119703918859,0.128685646974318,
1.13539959124502));
#37630=CARTESIAN_POINT('Ctrl Pts',(0.0927768272952827,0.133997686711853,
1.13709774332326));
#37631=CARTESIAN_POINT('Ctrl Pts',(0.082979544177925,0.138384526176108,
1.13881348137989));
#37632=CARTESIAN_POINT('Ctrl Pts',(0.0728343136972591,0.141721417442936,
1.14055808556308));
#37633=CARTESIAN_POINT('Ctrl Pts',(0.0653892612002304,0.144170186912073,
1.14183835906254));
#37634=CARTESIAN_POINT('Ctrl Pts',(0.0577564921504827,0.146052612758731,
1.14313417790127));
#37635=CARTESIAN_POINT('Ctrl Pts',(0.0499806597877626,0.147301514408983,
1.14445));
#37636=CARTESIAN_POINT('',(0.156060797133591,0.117265290216009,1.1046));
#37637=CARTESIAN_POINT('Origin',(0.,0.,1.1046));
#37638=CARTESIAN_POINT('Ctrl Pts',(-0.177892626630995,-0.00012009523392913,
1.12223275485995));
#37639=CARTESIAN_POINT('Ctrl Pts',(-0.178130827469488,0.00749489839273535,
1.12192948288029));
#37640=CARTESIAN_POINT('Ctrl Pts',(-0.177867516731744,0.0151409018269471,
1.12162681218094));
#37641=CARTESIAN_POINT('Ctrl Pts',(-0.177119648653777,0.022772046405986,
1.12132408898598));
#37642=CARTESIAN_POINT('Ctrl Pts',(-0.176683933562239,0.0272180241883703,
1.12114771955869));
#37643=CARTESIAN_POINT('Ctrl Pts',(-0.176082727329522,0.0316616978614784,
1.1209712215835));
#37644=CARTESIAN_POINT('Ctrl Pts',(-0.175323410854016,0.0360699258071878,
1.12079542245302));
#37645=CARTESIAN_POINT('Ctrl Pts',(-0.173218074679692,0.0482924997380182,
1.12030798897732));
#37646=CARTESIAN_POINT('Ctrl Pts',(-0.169899117173377,0.060280772698104,
1.11982442300823));
#37647=CARTESIAN_POINT('Ctrl Pts',(-0.165450405286176,0.0718434015054524,
1.11934209182814));
#37648=CARTESIAN_POINT('Ctrl Pts',(-0.163468469691568,0.0769946421750163,
1.11912720955245));
#37649=CARTESIAN_POINT('Ctrl Pts',(-0.161261595477516,0.0820613755489734,
1.11891257235417));
#37650=CARTESIAN_POINT('Ctrl Pts',(-0.158833971908418,0.0870258740589896,
1.11869794744021));
#37651=CARTESIAN_POINT('Ctrl Pts',(-0.157259648823123,0.0902453701582717,
1.11855876237008));
#37652=CARTESIAN_POINT('Ctrl Pts',(-0.155591255289476,0.0934239508703652,
1.11841948892714));
#37653=CARTESIAN_POINT('Ctrl Pts',(-0.153833447558489,0.0965496328988143,
1.11828037128997));
#37654=CARTESIAN_POINT('Ctrl Pts',(-0.14771977559034,0.10742078465325,1.11779651882779));
#37655=CARTESIAN_POINT('Ctrl Pts',(-0.140558745189236,0.117602653899592,
1.11731683957354));
#37656=CARTESIAN_POINT('Ctrl Pts',(-0.132418289468816,0.126903043139938,
1.11683877992991));
#37657=CARTESIAN_POINT('Ctrl Pts',(-0.12909688936255,0.130697709540948,
1.11664372606491));
#37658=CARTESIAN_POINT('Ctrl Pts',(-0.125611892721837,0.134345412680643,
1.11644894182206));
#37659=CARTESIAN_POINT('Ctrl Pts',(-0.121965775424868,0.137831740927343,
1.11625425375315));
#37660=CARTESIAN_POINT('Ctrl Pts',(-0.117995359394073,0.141628155697328,
1.11604224942997));
#37661=CARTESIAN_POINT('Ctrl Pts',(-0.113833879872902,0.145233242900832,
1.11583035914965));
#37662=CARTESIAN_POINT('Ctrl Pts',(-0.109497995542763,0.148643456469952,
1.11561835894421));
#37663=CARTESIAN_POINT('Ctrl Pts',(-0.106528819965926,0.150978740824945,
1.11547318306212));
#37664=CARTESIAN_POINT('Ctrl Pts',(-0.103484861618328,0.153216986140016,
1.11532830099587));
#37665=CARTESIAN_POINT('Ctrl Pts',(-0.100375391374892,0.155356036404444,
1.11518378070706));
#37666=CARTESIAN_POINT('Ctrl Pts',(-0.0901590665073864,0.162383996377836,
1.11470895184398));
#37667=CARTESIAN_POINT('Ctrl Pts',(-0.0792284020877703,0.168351899996775,
1.11423755053895));
#37668=CARTESIAN_POINT('Ctrl Pts',(-0.0677866372531476,0.173236468334987,
1.11376713654095));
#37669=CARTESIAN_POINT('Ctrl Pts',(-0.0629527485252524,0.175300088779209,
1.11356839718953));
#37670=CARTESIAN_POINT('Ctrl Pts',(-0.0580272205709242,0.1771698553942,
1.11336983405985));
#37671=CARTESIAN_POINT('Ctrl Pts',(-0.053024031320765,0.178841703955505,
1.11317126314023));
#37672=CARTESIAN_POINT('Ctrl Pts',(-0.0477983789695303,0.180587890023723,
1.11296386291187));
#37673=CARTESIAN_POINT('Ctrl Pts',(-0.0424815416125505,0.182119285098682,
1.11275621043829));
#37674=CARTESIAN_POINT('Ctrl Pts',(-0.0371242414709178,0.183422331662166,
1.11254943891139));
#37675=CARTESIAN_POINT('Ctrl Pts',(-0.024630778610864,0.18646109436267,
1.11206723848886));
#37676=CARTESIAN_POINT('Ctrl Pts',(-0.0118919597510465,0.188273325293319,
1.11158873863955));
#37677=CARTESIAN_POINT('Ctrl Pts',(0.000886208579909016,0.188815541438236,
1.11111139386139));
#37678=CARTESIAN_POINT('Ctrl Pts',(0.00944159770367764,0.189178572350712,
1.1107917963872));
#37679=CARTESIAN_POINT('Ctrl Pts',(0.018015230692156,0.18897135417352,1.11047271669991));
#37680=CARTESIAN_POINT('Ctrl Pts',(0.0265466554166013,0.188167601942836,
1.11015339081081));
#37681=CARTESIAN_POINT('Ctrl Pts',(0.0302389326862781,0.187819749598396,
1.11001519118297));
#37682=CARTESIAN_POINT('Ctrl Pts',(0.0339178177085591,0.187360375525866,
1.1098771490423));
#37683=CARTESIAN_POINT('Ctrl Pts',(0.0375710017615334,0.186789297951633,
1.1097394835104));
#37684=CARTESIAN_POINT('Ctrl Pts',(0.0423078408099154,0.186048819915471,
1.10956098183688));
#37685=CARTESIAN_POINT('Ctrl Pts',(0.0470053189021468,0.185120233668386,
1.10938296950455));
#37686=CARTESIAN_POINT('Ctrl Pts',(0.0516529562716852,0.184000805096474,
1.10920531719144));
#37687=CARTESIAN_POINT('Ctrl Pts',(0.0618028867738203,0.181556095816553,
1.10881734401536));
#37688=CARTESIAN_POINT('Ctrl Pts',(0.0717155486830652,0.178202889727245,
1.10843108790673));
#37689=CARTESIAN_POINT('Ctrl Pts',(0.0813183120370126,0.174031280266035,
1.10804520187417));
#37690=CARTESIAN_POINT('Ctrl Pts',(0.0859478038432918,0.172020147521446,
1.10785916623421));
#37691=CARTESIAN_POINT('Ctrl Pts',(0.0905051909798001,0.169818426512715,
1.10767321660747));
#37692=CARTESIAN_POINT('Ctrl Pts',(0.0949816305437677,0.167434340091183,
1.10748720206377));
#37693=CARTESIAN_POINT('Ctrl Pts',(0.0983118022353031,0.165660739219842,
1.10734881968224));
#37694=CARTESIAN_POINT('Ctrl Pts',(0.101597049834463,0.16378593049508,1.10721040073536));
#37695=CARTESIAN_POINT('Ctrl Pts',(0.104821419449008,0.161821258958598,
1.10707241581092));
#37696=CARTESIAN_POINT('Ctrl Pts',(0.116000559886905,0.155009589811987,
1.10659401133715));
#37697=CARTESIAN_POINT('Ctrl Pts',(0.126488220095427,0.147101893720343,
1.10611923196118));
#37698=CARTESIAN_POINT('Ctrl Pts',(0.136144216947772,0.138260857674004,
1.10564559537577));
#37699=CARTESIAN_POINT('Ctrl Pts',(0.143255609150872,0.131749663048667,
1.1052967742678));
#37700=CARTESIAN_POINT('Ctrl Pts',(0.149915772834495,0.124730943289562,
1.10494857300279));
#37701=CARTESIAN_POINT('Ctrl Pts',(0.156057659382849,0.117255425406029,
1.1046));
#37702=CARTESIAN_POINT('',(-0.0999999999999999,-1.22464679914735E-17,1.2));
#37703=CARTESIAN_POINT('',(-0.15,-1.83697019872103E-17,1.15));
#37704=CARTESIAN_POINT('Origin',(0.,0.,1.2));
#37705=CARTESIAN_POINT('Ctrl Pts',(0.113509973994371,-0.159049193030953,
-0.0230074082272069));
#37706=CARTESIAN_POINT('Ctrl Pts',(0.166385127640631,-0.121313337847033,
-0.019303686544359));
#37707=CARTESIAN_POINT('Ctrl Pts',(0.230633516687349,0.0103782615975306,
-0.0118962431786632));
#37708=CARTESIAN_POINT('Ctrl Pts',(0.116188988078006,0.199753850566951,
-0.000785078130119459));
#37709=CARTESIAN_POINT('Ctrl Pts',(-0.104655428901899,0.205782953697956,
0.0103260869184242));
#37710=CARTESIAN_POINT('Ctrl Pts',(-0.229698075471667,0.0238333788527267,
0.0214372519669679));
#37711=CARTESIAN_POINT('Ctrl Pts',(-0.144613108848303,-0.180075271725216,
0.0325484170155115));
#37712=CARTESIAN_POINT('Ctrl Pts',(0.0727946961077783,-0.219149774367173,
0.0436595820640553));
#37713=CARTESIAN_POINT('Ctrl Pts',(0.22359411788162,-0.057762978583554,
0.0547707471125989));
#37714=CARTESIAN_POINT('Ctrl Pts',(0.169827668332871,0.156494259322429,
0.0658819121611427));
#37715=CARTESIAN_POINT('Ctrl Pts',(-0.0393188016825179,0.227560800163251,
0.0769930772096863));
#37716=CARTESIAN_POINT('Ctrl Pts',(-0.212490816724285,0.090434536960108,
0.0881042422582301));
#37717=CARTESIAN_POINT('Ctrl Pts',(-0.19125222930514,-0.129434912039326,
0.0992154073067737));
#37718=CARTESIAN_POINT('Ctrl Pts',(0.00496630258143332,-0.230880650358359,
0.110326572355317));
#37719=CARTESIAN_POINT('Ctrl Pts',(0.196640931676781,-0.121090966106477,
0.121437737403861));
#37720=CARTESIAN_POINT('Ctrl Pts',(0.208405785032279,0.0994871990457256,
0.132548902452405));
#37721=CARTESIAN_POINT('Ctrl Pts',(0.0294968904732024,0.229042728261432,
0.143660067500948));
#37722=CARTESIAN_POINT('Ctrl Pts',(-0.176399147035948,0.149043619583305,
0.154771232549492));
#37723=CARTESIAN_POINT('Ctrl Pts',(-0.220904863824581,-0.0673178902258552,
0.165882397598036));
#37724=CARTESIAN_POINT('Ctrl Pts',(-0.0633012670336293,-0.222089176195486,
0.17699356264658));
#37725=CARTESIAN_POINT('Ctrl Pts',(0.152217643594786,-0.173667627565877,
0.188104727695123));
#37726=CARTESIAN_POINT('Ctrl Pts',(0.228470258285089,0.0336451535954383,
0.199215892743667));
#37727=CARTESIAN_POINT('Ctrl Pts',(0.0956918672404541,0.210175453516431,
0.210327057792211));
#37728=CARTESIAN_POINT('Ctrl Pts',(-0.124636506047609,0.194412953698174,
0.221438222840754));
#37729=CARTESIAN_POINT('Ctrl Pts',(-0.230932995110325,0.000779007092406014,
0.232549387889298));
#37730=CARTESIAN_POINT('Ctrl Pts',(-0.12594528285163,-0.193567664513544,
0.243660552937842));
#37731=CARTESIAN_POINT('Ctrl Pts',(0.0942717341349318,-0.21081625941051,
0.254771717986386));
#37732=CARTESIAN_POINT('Ctrl Pts',(0.228238070382781,-0.0351857683462,0.265882883034929));
#37733=CARTESIAN_POINT('Ctrl Pts',(0.153385834111148,0.172636731182735,
0.276994048083473));
#37734=CARTESIAN_POINT('Ctrl Pts',(-0.0618014955343493,0.222511191222357,
0.288105213132016));
#37735=CARTESIAN_POINT('Ctrl Pts',(-0.220445672440028,0.068806689849701,
0.299216378180561));
#37736=CARTESIAN_POINT('Ctrl Pts',(-0.177400663329184,-0.147850125855229,
0.310327543229104));
#37737=CARTESIAN_POINT('Ctrl Pts',(0.0279509811935462,-0.229236554058792,
0.321438708277648));
#37738=CARTESIAN_POINT('Ctrl Pts',(0.207729836817097,-0.100890881459812,
0.332549873326191));
#37739=CARTESIAN_POINT('Ctrl Pts',(0.197453422882556,0.11976143309821,0.343661038374735));
#37740=CARTESIAN_POINT('Ctrl Pts',(0.00652379087403971,0.230842143506323,
0.354772203423278));
#37741=CARTESIAN_POINT('Ctrl Pts',(-0.190374559216213,0.130721774273047,
0.365883368471823));
#37742=CARTESIAN_POINT('Ctrl Pts',(-0.213096254074054,-0.0889979863001003,
0.376994533520366));
#37743=CARTESIAN_POINT('Ctrl Pts',(-0.0408528604769679,-0.227292100295502,
0.38810569856891));
#37744=CARTESIAN_POINT('Ctrl Pts',(0.16876745272456,-0.15763312458598,0.399216863617453));
#37745=CARTESIAN_POINT('Ctrl Pts',(0.223979789625721,0.0562468568463683,
0.410328028665997));
#37746=CARTESIAN_POINT('Ctrl Pts',(0.0742695215461042,0.218665711155622,
0.421439193714541));
#37747=CARTESIAN_POINT('Ctrl Pts',(-0.143391090854028,0.181023893808443,
0.432550358763085));
#37748=CARTESIAN_POINT('Ctrl Pts',(-0.229860956455329,-0.0222395090620434,
0.443661523811628));
#37749=CARTESIAN_POINT('Ctrl Pts',(-0.106027445761331,-0.205155638019547,
0.454772688860172));
#37750=CARTESIAN_POINT('Ctrl Pts',(0.114812229735204,-0.200371672072451,
0.465883853908716));
#37751=CARTESIAN_POINT('Ctrl Pts',(0.230608404475241,-0.0122645363248325,
0.476995018957259));
#37752=CARTESIAN_POINT('Ctrl Pts',(0.135417351061808,0.187063615108022,
0.488106184005803));
#37753=CARTESIAN_POINT('Ctrl Pts',(-0.083669150175529,0.21524434574405,
0.499217349054346));
#37754=CARTESIAN_POINT('Ctrl Pts',(-0.226205440167697,0.0464946653328952,
0.510328514102891));
#37755=CARTESIAN_POINT('Ctrl Pts',(-0.161782842764492,-0.164793709991974,
0.521439679151433));
#37756=CARTESIAN_POINT('Ctrl Pts',(0.0506574022840452,-0.225309748257175,
0.532550844199978));
#37757=CARTESIAN_POINT('Ctrl Pts',(0.21675039941815,-0.0796863816342033,
0.543662009248521));
#37758=CARTESIAN_POINT('Ctrl Pts',(0.184535073495005,0.138843299139974,
0.554773174297065));
#37759=CARTESIAN_POINT('Ctrl Pts',(-0.01651427104253,0.230343078727826,
0.565884339345609));
#37760=CARTESIAN_POINT('Ctrl Pts',(-0.2024544512798,0.11109838082922,0.576995504394152));
#37761=CARTESIAN_POINT('Ctrl Pts',(-0.203165894515671,-0.109791959503082,
0.588106669442697));
#37762=CARTESIAN_POINT('Ctrl Pts',(-0.0179976902307884,-0.230231922661119,
0.599217834491239));
#37763=CARTESIAN_POINT('Ctrl Pts',(0.183636881720094,-0.140029106752845,
0.610328999539785));
#37764=CARTESIAN_POINT('Ctrl Pts',(0.217259204728728,0.0782885242326115,
0.621440164588326));
#37765=CARTESIAN_POINT('Ctrl Pts',(0.0521076907609949,0.224978762618687,
0.632551329636872));
#37766=CARTESIAN_POINT('Ctrl Pts',(-0.160717962682088,0.16583242004264,
0.643662494685413));
#37767=CARTESIAN_POINT('Ctrl Pts',(-0.226500243885858,-0.0450365916286509,
0.65477365973396));
#37768=CARTESIAN_POINT('Ctrl Pts',(-0.0850539171717745,-0.214700922773088,
0.665884824782501));
#37769=CARTESIAN_POINT('Ctrl Pts',(0.134209565723166,-0.187932029027199,
0.676995989831046));
#37770=CARTESIAN_POINT('Ctrl Pts',(0.230682622449346,0.0107788109627418,
0.68810715487959));
#37771=CARTESIAN_POINT('Ctrl Pts',(0.116100547839306,0.199627948587589,
0.699218319928133));
#37772=CARTESIAN_POINT('Ctrl Pts',(-0.104703729866326,0.205834360634882,
0.710329484976677));
#37773=CARTESIAN_POINT('Ctrl Pts',(-0.229712931099768,0.0237197038645086,
0.721440650025221));
#37774=CARTESIAN_POINT('Ctrl Pts',(-0.144554186745893,-0.180096480143545,
0.732551815073763));
#37775=CARTESIAN_POINT('Ctrl Pts',(0.072859438989827,-0.219139583863915,
0.743662980122308));
#37776=CARTESIAN_POINT('Ctrl Pts',(0.223612826941383,-0.0576884623911715,
0.75477414517085));
#37777=CARTESIAN_POINT('Ctrl Pts',(0.16977934979946,0.156542733614398,0.765885310219396));
#37778=CARTESIAN_POINT('Ctrl Pts',(-0.0393879040694563,0.227550539615811,
0.776996475267938));
#37779=CARTESIAN_POINT('Ctrl Pts',(-0.212518549811472,0.0903688057410859,
0.788107640316484));
#37780=CARTESIAN_POINT('Ctrl Pts',(-0.191212657747833,-0.129492758803799,
0.799218805365025));
#37781=CARTESIAN_POINT('Ctrl Pts',(0.00503667898133586,-0.230879377455661,
0.81032997041357));
#37782=CARTESIAN_POINT('Ctrl Pts',(0.196677879493939,-0.121030850518371,
0.821441135462113));
#37783=CARTESIAN_POINT('Ctrl Pts',(0.208375418707704,0.0995506903268707,
0.832552300510658));
#37784=CARTESIAN_POINT('Ctrl Pts',(0.0294270353677539,0.229051751091564,
0.8436634655592));
#37785=CARTESIAN_POINT('Ctrl Pts',(-0.176444601777748,0.14898978999011,
0.854774630607746));
#37786=CARTESIAN_POINT('Ctrl Pts',(-0.22088431932234,-0.0673852547682493,
0.865885795656288));
#37787=CARTESIAN_POINT('Ctrl Pts',(-0.0632335256349382,-0.22210847899434,
0.876996960704833));
#37788=CARTESIAN_POINT('Ctrl Pts',(0.152270606837662,-0.173621188252162,
0.888108125753376));
#37789=CARTESIAN_POINT('Ctrl Pts',(0.228459985995541,0.0337148347205355,
0.899219290801919));
#37790=CARTESIAN_POINT('Ctrl Pts',(0.0956277562497704,0.210204633917866,
0.910330455850463));
#37791=CARTESIAN_POINT('Ctrl Pts',(-0.12469579560031,0.194374924182257,
0.921441620899007));
#37792=CARTESIAN_POINT('Ctrl Pts',(-0.230933226540692,0.000708579792413808,
0.932552785947551));
#37793=CARTESIAN_POINT('Ctrl Pts',(-0.125886228368054,-0.193606087509586,
0.943663950996094));
#37794=CARTESIAN_POINT('Ctrl Pts',(0.0943360139257667,-0.210787462610152,
0.954775116044639));
#37795=CARTESIAN_POINT('Ctrl Pts',(0.228248823506631,-0.0351162152961091,
0.965886281093181));
#37796=CARTESIAN_POINT('Ctrl Pts',(0.153333110744206,0.172683627576032,
0.976997446141726));
#37797=CARTESIAN_POINT('Ctrl Pts',(-0.0618692454411617,0.222492101746939,
0.988108611190268));
#37798=CARTESIAN_POINT('Ctrl Pts',(-0.220466868021367,0.0687398848825245,
0.999219776238814));
#37799=CARTESIAN_POINT('Ctrl Pts',(-0.17735514221838,-0.147905058047522,
1.01033094128735));
#37800=CARTESIAN_POINT('Ctrl Pts',(0.0280201048116106,-0.229226437530741,
1.0214421063359));
#37801=CARTESIAN_POINT('Ctrl Pts',(0.207762111854432,-0.10083052618152,
1.03255327138444));
#37802=CARTESIAN_POINT('Ctrl Pts',(0.197414006873683,0.119827380577986,
1.04366443643299));
#37803=CARTESIAN_POINT('Ctrl Pts',(0.00645886152005097,0.230833217918201,
1.05477560148153));
#37804=CARTESIAN_POINT('Ctrl Pts',(-0.190424854748374,0.130684465150768,
1.06588676653008));
#37805=CARTESIAN_POINT('Ctrl Pts',(-0.213049227679005,-0.0891025387309722,
1.07699793157862));
#37806=CARTESIAN_POINT('Ctrl Pts',(-0.0408214485225542,-0.227228942196666,
1.08810909662716));
#37807=CARTESIAN_POINT('Ctrl Pts',(0.168888461736298,-0.15772814986318,
1.09922026167571));
#37808=CARTESIAN_POINT('Ctrl Pts',(0.223817187934597,0.0566161966084782,
1.11033142672425));
#37809=CARTESIAN_POINT('Ctrl Pts',(0.124300218570944,0.164165746435707,
1.11773887008995));
#37810=CARTESIAN_POINT('Ctrl Pts',(0.0627850911123727,0.1850383536838,1.12144259177279));
#37811=CARTESIAN_POINT('Ctrl Pts',(0.105793541951254,-0.14823699524473,
-0.0153382721514713));
#37812=CARTESIAN_POINT('Ctrl Pts',(0.155074231467859,-0.113066431478549,
-0.0116345504686234));
#37813=CARTESIAN_POINT('Ctrl Pts',(0.214955001436596,0.00967274517879857,
-0.00422710710292769));
#37814=CARTESIAN_POINT('Ctrl Pts',(0.108290436090784,0.186174541551099,
0.00688405794561606));
#37815=CARTESIAN_POINT('Ctrl Pts',(-0.0975409307071879,0.191793784975909,
0.0179952229941597));
#37816=CARTESIAN_POINT('Ctrl Pts',(-0.214083151712633,0.022213180716797,
0.0291063880427034));
#37817=CARTESIAN_POINT('Ctrl Pts',(-0.134782279118508,-0.167833716661673,
0.0402175530912472));
#37818=CARTESIAN_POINT('Ctrl Pts',(0.0678460972679723,-0.204251926348524,
0.0513287181397908));
#37819=CARTESIAN_POINT('Ctrl Pts',(0.208394142450739,-0.0538362390807298,
0.0624398831883346));
#37820=CARTESIAN_POINT('Ctrl Pts',(0.158282747515632,0.145855746470163,
0.0735510482368781));
#37821=CARTESIAN_POINT('Ctrl Pts',(-0.0366459012269607,0.212091168831785,
0.084662213285422));
#37822=CARTESIAN_POINT('Ctrl Pts',(-0.198045646054783,0.0842867780077688,
0.0957733783339656));
#37823=CARTESIAN_POINT('Ctrl Pts',(-0.178250862301028,-0.120635899339281,
0.106884543382509));
#37824=CARTESIAN_POINT('Ctrl Pts',(0.00462869228141735,-0.215185334908375,
0.117995708431053));
#37825=CARTESIAN_POINT('Ctrl Pts',(0.183273239545565,-0.112859176615955,
0.129106873479597));
#37826=CARTESIAN_POINT('Ctrl Pts',(0.194238315681312,0.0927240382098824,
0.14021803852814));
#37827=CARTESIAN_POINT('Ctrl Pts',(0.0274916856192995,0.213472355144377,
0.151329203576684));
#37828=CARTESIAN_POINT('Ctrl Pts',(-0.164407495706399,0.138911602796551,
0.162440368625228));
#37829=CARTESIAN_POINT('Ctrl Pts',(-0.20588770445336,-0.062741605808422,
0.173551533673771));
#37830=CARTESIAN_POINT('Ctrl Pts',(-0.0589980335104445,-0.206991507018771,
0.184662698722315));
#37831=CARTESIAN_POINT('Ctrl Pts',(0.141869855984326,-0.161861665507704,
0.195773863770859));
#37832=CARTESIAN_POINT('Ctrl Pts',(0.21293880179812,0.0313579489369987,
0.206885028819403));
#37833=CARTESIAN_POINT('Ctrl Pts',(0.0891867138635642,0.195887681727571,
0.217996193867946));
#37834=CARTESIAN_POINT('Ctrl Pts',(-0.116163690001897,0.18119671998123,
0.22910735891649));
#37835=CARTESIAN_POINT('Ctrl Pts',(-0.21523412125303,0.00072605002547781,
0.240218523965033));
#37836=CARTESIAN_POINT('Ctrl Pts',(-0.11738349588193,-0.180408893734178,
0.251329689013577));
#37837=CARTESIAN_POINT('Ctrl Pts',(0.0878631217069615,-0.196484925501419,
0.262440854062121));
#37838=CARTESIAN_POINT('Ctrl Pts',(0.212722398078527,-0.0327938323711113,
0.273552019110664));
#37839=CARTESIAN_POINT('Ctrl Pts',(0.142958632662274,0.160900849678758,
0.284663184159209));
#37840=CARTESIAN_POINT('Ctrl Pts',(-0.057600216794938,0.207384833374845,
0.295774349207752));
#37841=CARTESIAN_POINT('Ctrl Pts',(-0.205459728996263,0.0641291965189069,
0.306885514256296));
#37842=CARTESIAN_POINT('Ctrl Pts',(-0.165340928710165,-0.137799243024573,
0.317996679304839));
#37843=CARTESIAN_POINT('Ctrl Pts',(0.0260508675794864,-0.213653004623031,
0.329107844353384));
#37844=CARTESIAN_POINT('Ctrl Pts',(0.193608318568785,-0.0940322979965331,
0.340219009401926));
#37845=CARTESIAN_POINT('Ctrl Pts',(0.184030497427301,0.111620025542831,
0.351330174450471));
#37846=CARTESIAN_POINT('Ctrl Pts',(0.00608030219043116,0.215149445760286,
0.362441339499014));
#37847=CARTESIAN_POINT('Ctrl Pts',(-0.177432856410404,0.121835280406139,
0.373552504547559));
#37848=CARTESIAN_POINT('Ctrl Pts',(-0.198609925645444,-0.0829478843655077,
0.384663669596101));
#37849=CARTESIAN_POINT('Ctrl Pts',(-0.0380756743800589,-0.211840735237885,
0.395774834644646));
#37850=CARTESIAN_POINT('Ctrl Pts',(0.157294605588646,-0.14691719143219,
0.406885999693188));
#37851=CARTESIAN_POINT('Ctrl Pts',(0.208753596148093,0.0524231836199493,
0.417997164741733));
#37852=CARTESIAN_POINT('Ctrl Pts',(0.0692206637610257,0.203800769856489,
0.429108329790276));
#37853=CARTESIAN_POINT('Ctrl Pts',(-0.133643334165982,0.168717851215016,
0.44021949483882));
#37854=CARTESIAN_POINT('Ctrl Pts',(-0.21423496001257,-0.0207276625316418,
0.451330659887364));
#37855=CARTESIAN_POINT('Ctrl Pts',(-0.0988196775702872,-0.191209114350017,
0.462441824935908));
#37856=CARTESIAN_POINT('Ctrl Pts',(0.107007270071357,-0.186750363419964,
0.473552989984451));
#37857=CARTESIAN_POINT('Ctrl Pts',(0.21493159635798,-0.011430790551128,
0.484664155032995));
#37858=CARTESIAN_POINT('Ctrl Pts',(0.126211650891535,0.174346990983058,
0.495775320081538));
#37859=CARTESIAN_POINT('Ctrl Pts',(-0.0779813036479037,0.200611989589323,
0.506886485130082));
#37860=CARTESIAN_POINT('Ctrl Pts',(-0.21082794649543,0.0433339481484583,
0.517997650178626));
#37861=CARTESIAN_POINT('Ctrl Pts',(-0.150784810891129,-0.153590998727594,
0.529108815227169));
#37862=CARTESIAN_POINT('Ctrl Pts',(0.0472137013611209,-0.209993143910453,
0.540219980275713));
#37863=CARTESIAN_POINT('Ctrl Pts',(0.202015661416081,-0.0742692845544967,
0.551331145324257));
#37864=CARTESIAN_POINT('Ctrl Pts',(0.171990340163759,0.129404702294652,
0.562442310372801));
#37865=CARTESIAN_POINT('Ctrl Pts',(-0.0153916274037652,0.214684307510999,
0.573553475421344));
#37866=CARTESIAN_POINT('Ctrl Pts',(-0.188691554856225,0.103545889399597,
0.584664640469888));
#37867=CARTESIAN_POINT('Ctrl Pts',(-0.189354634030427,-0.102328278871562,
0.595775805518432));
#37868=CARTESIAN_POINT('Ctrl Pts',(-0.0167742034418123,-0.21458070785722,
0.606886970566975));
#37869=CARTESIAN_POINT('Ctrl Pts',(0.171153207655705,-0.130509898455162,
0.61799813561552));
#37870=CARTESIAN_POINT('Ctrl Pts',(0.202489878034016,0.0729664537947597,
0.629109300664062));
#37871=CARTESIAN_POINT('Ctrl Pts',(0.0485653989206222,0.209684658745684,
0.640220465712607));
#37872=CARTESIAN_POINT('Ctrl Pts',(-0.149792321581985,0.154559097049293,
0.65133163076115));
#37873=CARTESIAN_POINT('Ctrl Pts',(-0.211102709394471,-0.041974994603061,
0.662442795809694));
#37874=CARTESIAN_POINT('Ctrl Pts',(-0.079271933890819,-0.20010550862688,
0.673553960858237));
#37875=CARTESIAN_POINT('Ctrl Pts',(0.125085971055702,-0.17515636994031,
0.684665125906781));
#37876=CARTESIAN_POINT('Ctrl Pts',(0.215000768978506,0.0100460651134341,
0.695776290955325));
#37877=CARTESIAN_POINT('Ctrl Pts',(0.108208008038219,0.186057198414926,
0.706887456003868));
#37878=CARTESIAN_POINT('Ctrl Pts',(-0.0975859481618359,0.191841697258389,
0.717998621052413));
#37879=CARTESIAN_POINT('Ctrl Pts',(-0.214096997451993,0.0221072333783236,
0.729109786100956));
#37880=CARTESIAN_POINT('Ctrl Pts',(-0.134727362553083,-0.167853483327237,
0.7402209511495));
#37881=CARTESIAN_POINT('Ctrl Pts',(0.0679064389152043,-0.204242428597833,
0.751332116198043));
#37882=CARTESIAN_POINT('Ctrl Pts',(0.208411579664662,-0.0537667885148679,
0.762443281246587));
#37883=CARTESIAN_POINT('Ctrl Pts',(0.158237713686343,0.14590092546951,0.773554446295131));
#37884=CARTESIAN_POINT('Ctrl Pts',(-0.0367103060190181,0.21208160579853,
0.784665611343674));
#37885=CARTESIAN_POINT('Ctrl Pts',(-0.198071493840836,0.0842255152109201,
0.795776776392219));
#37886=CARTESIAN_POINT('Ctrl Pts',(-0.178213980826558,-0.120689813668469,
0.80688794144076));
#37887=CARTESIAN_POINT('Ctrl Pts',(0.00469428447876819,-0.215184148537872,
0.817999106489307));
#37888=CARTESIAN_POINT('Ctrl Pts',(0.183307675642296,-0.112803147698245,
0.829110271537848));
#37889=CARTESIAN_POINT('Ctrl Pts',(0.194210013665906,0.0927832133403047,
0.840221436586394));
#37890=CARTESIAN_POINT('Ctrl Pts',(0.0274265792786954,0.213480764600607,
0.851332601634936));
#37891=CARTESIAN_POINT('Ctrl Pts',(-0.164449860425235,0.138861432550488,
0.86244376668348));
#37892=CARTESIAN_POINT('Ctrl Pts',(-0.205868556570727,-0.0628043908949741,
0.873554931732024));
#37893=CARTESIAN_POINT('Ctrl Pts',(-0.0589348971863656,-0.207009497609277,
0.884666096780567));
#37894=CARTESIAN_POINT('Ctrl Pts',(0.141919218774748,-0.161818383148359,
0.895777261829112));
#37895=CARTESIAN_POINT('Ctrl Pts',(0.212929227820989,0.0314228931244718,
0.906888426877654));
#37896=CARTESIAN_POINT('Ctrl Pts',(0.0891269611515884,0.195914878439144,
0.9179995919262));
#37897=CARTESIAN_POINT('Ctrl Pts',(-0.116218949038264,0.181161275719849,
0.929110756974741));
#37898=CARTESIAN_POINT('Ctrl Pts',(-0.215234336950711,0.000660410388236847,
0.940221922023287));
#37899=CARTESIAN_POINT('Ctrl Pts',(-0.117328455934639,-0.180444704726821,
0.951333087071829));
#37900=CARTESIAN_POINT('Ctrl Pts',(0.0879230317440182,-0.196458086313641,
0.962444252120374));
#37901=CARTESIAN_POINT('Ctrl Pts',(0.212732420202743,-0.0327290075520782,
0.973555417168917));
#37902=CARTESIAN_POINT('Ctrl Pts',(0.142909493440969,0.160944558045319,
0.98466658221746));
#37903=CARTESIAN_POINT('Ctrl Pts',(-0.0576633610487541,0.207367041606005,
0.995777747266004));
#37904=CARTESIAN_POINT('Ctrl Pts',(-0.205479483697499,0.0640669329675303,
1.00688891231455));
#37905=CARTESIAN_POINT('Ctrl Pts',(-0.165298502134104,-0.137850440914814,
1.01800007736309));
#37906=CARTESIAN_POINT('Ctrl Pts',(0.026115292159373,-0.213643575818697,
1.02911124241164));
#37907=CARTESIAN_POINT('Ctrl Pts',(0.193638399542254,-0.0939760456828254,
1.04022240746018));
#37908=CARTESIAN_POINT('Ctrl Pts',(0.183993760927049,0.111681489898982,
1.05133357250872));
#37909=CARTESIAN_POINT('Ctrl Pts',(0.00601978674766102,0.215141126935532,
1.06244473755726));
#37910=CARTESIAN_POINT('Ctrl Pts',(-0.177479732841649,0.121800507565884,
1.07355590260581));
#37911=CARTESIAN_POINT('Ctrl Pts',(-0.198566096114678,-0.0830453293000129,
1.08466706765435));
#37912=CARTESIAN_POINT('Ctrl Pts',(-0.0380463978169507,-0.211781870639967,
1.0957782327029));
#37913=CARTESIAN_POINT('Ctrl Pts',(0.157407388382168,-0.147005756870945,
1.10688939775144));
#37914=CARTESIAN_POINT('Ctrl Pts',(0.208602048154327,0.0527674155869038,
1.11800056279999));
#37915=CARTESIAN_POINT('Ctrl Pts',(0.115850263419028,0.153005724266717,
1.12540800616568));
#37916=CARTESIAN_POINT('Ctrl Pts',(0.0585169473375027,0.172459407258861,
1.12911172784853));
#37917=CARTESIAN_POINT('Ctrl Pts',(0.0980771099081375,-0.137424797458507,
-0.00766913607573581));
#37918=CARTESIAN_POINT('Ctrl Pts',(0.143763335295088,-0.104819525110066,
-0.00396541439288791));
#37919=CARTESIAN_POINT('Ctrl Pts',(0.199276486185844,0.0089672287600667,
0.00344202897280782));
#37920=CARTESIAN_POINT('Ctrl Pts',(0.100391884103562,0.172595232535247,
0.0145531940213516));
#37921=CARTESIAN_POINT('Ctrl Pts',(-0.0904264325124765,0.177804616253862,
0.0256643590698952));
#37922=CARTESIAN_POINT('Ctrl Pts',(-0.198468227953599,0.020592982580867,
0.036775524118439));
#37923=CARTESIAN_POINT('Ctrl Pts',(-0.124951449388714,-0.155592161598129,
0.0478866891669827));
#37924=CARTESIAN_POINT('Ctrl Pts',(0.0628974984281669,-0.189354078329874,
0.0589978542155263));
#37925=CARTESIAN_POINT('Ctrl Pts',(0.193194167019859,-0.0499094995779056,
0.07010901926407));
#37926=CARTESIAN_POINT('Ctrl Pts',(0.146737826698393,0.135217233617898,
0.0812201843126137));
#37927=CARTESIAN_POINT('Ctrl Pts',(-0.0339730007714042,0.196621537500318,
0.0923313493611574));
#37928=CARTESIAN_POINT('Ctrl Pts',(-0.18360047538528,0.07813901905543,0.103442514409701));
#37929=CARTESIAN_POINT('Ctrl Pts',(-0.165249495296916,-0.111836886639236,
0.114553679458245));
#37930=CARTESIAN_POINT('Ctrl Pts',(0.00429108198140191,-0.199490019458391,
0.125664844506789));
#37931=CARTESIAN_POINT('Ctrl Pts',(0.169905547414348,-0.104627387125433,
0.136776009555332));
#37932=CARTESIAN_POINT('Ctrl Pts',(0.180070846330345,0.0859608773740392,
0.147887174603876));
#37933=CARTESIAN_POINT('Ctrl Pts',(0.0254864807653961,0.197901982027321,
0.15899833965242));
#37934=CARTESIAN_POINT('Ctrl Pts',(-0.152415844376849,0.128779586009797,
0.170109504700963));
#37935=CARTESIAN_POINT('Ctrl Pts',(-0.190870545082139,-0.0581653213909888,
0.181220669749507));
#37936=CARTESIAN_POINT('Ctrl Pts',(-0.0546947999872595,-0.191893837842057,
0.192331834798051));
#37937=CARTESIAN_POINT('Ctrl Pts',(0.131522068373867,-0.150055703449532,
0.203442999846594));
#37938=CARTESIAN_POINT('Ctrl Pts',(0.197407345311151,0.0290707442785592,
0.214554164895138));
#37939=CARTESIAN_POINT('Ctrl Pts',(0.0826815604866742,0.181599909938712,
0.225665329943681));
#37940=CARTESIAN_POINT('Ctrl Pts',(-0.107690873956185,0.167980486264285,
0.236776494992226));
#37941=CARTESIAN_POINT('Ctrl Pts',(-0.199535247395734,0.000673092958549589,
0.247887660040769));
#37942=CARTESIAN_POINT('Ctrl Pts',(-0.10882170891223,-0.167250122954812,
0.258998825089313));
#37943=CARTESIAN_POINT('Ctrl Pts',(0.0814545092789914,-0.182153591592328,
0.270109990137857));
#37944=CARTESIAN_POINT('Ctrl Pts',(0.197206725774273,-0.0304018963960226,
0.2812211551864));
#37945=CARTESIAN_POINT('Ctrl Pts',(0.1325314312134,0.149164968174781,0.292332320234944));
#37946=CARTESIAN_POINT('Ctrl Pts',(-0.0533989380555266,0.192258475527334,
0.303443485283487));
#37947=CARTESIAN_POINT('Ctrl Pts',(-0.190473785552499,0.0594517031881129,
0.314554650332031));
#37948=CARTESIAN_POINT('Ctrl Pts',(-0.153281194091147,-0.127748360193918,
0.325665815380575));
#37949=CARTESIAN_POINT('Ctrl Pts',(0.0241507539654265,-0.198069455187271,
0.336776980429119));
#37950=CARTESIAN_POINT('Ctrl Pts',(0.179486800320472,-0.0871737145332536,
0.347888145477662));
#37951=CARTESIAN_POINT('Ctrl Pts',(0.170607571972046,0.103478617987453,
0.358999310526206));
#37952=CARTESIAN_POINT('Ctrl Pts',(0.00563681350682242,0.199456748014249,
0.37011047557475));
#37953=CARTESIAN_POINT('Ctrl Pts',(-0.164491153604594,0.11294878653923,
0.381221640623293));
#37954=CARTESIAN_POINT('Ctrl Pts',(-0.184123597216834,-0.0768977824309152,
0.392332805671837));
#37955=CARTESIAN_POINT('Ctrl Pts',(-0.0352984882831497,-0.196389370180267,
0.403443970720381));
#37956=CARTESIAN_POINT('Ctrl Pts',(0.145821758452731,-0.136201258278399,
0.414555135768924));
#37957=CARTESIAN_POINT('Ctrl Pts',(0.193527402670466,0.0485995103935303,
0.425666300817468));
#37958=CARTESIAN_POINT('Ctrl Pts',(0.0641718059759468,0.188935828557357,
0.436777465866012));
#37959=CARTESIAN_POINT('Ctrl Pts',(-0.123895577477937,0.156411808621589,
0.447888630914555));
#37960=CARTESIAN_POINT('Ctrl Pts',(-0.198608963569812,-0.01921581600124,
0.458999795963099));
#37961=CARTESIAN_POINT('Ctrl Pts',(-0.0916119093792434,-0.177262590680487,
0.470110961011643));
#37962=CARTESIAN_POINT('Ctrl Pts',(0.0992023104075105,-0.173129054767478,
0.481222126060186));
#37963=CARTESIAN_POINT('Ctrl Pts',(0.199254788240719,-0.0105970447774237,
0.49233329110873));
#37964=CARTESIAN_POINT('Ctrl Pts',(0.117005950721263,0.161630366858093,
0.503444456157274));
#37965=CARTESIAN_POINT('Ctrl Pts',(-0.0722934571202785,0.185979633434597,
0.514555621205818));
#37966=CARTESIAN_POINT('Ctrl Pts',(-0.195450452823164,0.0401732309640217,
0.525666786254361));
#37967=CARTESIAN_POINT('Ctrl Pts',(-0.139786779017765,-0.142388287463214,
0.536777951302905));
#37968=CARTESIAN_POINT('Ctrl Pts',(0.0437700004381964,-0.19467653956373,
0.547889116351449));
#37969=CARTESIAN_POINT('Ctrl Pts',(0.187280923414012,-0.0688521874747905,
0.559000281399993));
#37970=CARTESIAN_POINT('Ctrl Pts',(0.159445606832513,0.119966105449332,
0.570111446448536));
#37971=CARTESIAN_POINT('Ctrl Pts',(-0.0142689837650004,0.199025536294172,
0.581222611497081));
#37972=CARTESIAN_POINT('Ctrl Pts',(-0.174928658432651,0.0959933979699734,
0.592333776545623));
#37973=CARTESIAN_POINT('Ctrl Pts',(-0.175543373545183,-0.0948645982400418,
0.603444941594168));
#37974=CARTESIAN_POINT('Ctrl Pts',(-0.0155507166528361,-0.198929493053321,
0.61455610664271));
#37975=CARTESIAN_POINT('Ctrl Pts',(0.158669533591315,-0.120990690157479,
0.625667271691256));
#37976=CARTESIAN_POINT('Ctrl Pts',(0.187720551339304,0.0676443833569079,
0.636778436739797));
#37977=CARTESIAN_POINT('Ctrl Pts',(0.0450231070802491,0.194390554872681,
0.647889601788343));
#37978=CARTESIAN_POINT('Ctrl Pts',(-0.138866680481881,0.143285774055946,
0.659000766836885));
#37979=CARTESIAN_POINT('Ctrl Pts',(-0.195705174903083,-0.038913397577471,
0.67011193188543));
#37980=CARTESIAN_POINT('Ctrl Pts',(-0.0734899506098636,-0.185510094480672,
0.681223096933973));
#37981=CARTESIAN_POINT('Ctrl Pts',(0.115962376388238,-0.162380710853421,
0.692334261982516));
#37982=CARTESIAN_POINT('Ctrl Pts',(0.199318915507666,0.00931331926412601,
0.703445427031061));
#37983=CARTESIAN_POINT('Ctrl Pts',(0.100315468237132,0.172486448242263,
0.714556592079604));
#37984=CARTESIAN_POINT('Ctrl Pts',(-0.0904681664573454,0.177849033881895,
0.725667757128148));
#37985=CARTESIAN_POINT('Ctrl Pts',(-0.198481063804218,0.0204947628921387,
0.736778922176691));
#37986=CARTESIAN_POINT('Ctrl Pts',(-0.124900538360275,-0.155610486510929,
0.747890087225236));
#37987=CARTESIAN_POINT('Ctrl Pts',(0.0629534388405818,-0.189345273331751,
0.759001252273779));
#37988=CARTESIAN_POINT('Ctrl Pts',(0.193210332387941,-0.0498451146385645,
0.770112417322323));
#37989=CARTESIAN_POINT('Ctrl Pts',(0.146696077573226,0.135259117324623,
0.781223582370866));
#37990=CARTESIAN_POINT('Ctrl Pts',(-0.0340327079685797,0.196612671981249,
0.79233474741941));
#37991=CARTESIAN_POINT('Ctrl Pts',(-0.1836244378702,0.0780822246807544,
0.803445912467955));
#37992=CARTESIAN_POINT('Ctrl Pts',(-0.165215303905282,-0.111886868533138,
0.814557077516496));
#37993=CARTESIAN_POINT('Ctrl Pts',(0.00435188997620014,-0.199488919620082,
0.825668242565042));
#37994=CARTESIAN_POINT('Ctrl Pts',(0.169937471790653,-0.104575444878119,
0.836779407613584));
#37995=CARTESIAN_POINT('Ctrl Pts',(0.180044608624107,0.0860157363537389,
0.847890572662129));
#37996=CARTESIAN_POINT('Ctrl Pts',(0.0254261231896373,0.197909778109651,
0.859001737710672));
#37997=CARTESIAN_POINT('Ctrl Pts',(-0.152455119072723,0.128733075110866,
0.870112902759215));
#37998=CARTESIAN_POINT('Ctrl Pts',(-0.190852793819114,-0.058223527021699,
0.88122406780776));
#37999=CARTESIAN_POINT('Ctrl Pts',(-0.0546362687377931,-0.191910516224214,
0.892335232856302));
#38000=CARTESIAN_POINT('Ctrl Pts',(0.131567830711834,-0.150015578044556,
0.903446397904849));
#38001=CARTESIAN_POINT('Ctrl Pts',(0.197398469646436,0.0291309515284085,
0.914557562953389));
#38002=CARTESIAN_POINT('Ctrl Pts',(0.0826261660534066,0.181625122960423,
0.925668728001935));
#38003=CARTESIAN_POINT('Ctrl Pts',(-0.107742102476217,0.167947627257441,
0.936779893050478));
#38004=CARTESIAN_POINT('Ctrl Pts',(-0.199535447360731,0.000612240984059651,
0.947891058099021));
#38005=CARTESIAN_POINT('Ctrl Pts',(-0.108770683501224,-0.167283321944057,
0.959002223147566));
#38006=CARTESIAN_POINT('Ctrl Pts',(0.0815100495622697,-0.182128710017129,
0.970113388196108));
#38007=CARTESIAN_POINT('Ctrl Pts',(0.197216016898856,-0.0303417998080474,
0.981224553244654));
#38008=CARTESIAN_POINT('Ctrl Pts',(0.132485876137733,0.149205488514605,
0.992335718293196));
#38009=CARTESIAN_POINT('Ctrl Pts',(-0.0534574766563464,0.19224198146507,
1.00344688334174));
#38010=CARTESIAN_POINT('Ctrl Pts',(-0.190492099373632,0.0593939810525364,
1.01455804839028));
#38011=CARTESIAN_POINT('Ctrl Pts',(-0.153241862049827,-0.127795823782107,
1.02566921343883));
#38012=CARTESIAN_POINT('Ctrl Pts',(0.0242104795071353,-0.198060714106653,
1.03678037848737));
#38013=CARTESIAN_POINT('Ctrl Pts',(0.179514687230076,-0.0871215651841315,
1.04789154353591));
#38014=CARTESIAN_POINT('Ctrl Pts',(0.170573514980415,0.103535599219979,
1.05900270858446));
#38015=CARTESIAN_POINT('Ctrl Pts',(0.0055807119752709,0.199449035952863,
1.070113873633));
#38016=CARTESIAN_POINT('Ctrl Pts',(-0.164534610934924,0.112916549981001,
1.08122503868155));
#38017=CARTESIAN_POINT('Ctrl Pts',(-0.184082964550351,-0.0769881198690536,
1.09233620373009));
#38018=CARTESIAN_POINT('Ctrl Pts',(-0.0352713471113472,-0.196334799083268,
1.10344736877863));
#38019=CARTESIAN_POINT('Ctrl Pts',(0.145926315028038,-0.136283363878709,
1.11455853382718));
#38020=CARTESIAN_POINT('Ctrl Pts',(0.193386908374058,0.0489186345653294,
1.12566969887572));
#38021=CARTESIAN_POINT('Ctrl Pts',(0.107400308267113,0.141845702097726,
1.13307714224142));
#38022=CARTESIAN_POINT('Ctrl Pts',(0.0542488035626326,0.159880460833922,
1.13678086392426));
#38023=CARTESIAN_POINT('Ctrl Pts',(0.0903606778650208,-0.126612599672284,
-2.77555756156289E-16));
#38024=CARTESIAN_POINT('Ctrl Pts',(0.132452439122316,-0.0965726187415828,
0.00370372168284762));
#38025=CARTESIAN_POINT('Ctrl Pts',(0.183597970935092,0.00826171234133487,
0.0111111650485434));
#38026=CARTESIAN_POINT('Ctrl Pts',(0.0924933321163406,0.159015923519395,
0.0222223300970871));
#38027=CARTESIAN_POINT('Ctrl Pts',(-0.0833119343177651,0.163815447531815,
0.0333334951456308));
#38028=CARTESIAN_POINT('Ctrl Pts',(-0.182853304194564,0.018972784444937,
0.0444446601941745));
#38029=CARTESIAN_POINT('Ctrl Pts',(-0.115120619658919,-0.143350606534586,
0.0555558252427182));
#38030=CARTESIAN_POINT('Ctrl Pts',(0.0579488995883613,-0.174456230311225,
0.0666669902912619));
#38031=CARTESIAN_POINT('Ctrl Pts',(0.177994191588978,-0.0459827600750814,
0.0777781553398056));
#38032=CARTESIAN_POINT('Ctrl Pts',(0.135192905881154,0.124578720765632,
0.0888893203883492));
#38033=CARTESIAN_POINT('Ctrl Pts',(-0.0313001003158473,0.181151906168851,
0.100000485436893));
#38034=CARTESIAN_POINT('Ctrl Pts',(-0.169155304715778,0.0719912601030908,
0.111111650485437));
#38035=CARTESIAN_POINT('Ctrl Pts',(-0.152248128292804,-0.103037873939191,
0.12222281553398));
#38036=CARTESIAN_POINT('Ctrl Pts',(0.00395347168138628,-0.183794704008407,
0.133333980582524));
#38037=CARTESIAN_POINT('Ctrl Pts',(0.156537855283131,-0.0963955976349113,
0.144445145631068));
#38038=CARTESIAN_POINT('Ctrl Pts',(0.165903376979378,0.0791977165381959,
0.155556310679611));
#38039=CARTESIAN_POINT('Ctrl Pts',(0.0234812759114929,0.182331608910266,
0.166667475728155));
#38040=CARTESIAN_POINT('Ctrl Pts',(-0.1404241930473,0.118647569223042,0.177778640776699));
#38041=CARTESIAN_POINT('Ctrl Pts',(-0.175853385710917,-0.0535890369735552,
0.188889805825242));
#38042=CARTESIAN_POINT('Ctrl Pts',(-0.0503915664640746,-0.176796168665343,
0.200000970873786));
#38043=CARTESIAN_POINT('Ctrl Pts',(0.121174280763407,-0.138249741391359,
0.21111213592233));
#38044=CARTESIAN_POINT('Ctrl Pts',(0.181875888824183,0.0267835396201195,
0.222223300970874));
#38045=CARTESIAN_POINT('Ctrl Pts',(0.0761764071097843,0.167312138149853,
0.233334466019417));
#38046=CARTESIAN_POINT('Ctrl Pts',(-0.0992180579104728,0.154764252547341,
0.244445631067961));
#38047=CARTESIAN_POINT('Ctrl Pts',(-0.183836373538439,0.000620135891621234,
0.255556796116504));
#38048=CARTESIAN_POINT('Ctrl Pts',(-0.10025992194253,-0.154091352175446,
0.266667961165049));
#38049=CARTESIAN_POINT('Ctrl Pts',(0.0750458968510211,-0.167822257683237,
0.277779126213592));
#38050=CARTESIAN_POINT('Ctrl Pts',(0.181691053470019,-0.0280099604209337,
0.288890291262136));
#38051=CARTESIAN_POINT('Ctrl Pts',(0.122104229764526,0.137429086670804,
0.30000145631068));
#38052=CARTESIAN_POINT('Ctrl Pts',(-0.0491976593161155,0.177132117679823,
0.311112621359223));
#38053=CARTESIAN_POINT('Ctrl Pts',(-0.175487842108734,0.0547742098573187,
0.322223786407767));
#38054=CARTESIAN_POINT('Ctrl Pts',(-0.141221459472129,-0.117697477363263,
0.33333495145631));
#38055=CARTESIAN_POINT('Ctrl Pts',(0.0222506403513669,-0.18248590575151,
0.344446116504855));
#38056=CARTESIAN_POINT('Ctrl Pts',(0.165365282072159,-0.0803151310699741,
0.355557281553397));
#38057=CARTESIAN_POINT('Ctrl Pts',(0.157184646516792,0.0953372104320743,
0.366668446601942));
#38058=CARTESIAN_POINT('Ctrl Pts',(0.00519332482321354,0.183764050268212,
0.377779611650485));
#38059=CARTESIAN_POINT('Ctrl Pts',(-0.151549450798785,0.104062292672322,
0.388890776699029));
#38060=CARTESIAN_POINT('Ctrl Pts',(-0.169637268788223,-0.0708476804963227,
0.400001941747572));
#38061=CARTESIAN_POINT('Ctrl Pts',(-0.0325213021862407,-0.180938005122649,
0.411113106796117));
#38062=CARTESIAN_POINT('Ctrl Pts',(0.134348911316817,-0.125485325124609,
0.42222427184466));
#38063=CARTESIAN_POINT('Ctrl Pts',(0.178301209192838,0.0447758371671112,
0.433335436893204));
#38064=CARTESIAN_POINT('Ctrl Pts',(0.0591229481908682,0.174070887258225,
0.444446601941748));
#38065=CARTESIAN_POINT('Ctrl Pts',(-0.114147820789891,0.144105766028162,
0.455557766990291));
#38066=CARTESIAN_POINT('Ctrl Pts',(-0.182982967127054,-0.0177039694708382,
0.466668932038835));
#38067=CARTESIAN_POINT('Ctrl Pts',(-0.0844041411881997,-0.163316067010957,
0.477780097087378));
#38068=CARTESIAN_POINT('Ctrl Pts',(0.0913973507436636,-0.159507746114991,
0.488891262135923));
#38069=CARTESIAN_POINT('Ctrl Pts',(0.183577980123458,-0.00976329900371924,
0.500002427184466));
#38070=CARTESIAN_POINT('Ctrl Pts',(0.10780025055099,0.148913742733129,0.51111359223301));
#38071=CARTESIAN_POINT('Ctrl Pts',(-0.0666056105926533,0.17134727727987,
0.522224757281553));
#38072=CARTESIAN_POINT('Ctrl Pts',(-0.180072959150898,0.037012513779585,
0.533335922330097));
#38073=CARTESIAN_POINT('Ctrl Pts',(-0.128788747144402,-0.131185576198834,
0.544447087378641));
#38074=CARTESIAN_POINT('Ctrl Pts',(0.0403262995152723,-0.179359935217008,
0.555558252427184));
#38075=CARTESIAN_POINT('Ctrl Pts',(0.172546185411942,-0.0634350903950841,
0.566669417475728));
#38076=CARTESIAN_POINT('Ctrl Pts',(0.146900873501267,0.11052750860401,0.577780582524271));
#38077=CARTESIAN_POINT('Ctrl Pts',(-0.013146340126236,0.183366765077345,
0.588891747572816));
#38078=CARTESIAN_POINT('Ctrl Pts',(-0.161165762009075,0.0884409065403499,
0.600002912621358));
#38079=CARTESIAN_POINT('Ctrl Pts',(-0.16173211305994,-0.087400917608522,
0.611114077669903));
#38080=CARTESIAN_POINT('Ctrl Pts',(-0.0143272298638598,-0.183278278249422,
0.622225242718446));
#38081=CARTESIAN_POINT('Ctrl Pts',(0.146185859526926,-0.111471481859797,
0.63333640776699));
#38082=CARTESIAN_POINT('Ctrl Pts',(0.172951224644592,0.0623223129190563,
0.644447572815534));
#38083=CARTESIAN_POINT('Ctrl Pts',(0.0414808152398764,0.179096450999678,
0.655558737864077));
#38084=CARTESIAN_POINT('Ctrl Pts',(-0.127941039381778,0.1320124510626,0.666669902912621));
#38085=CARTESIAN_POINT('Ctrl Pts',(-0.180307640411694,-0.0358518005518811,
0.677781067961165));
#38086=CARTESIAN_POINT('Ctrl Pts',(-0.0677079673289082,-0.170914680334463,
0.68889223300971));
#38087=CARTESIAN_POINT('Ctrl Pts',(0.106838781720774,-0.149605051766532,
0.700003398058251));
#38088=CARTESIAN_POINT('Ctrl Pts',(0.183637062036826,0.00858057341481814,
0.711114563106797));
#38089=CARTESIAN_POINT('Ctrl Pts',(0.0924229284360449,0.1589156980696,0.722225728155339));
#38090=CARTESIAN_POINT('Ctrl Pts',(-0.0833503847528551,0.163856370505402,
0.733336893203883));
#38091=CARTESIAN_POINT('Ctrl Pts',(-0.182865130156443,0.0188822924059537,
0.744448058252428));
#38092=CARTESIAN_POINT('Ctrl Pts',(-0.115073714167466,-0.143367489694622,
0.75555922330097));
#38093=CARTESIAN_POINT('Ctrl Pts',(0.0580004387659595,-0.174448118065669,
0.766670388349515));
#38094=CARTESIAN_POINT('Ctrl Pts',(0.17800908511122,-0.0459234407622611,
0.777781553398057));
#38095=CARTESIAN_POINT('Ctrl Pts',(0.135154441460109,0.124617309179735,
0.788892718446602));
#38096=CARTESIAN_POINT('Ctrl Pts',(-0.0313551099181417,0.181143738163968,
0.800003883495145));
#38097=CARTESIAN_POINT('Ctrl Pts',(-0.169177381899564,0.0719389341505889,
0.81111504854369));
#38098=CARTESIAN_POINT('Ctrl Pts',(-0.152216626984007,-0.103083923397808,
0.822226213592232));
#38099=CARTESIAN_POINT('Ctrl Pts',(0.00400949547363229,-0.183793690702293,
0.833337378640777));
#38100=CARTESIAN_POINT('Ctrl Pts',(0.156567267939011,-0.0963477420579929,
0.844448543689319));
#38101=CARTESIAN_POINT('Ctrl Pts',(0.165879203582308,0.0792482593671729,
0.855559708737864));
#38102=CARTESIAN_POINT('Ctrl Pts',(0.0234256671005791,0.182338791618694,
0.866670873786407));
#38103=CARTESIAN_POINT('Ctrl Pts',(-0.140460377720211,0.118604717671243,
0.877782038834952));
#38104=CARTESIAN_POINT('Ctrl Pts',(-0.175837031067501,-0.0536426631484242,
0.888893203883495));
#38105=CARTESIAN_POINT('Ctrl Pts',(-0.0503376402892206,-0.17681153483915,
0.900004368932038));
#38106=CARTESIAN_POINT('Ctrl Pts',(0.12121644264892,-0.138212772940753,
0.911115533980582));
#38107=CARTESIAN_POINT('Ctrl Pts',(0.181867711471885,0.026839009932345,
0.922226699029127));
#38108=CARTESIAN_POINT('Ctrl Pts',(0.0761253709552246,0.167335367481701,
0.933337864077668));
#38109=CARTESIAN_POINT('Ctrl Pts',(-0.099265255914171,0.154733978795034,
0.944449029126215));
#38110=CARTESIAN_POINT('Ctrl Pts',(-0.18383655777075,0.000564071579882353,
0.955560194174756));
#38111=CARTESIAN_POINT('Ctrl Pts',(-0.100212911067809,-0.154121939161292,
0.966671359223301));
#38112=CARTESIAN_POINT('Ctrl Pts',(0.0750970673805211,-0.167799333720618,
0.977782524271844));
#38113=CARTESIAN_POINT('Ctrl Pts',(0.181699613594968,-0.0279545920640164,
0.988893689320389));
#38114=CARTESIAN_POINT('Ctrl Pts',(0.122062258834496,0.137466418983892,
1.00000485436893));
#38115=CARTESIAN_POINT('Ctrl Pts',(-0.0492515922639386,0.177116921324136,
1.01111601941748));
#38116=CARTESIAN_POINT('Ctrl Pts',(-0.175504715049764,0.0547210291375423,
1.02222718446602));
#38117=CARTESIAN_POINT('Ctrl Pts',(-0.14118522196555,-0.1177412066494,1.03333834951456));
#38118=CARTESIAN_POINT('Ctrl Pts',(0.0223056668548975,-0.182477852394609,
1.04444951456311));
#38119=CARTESIAN_POINT('Ctrl Pts',(0.165390974917898,-0.0802670846854376,
1.05556067961165));
#38120=CARTESIAN_POINT('Ctrl Pts',(0.157153269033781,0.0953897085409752,
1.06667184466019));
#38121=CARTESIAN_POINT('Ctrl Pts',(0.00514163720288116,0.183756944970195,
1.07778300970874));
#38122=CARTESIAN_POINT('Ctrl Pts',(-0.151589489028199,0.104032592396117,
1.08889417475728));
#38123=CARTESIAN_POINT('Ctrl Pts',(-0.169599832986023,-0.0709309104380943,
1.10000533980583));
#38124=CARTESIAN_POINT('Ctrl Pts',(-0.0324962964057439,-0.180887727526569,
1.11111650485437));
#38125=CARTESIAN_POINT('Ctrl Pts',(0.134445241673909,-0.125560970886474,
1.12222766990291));
#38126=CARTESIAN_POINT('Ctrl Pts',(0.178171768593789,0.0450698535437549,
1.13333883495146));
#38127=CARTESIAN_POINT('Ctrl Pts',(0.0989503531151977,0.130685679928735,
1.14074627831715));
#38128=CARTESIAN_POINT('Ctrl Pts',(0.0499806597877626,0.147301514408983,
1.14445));
#38129=CARTESIAN_POINT('',(0.0903606778650206,-0.126612599672284,0.));
#38130=CARTESIAN_POINT('Ctrl Pts',(0.0903606778650208,-0.126612599672284,
-2.77555756156289E-16));
#38131=CARTESIAN_POINT('Ctrl Pts',(0.132452439122316,-0.0965726187415828,
0.00370372168284762));
#38132=CARTESIAN_POINT('Ctrl Pts',(0.183597970935092,0.00826171234133487,
0.0111111650485434));
#38133=CARTESIAN_POINT('Ctrl Pts',(0.0924933321163406,0.159015923519395,
0.0222223300970871));
#38134=CARTESIAN_POINT('Ctrl Pts',(-0.0833119343177651,0.163815447531815,
0.0333334951456308));
#38135=CARTESIAN_POINT('Ctrl Pts',(-0.15310616378989,0.0622578531632503,
0.0411241775931451));
#38136=CARTESIAN_POINT('Ctrl Pts',(-0.155772922446558,0.00543356393242454,
0.0452111383578116));
#38137=CARTESIAN_POINT('Ctrl Pts',(-0.155735926886437,0.000101346774827265,
0.0455943774396301));
#38138=CARTESIAN_POINT('Ctrl Pts',(0.0863567639152676,0.175641488315944,
2.2659825404947E-17));
#38139=CARTESIAN_POINT('Ctrl Pts',(0.0902605506355985,0.173244147111074,
2.45989142876686E-17));
#38140=CARTESIAN_POINT('Ctrl Pts',(0.0940681517855526,0.170703362163956,
1.50959816364938E-17));
#38141=CARTESIAN_POINT('Ctrl Pts',(0.0977705169885396,0.168018661523996,
1.10588621593521E-17));
#38142=CARTESIAN_POINT('Ctrl Pts',(0.104919852250204,0.162834455239647,
2.72100915479622E-18));
#38143=CARTESIAN_POINT('Ctrl Pts',(0.111677400716997,0.157113958337607,
-2.16691070983975E-17));
#38144=CARTESIAN_POINT('Ctrl Pts',(0.118012246833275,0.150919901422416,
-3.33934269125535E-17));
#38145=CARTESIAN_POINT('Ctrl Pts',(0.122832506482077,0.146206769948873,
-4.2314601108814E-17));
#38146=CARTESIAN_POINT('Ctrl Pts',(0.127411584310215,0.141213843322959,
-4.34283416288416E-17));
#38147=CARTESIAN_POINT('Ctrl Pts',(0.131710542479305,0.135995360136636,
-4.0766001685455E-17));
#38148=CARTESIAN_POINT('Ctrl Pts',(0.136227531634889,0.130512210258439,
-3.79686353981478E-17));
#38149=CARTESIAN_POINT('Ctrl Pts',(0.140440157604184,0.124776412163605,
1.15313389293564E-17));
#38150=CARTESIAN_POINT('Ctrl Pts',(0.144331170139148,0.11882042578862,3.72965547335014E-17));
#38151=CARTESIAN_POINT('Ctrl Pts',(0.147802837134673,0.113506333084464,
6.02849796064744E-17));
#38152=CARTESIAN_POINT('Ctrl Pts',(0.15101843405387,0.108016870008689,-1.53625880027527E-18));
#38153=CARTESIAN_POINT('Ctrl Pts',(0.153962315598392,0.102374391558266,
-8.67361737988404E-18));
#38154=CARTESIAN_POINT('Ctrl Pts',(0.15571005357274,0.0990245373918854,
-1.29109592829026E-17));
#38155=CARTESIAN_POINT('Ctrl Pts',(0.157357576324963,0.0956291376942575,
-3.44593994380303E-18));
#38156=CARTESIAN_POINT('Ctrl Pts',(0.158902506880511,0.0921936740973187,
-6.07153216591882E-18));
#38157=CARTESIAN_POINT('Ctrl Pts',(0.163908283820673,0.0810623229886477,
-1.45787941606636E-17));
#38158=CARTESIAN_POINT('Ctrl Pts',(0.167841697827597,0.0695089356622268,
-9.75260753403157E-18));
#38159=CARTESIAN_POINT('Ctrl Pts',(0.170598119604662,0.0576980955231356,
-5.20417042793042E-18));
#38160=CARTESIAN_POINT('Ctrl Pts',(0.171984491688748,0.0517577059954232,
-2.91648489207139E-18));
#38161=CARTESIAN_POINT('Ctrl Pts',(0.173072324320188,0.0457521241966622,
1.08654590748341E-17));
#38162=CARTESIAN_POINT('Ctrl Pts',(0.173843127025583,0.0397030009933723,
1.73472347597681E-17));
#38163=CARTESIAN_POINT('Ctrl Pts',(0.174324086814962,0.0359285136940646,
2.13916853648473E-17));
#38164=CARTESIAN_POINT('Ctrl Pts',(0.17468129632341,0.0321360477424029,
-3.73379012875618E-17));
#38165=CARTESIAN_POINT('Ctrl Pts',(0.174909438673913,0.0283479136595781,
-3.46944695195361E-17));
#38166=CARTESIAN_POINT('Ctrl Pts',(0.175317247780942,0.0215765466853118,
-2.99692812919358E-17));
#38167=CARTESIAN_POINT('Ctrl Pts',(0.175315000224248,0.0148063200599795,
-5.50593613673983E-17));
#38168=CARTESIAN_POINT('Ctrl Pts',(0.174882170147482,0.00806701752180915,
-4.68375338513738E-17));
#38169=CARTESIAN_POINT('Ctrl Pts',(0.174454769721774,0.00141225638482493,
-4.0453568795602E-17));
#38170=CARTESIAN_POINT('Ctrl Pts',(0.173607423807277,-0.00521244743448051,
5.53912001912299E-18));
#38171=CARTESIAN_POINT('Ctrl Pts',(0.172357876958299,-0.0117762500451153,
6.93889390390723E-18));
#38172=CARTESIAN_POINT('Ctrl Pts',(0.171266545977134,-0.0175089531839406,
8.16143038450564E-18));
#38173=CARTESIAN_POINT('Ctrl Pts',(0.169868307866471,-0.0231952127882146,
5.24172218001205E-19));
#38174=CARTESIAN_POINT('Ctrl Pts',(0.168172344307035,-0.0288124942050995,
-3.46944695195361E-18));
#38175=CARTESIAN_POINT('Ctrl Pts',(0.167269600009596,-0.0318025164482014,
-5.59521015704244E-18));
#38176=CARTESIAN_POINT('Ctrl Pts',(0.166282932031305,-0.0347708579305845,
-1.1797187803688E-17));
#38177=CARTESIAN_POINT('Ctrl Pts',(0.165217237950495,-0.0377059593473793,
-8.67361737988404E-18));
#38178=CARTESIAN_POINT('Ctrl Pts',(0.161836480623691,-0.047017135789496,
1.23544919580411E-18));
#38179=CARTESIAN_POINT('Ctrl Pts',(0.157654897120342,-0.0560198074489911,
-1.7088045241211E-17));
#38180=CARTESIAN_POINT('Ctrl Pts',(0.152731837788828,-0.0646106508942882,
1.38777878078145E-17));
#38181=CARTESIAN_POINT('Ctrl Pts',(0.14995806869425,-0.0694509370741418,
3.13246770113308E-17));
#38182=CARTESIAN_POINT('Ctrl Pts',(0.146948492244732,-0.074160201986225,
-2.50126624213863E-18));
#38183=CARTESIAN_POINT('Ctrl Pts',(0.143711118647294,-0.0787168991005189,
3.46944695195361E-18));
#38184=CARTESIAN_POINT('Ctrl Pts',(0.141667380230334,-0.0815935201226661,
7.2387295398745E-18));
#38185=CARTESIAN_POINT('Ctrl Pts',(0.139532823645962,-0.0844092886780934,
1.73900611772481E-17));
#38186=CARTESIAN_POINT('Ctrl Pts',(0.137309196652862,-0.08715819230643,
2.08166817117217E-17));
#38187=CARTESIAN_POINT('Ctrl Pts',(0.135173374337891,-0.0897985495827733,
2.41079947894884E-17));
#38188=CARTESIAN_POINT('Ctrl Pts',(0.132961417486925,-0.0923697150592745,
-3.29131307776674E-18));
#38189=CARTESIAN_POINT('Ctrl Pts',(0.130676581353388,-0.0948665968574491,
0.));
#38190=CARTESIAN_POINT('Ctrl Pts',(0.123427275316167,-0.10278867933332,
1.04426463739872E-17));
#38191=CARTESIAN_POINT('Ctrl Pts',(0.115443266551879,-0.109969536302748,
2.37276977285196E-17));
#38192=CARTESIAN_POINT('Ctrl Pts',(0.106786977446893,-0.116251471062968,
2.77555756156289E-17));
#38193=CARTESIAN_POINT('Ctrl Pts',(0.101553949468808,-0.120049119218897,
3.01905679570255E-17));
#38194=CARTESIAN_POINT('Ctrl Pts',(0.0960747579407472,-0.123517461158967,
2.18989005301202E-17));
#38195=CARTESIAN_POINT('Ctrl Pts',(0.0903606778650241,-0.126612599672281,
2.08166817117217E-17));
#38196=CARTESIAN_POINT('Ctrl Pts',(0.188079991776263,-0.0516378774142081,
1.1046));
#38197=CARTESIAN_POINT('Ctrl Pts',(0.179754570390634,-0.0821182550519846,
1.1028067538919));
#38198=CARTESIAN_POINT('Ctrl Pts',(0.164446793279769,-0.110682480125595,
1.1010135077838));
#38199=CARTESIAN_POINT('Ctrl Pts',(0.143091597726206,-0.133587557506818,
1.09922026167571));
#38200=CARTESIAN_POINT('Ctrl Pts',(0.0989851583166799,-0.180895080641009,
1.09551653999286));
#38201=CARTESIAN_POINT('Ctrl Pts',(0.0290818548970629,-0.204062011418838,
1.09181281831001));
#38202=CARTESIAN_POINT('Ctrl Pts',(-0.0345744266721549,-0.19262440956347,
1.08810909662716));
#38203=CARTESIAN_POINT('Ctrl Pts',(-0.0982307082413709,-0.181186807708102,
1.08440537494431));
#38204=CARTESIAN_POINT('Ctrl Pts',(-0.155639967960188,-0.135144673219537,
1.08070165326147));
#38205=CARTESIAN_POINT('Ctrl Pts',(-0.180573868997825,-0.0754924386616321,
1.07699793157862));
#38206=CARTESIAN_POINT('Ctrl Pts',(-0.190472245868201,-0.0518114150655666,
1.07552761078989));
#38207=CARTESIAN_POINT('Ctrl Pts',(-0.195252608806662,-0.0259854826956367,
1.07405729000116));
#38208=CARTESIAN_POINT('Ctrl Pts',(-0.195129684289216,-0.000113636086278679,
1.07258696921242));
#38209=CARTESIAN_POINT('Origin',(0.,0.,-0.129405622560369));
#38210=CARTESIAN_POINT('',(-0.0903606778650173,-0.126612599672286,0.));
#38211=CARTESIAN_POINT('Ctrl Pts',(-0.0905549614304886,-0.126792015305981,
1.24276674021151E-16));
#38212=CARTESIAN_POINT('Ctrl Pts',(-0.0513706458239086,-0.154472437079514,
0.00344950590738082));
#38213=CARTESIAN_POINT('Ctrl Pts',(0.0587535178885047,-0.172169358136003,
0.0106052258091336));
#38214=CARTESIAN_POINT('Ctrl Pts',(0.177508460417327,-0.0479721809770191,
0.0214671597052585));
#38215=CARTESIAN_POINT('Ctrl Pts',(0.13650560094313,0.123222299189869,0.0325858016883748));
#38216=CARTESIAN_POINT('Ctrl Pts',(-0.0295638381403906,0.181478253869214,
0.043704443671491));
#38217=CARTESIAN_POINT('Ctrl Pts',(-0.141307745535963,0.0946781319192958,
0.0526443839621562));
#38218=CARTESIAN_POINT('Ctrl Pts',(-0.155414936746312,0.0214718667413076,
0.0578781102584494));
#38219=CARTESIAN_POINT('Ctrl Pts',(-0.155326046963413,7.29270061605551E-5,
0.0594056225603705));
#38220=CARTESIAN_POINT('Origin',(0.,0.,0.));
#38221=CARTESIAN_POINT('Ctrl Pts',(-0.0685825729128748,0.139614588036674,
-0.0230074082272066));
#38222=CARTESIAN_POINT('Ctrl Pts',(-0.115028016933624,0.116799292759742,
-0.0193011942328345));
#38223=CARTESIAN_POINT('Ctrl Pts',(-0.182555218707277,0.0215691441263552,
-0.0118887662440903));
#38224=CARTESIAN_POINT('Ctrl Pts',(-0.116942936218886,-0.142059634545264,
-0.000770124260974049));
#38225=CARTESIAN_POINT('Ctrl Pts',(0.0559468948314244,-0.175104601534012,
0.0103485177221422));
#38226=CARTESIAN_POINT('Ctrl Pts',(0.177508460417327,-0.0479721809770191,
0.0214671597052585));
#38227=CARTESIAN_POINT('Ctrl Pts',(0.13650560094313,0.123222299189869,0.0325858016883748));
#38228=CARTESIAN_POINT('Ctrl Pts',(-0.0295638381403906,0.181478253869214,
0.043704443671491));
#38229=CARTESIAN_POINT('Ctrl Pts',(-0.168540213790592,0.0735245708832444,
0.0548230856546073));
#38230=CARTESIAN_POINT('Ctrl Pts',(-0.153132379752993,-0.101797781965797,
0.0659417276377235));
#38231=CARTESIAN_POINT('Ctrl Pts',(0.00255447675030308,-0.183860034663711,
0.0770603696208398));
#38232=CARTESIAN_POINT('Ctrl Pts',(0.155899683301632,-0.0975032021788082,
0.0881790116039561));
#38233=CARTESIAN_POINT('Ctrl Pts',(0.166434877052597,0.0781732535368643,
0.0992976535870723));
#38234=CARTESIAN_POINT('Ctrl Pts',(0.0245080507541896,0.182238325373942,
0.110416295570189));
#38235=CARTESIAN_POINT('Ctrl Pts',(-0.139868975820189,0.119365863723167,
0.121534937553305));
#38236=CARTESIAN_POINT('Ctrl Pts',(-0.176120077222934,-0.0528512641939849,
0.132653579536421));
#38237=CARTESIAN_POINT('Ctrl Pts',(-0.0510374815939226,-0.176654153931159,
0.143772221519537));
#38238=CARTESIAN_POINT('Ctrl Pts',(0.120797626960931,-0.138634273102519,
0.154890863502654));
#38239=CARTESIAN_POINT('Ctrl Pts',(0.181976886629041,0.0263806680570579,
0.16600950548577));
#38240=CARTESIAN_POINT('Ctrl Pts',(0.0764574137846417,0.167229745635935,
0.177128147468886));
#38241=CARTESIAN_POINT('Ctrl Pts',(-0.0991003621173195,0.154889135395602,
0.188246789452002));
#38242=CARTESIAN_POINT('Ctrl Pts',(-0.183877909581896,0.000663349951290586,
0.199365431435119));
#38243=CARTESIAN_POINT('Ctrl Pts',(-0.100215313155719,-0.154170088892816,
0.210484073418235));
#38244=CARTESIAN_POINT('Ctrl Pts',(0.0752488571272716,-0.167777039880966,
0.221602715401351));
#38245=CARTESIAN_POINT('Ctrl Pts',(0.181781810074028,-0.0276929424335053,
0.232721357384467));
#38246=CARTESIAN_POINT('Ctrl Pts',(0.121794738393109,0.137759091140133,
0.243839999367584));
#38247=CARTESIAN_POINT('Ctrl Pts',(-0.0497615974795104,0.177017821004958,
0.2549586413507));
#38248=CARTESIAN_POINT('Ctrl Pts',(-0.175734151264734,0.0541205469518692,
0.266077283333817));
#38249=CARTESIAN_POINT('Ctrl Pts',(-0.140726598433086,-0.11835349598584,
0.277195925316932));
#38250=CARTESIAN_POINT('Ctrl Pts',(0.0231926238140432,-0.182410602009977,
0.288314567300049));
#38251=CARTESIAN_POINT('Ctrl Pts',(0.165866396469461,-0.0793716828903688,
0.299433209283165));
#38252=CARTESIAN_POINT('Ctrl Pts',(0.156599354026699,0.096375141196464,
0.310551851266282));
#38253=CARTESIAN_POINT('Ctrl Pts',(0.00388050940998321,0.183838154825996,
0.321670493249398));
#38254=CARTESIAN_POINT('Ctrl Pts',(-0.152393050178991,0.102897443019027,
0.332789135232514));
#38255=CARTESIAN_POINT('Ctrl Pts',(-0.169067964401488,-0.0723017906820314,
0.34390777721563));
#38256=CARTESIAN_POINT('Ctrl Pts',(-0.0308692884081366,-0.181269447386996,
0.355026419198746));
#38257=CARTESIAN_POINT('Ctrl Pts',(0.135606994996762,-0.124186426112907,
0.366145061181863));
#38258=CARTESIAN_POINT('Ctrl Pts',(0.177861387826841,0.0466567491694538,
0.377263703164979));
#38259=CARTESIAN_POINT('Ctrl Pts',(0.0571870330903418,0.174760318061885,
0.388382345148095));
#38260=CARTESIAN_POINT('Ctrl Pts',(-0.115873124952358,0.142775853828764,
0.399500987131212));
#38261=CARTESIAN_POINT('Ctrl Pts',(-0.182788473512851,-0.0199974866820836,
0.410619629114327));
#38262=CARTESIAN_POINT('Ctrl Pts',(-0.0822616502622442,-0.164452261823584,
0.421738271097444));
#38263=CARTESIAN_POINT('Ctrl Pts',(0.0936204134582059,-0.158261630557358,
0.43285691308056));
#38264=CARTESIAN_POINT('Ctrl Pts',(0.183742116834086,-0.00709647969689106,
0.443975555063676));
#38265=CARTESIAN_POINT('Ctrl Pts',(0.10554806974386,0.150569354438759,0.455094197046793));
#38266=CARTESIAN_POINT('Ctrl Pts',(-0.0693325883166112,0.170307127625589,
0.466212839029909));
#38267=CARTESIAN_POINT('Ctrl Pts',(-0.180701587562324,0.0340361833232659,
0.477331481013025));
#38268=CARTESIAN_POINT('Ctrl Pts',(-0.126540093064824,-0.133413381524886,
0.488450122996142));
#38269=CARTESIAN_POINT('Ctrl Pts',(0.0435376164803608,-0.17865050090601,
0.499568764979258));
#38270=CARTESIAN_POINT('Ctrl Pts',(0.173732980498774,-0.0602360109052031,
0.510687406962374));
#38271=CARTESIAN_POINT('Ctrl Pts',(0.144781397169404,0.113357278356683,
0.521806048945491));
#38272=CARTESIAN_POINT('Ctrl Pts',(-0.0167962271460079,0.183110382765203,
0.532924690928607));
#38273=CARTESIAN_POINT('Ctrl Pts',(-0.162987778710162,0.0851264325217889,
0.544043332911723));
#38274=CARTESIAN_POINT('Ctrl Pts',(-0.159875453933454,-0.0908370230265797,
0.555161974894839));
#38275=CARTESIAN_POINT('Ctrl Pts',(-0.0103102773360761,-0.183589824620028,
0.566280616877956));
#38276=CARTESIAN_POINT('Ctrl Pts',(0.14869956060099,-0.108166382022474,
0.577399258861071));
#38277=CARTESIAN_POINT('Ctrl Pts',(0.171494149863546,0.0663421591850832,
0.588517900844189));
#38278=CARTESIAN_POINT('Ctrl Pts',(0.0371926577693494,0.180078404398782,
0.599636542827304));
#38279=CARTESIAN_POINT('Ctrl Pts',(-0.1311789224034,0.128855018683177,0.610755184810421));
#38280=CARTESIAN_POINT('Ctrl Pts',(-0.179384918603911,-0.0404051543769803,
0.621873826793537));
#38281=CARTESIAN_POINT('Ctrl Pts',(-0.0632665469493242,-0.172652453095426,
0.632992468776653));
#38282=CARTESIAN_POINT('Ctrl Pts',(0.110806726459172,-0.146742614445027,
0.644111110759769));
#38283=CARTESIAN_POINT('Ctrl Pts',(0.183376231205259,0.0135898253011021,
0.655229752742886));
#38284=CARTESIAN_POINT('Ctrl Pts',(0.0879651525947856,0.161473395492061,
0.666348394726001));
#38285=CARTESIAN_POINT('Ctrl Pts',(-0.0880258220622017,0.161440330069759,
0.677467036709119));
#38286=CARTESIAN_POINT('Ctrl Pts',(-0.183381324808445,0.013520918395534,
0.688585678692234));
#38287=CARTESIAN_POINT('Ctrl Pts',(-0.11075157823663,-0.146784241118916,
0.699704320675351));
#38288=CARTESIAN_POINT('Ctrl Pts',(0.0633314188332071,-0.172628667698419,
0.710822962658467));
#38289=CARTESIAN_POINT('Ctrl Pts',(0.17940008868909,-0.0403377453646542,
0.721941604641583));
#38290=CARTESIAN_POINT('Ctrl Pts',(0.131130494233742,0.128904301731096,
0.733060246624699));
#38291=CARTESIAN_POINT('Ctrl Pts',(-0.0372603218894873,0.180064416072257,
0.744178888607816));
#38292=CARTESIAN_POINT('Ctrl Pts',(-0.171519066664489,0.0662777133981789,
0.755297530590932));
#38293=CARTESIAN_POINT('Ctrl Pts',(-0.148658905212271,-0.108222250133236,
0.766416172574049));
#38294=CARTESIAN_POINT('Ctrl Pts',(0.0103792628149562,-0.18358593744105,
0.777534814557165));
#38295=CARTESIAN_POINT('Ctrl Pts',(0.159909575810308,-0.0907769413831382,
0.78865345654028));
#38296=CARTESIAN_POINT('Ctrl Pts',(0.162955779866738,0.0851876712390422,
0.799772098523398));
#38297=CARTESIAN_POINT('Ctrl Pts',(0.0167274199086701,0.183116681231986,
0.810890740506512));
#38298=CARTESIAN_POINT('Ctrl Pts',(-0.144823982381472,0.11330286690894,
0.82200938248963));
#38299=CARTESIAN_POINT('Ctrl Pts',(-0.173710333792674,-0.0603012890298399,
0.833128024472746));
#38300=CARTESIAN_POINT('Ctrl Pts',(-0.0434704832044991,-0.178666848096071,
0.844246666455862));
#38301=CARTESIAN_POINT('Ctrl Pts',(0.126590215885116,-0.133365823077974,
0.855365308438979));
#38302=CARTESIAN_POINT('Ctrl Pts',(0.18068878531032,0.0341040818691465,
0.866483950422094));
#38303=CARTESIAN_POINT('Ctrl Pts',(0.069268588294083,0.170333168137465,
0.877602592405212));
#38304=CARTESIAN_POINT('Ctrl Pts',(-0.105604640517969,0.15052968290502,
0.888721234388326));
#38305=CARTESIAN_POINT('Ctrl Pts',(-0.183739437498563,-0.00716552286239433,
0.899839876371444));
#38306=CARTESIAN_POINT('Ctrl Pts',(-0.0935609375970031,-0.15829679799695,
0.91095851835456));
#38307=CARTESIAN_POINT('Ctrl Pts',(0.0823234386500799,-0.164421340203127,
0.922077160337675));
#38308=CARTESIAN_POINT('Ctrl Pts',(0.182795976495949,-0.0199287985657338,
0.933195802320793));
#38309=CARTESIAN_POINT('Ctrl Pts',(0.115819463928053,0.142819381470141,
0.944314444303908));
#38310=CARTESIAN_POINT('Ctrl Pts',(-0.0572526917402423,0.174738822826618,
0.955433086287024));
#38311=CARTESIAN_POINT('Ctrl Pts',(-0.177878918025408,0.046589901053406,
0.966551728270142));
#38312=CARTESIAN_POINT('Ctrl Pts',(-0.135560300066214,-0.124237352171324,
0.977670370253256));
#38313=CARTESIAN_POINT('Ctrl Pts',(0.0309373610575528,-0.181257875466721,
0.988789012236375));
#38314=CARTESIAN_POINT('Ctrl Pts',(0.169095195914933,-0.0722381792257861,
0.999907654219489));
#38315=CARTESIAN_POINT('Ctrl Pts',(0.152354231364944,0.102954552944809,
1.01102629620261));
#38316=CARTESIAN_POINT('Ctrl Pts',(-0.00394931635484403,0.183836962465064,
1.02214493818572));
#38317=CARTESIAN_POINT('Ctrl Pts',(-0.156636075542215,0.0963157594965877,
1.03326358016884));
#38318=CARTESIAN_POINT('Ctrl Pts',(-0.165835572967195,-0.0794329933758677,
1.04438222215196));
#38319=CARTESIAN_POINT('Ctrl Pts',(-0.0231259578302998,-0.182421227428175,
1.05550086413507));
#38320=CARTESIAN_POINT('Ctrl Pts',(0.140774638007895,-0.11829694620695,
1.06661950611819));
#38321=CARTESIAN_POINT('Ctrl Pts',(0.175706993010233,0.0541796064983141,
1.07773814810131));
#38322=CARTESIAN_POINT('Ctrl Pts',(0.0497080432048737,0.177049779856472,
1.08885679008442));
#38323=CARTESIAN_POINT('Ctrl Pts',(-0.121871201614337,0.137688031013954,
1.09997543206754));
#38324=CARTESIAN_POINT('Ctrl Pts',(-0.181724153253684,-0.027712968875509,
1.11109407405065));
#38325=CARTESIAN_POINT('Ctrl Pts',(-0.075277483453787,-0.167898453189698,
1.12221271603377));
#38326=CARTESIAN_POINT('Ctrl Pts',(0.100462758039806,-0.153944373403644,
1.13333135801688));
#38327=CARTESIAN_POINT('Ctrl Pts',(0.155754888396286,-0.0511266487217653,
1.14074378600563));
#38328=CARTESIAN_POINT('Ctrl Pts',(0.155548765964692,0.000619602180124784,
1.14445));
#38329=CARTESIAN_POINT('Ctrl Pts',(-0.074439243930934,0.151537102412034,
-0.0153382721514711));
#38330=CARTESIAN_POINT('Ctrl Pts',(-0.124850938769699,0.126773474301532,
-0.011632058157099));
#38331=CARTESIAN_POINT('Ctrl Pts',(-0.198144687185762,0.0234110607521693,
-0.0042196301683548));
#38332=CARTESIAN_POINT('Ctrl Pts',(-0.126929384324154,-0.154190945884872,
0.00689901181476148));
#38333=CARTESIAN_POINT('Ctrl Pts',(0.0607245306591998,-0.190057817801302,
0.0180176537978778));
#38334=CARTESIAN_POINT('Ctrl Pts',(0.192666956394248,-0.0520688088821623,
0.029136295780994));
#38335=CARTESIAN_POINT('Ctrl Pts',(0.148162620545796,0.133744979191402,
0.0402549377641103));
#38336=CARTESIAN_POINT('Ctrl Pts',(-0.0320884689126903,0.19697575395855,
0.0513735797472264));
#38337=CARTESIAN_POINT('Ctrl Pts',(-0.182932858212653,0.0798032683003624,
0.0624922217303428));
#38338=CARTESIAN_POINT('Ctrl Pts',(-0.166209258212561,-0.110490895887015,
0.0736108637134591));
#38339=CARTESIAN_POINT('Ctrl Pts',(0.00277261860929502,-0.199560929084259,
0.0847295056965753));
#38340=CARTESIAN_POINT('Ctrl Pts',(0.169212878157669,-0.10582957656395,
0.0958481476796916));
#38341=CARTESIAN_POINT('Ctrl Pts',(0.180647734334385,0.0848489294255244,
0.106966789662808));
#38342=CARTESIAN_POINT('Ctrl Pts',(0.0266009379770665,0.197800732458805,
0.118085431645924));
#38343=CARTESIAN_POINT('Ctrl Pts',(-0.151813213871049,0.12955921992025,
0.129204073629041));
#38344=CARTESIAN_POINT('Ctrl Pts',(-0.191160010957712,-0.0573645458357494,
0.140322715612156));
#38345=CARTESIAN_POINT('Ctrl Pts',(-0.0553958736254638,-0.191739695630841,
0.151441357595273));
#38346=CARTESIAN_POINT('Ctrl Pts',(0.131113249878304,-0.150473072594935,
0.162559999578389));
#38347=CARTESIAN_POINT('Ctrl Pts',(0.19751696791516,0.0286334691329668,
0.173678641561505));
#38348=CARTESIAN_POINT('Ctrl Pts',(0.0829865639814035,0.181510481441338,
0.184797283544622));
#38349=CARTESIAN_POINT('Ctrl Pts',(-0.107563127424026,0.168116033596642,
0.195915925527738));
#38350=CARTESIAN_POINT('Ctrl Pts',(-0.199580330447296,0.000719997322039096,
0.207034567510854));
#38351=CARTESIAN_POINT('Ctrl Pts',(-0.108773290717609,-0.167335583465575,
0.218153209493971));
#38352=CARTESIAN_POINT('Ctrl Pts',(0.0816748015321165,-0.182104512374819,
0.229271851477087));
#38353=CARTESIAN_POINT('Ctrl Pts',(0.197305232620797,-0.0300578063700233,
0.240390493460203));
#38354=CARTESIAN_POINT('Ctrl Pts',(0.132195510545613,0.149523153675082,
0.251509135443319));
#38355=CARTESIAN_POINT('Ctrl Pts',(-0.054011034229875,0.192134418384253,
0.262627777426435));
#38356=CARTESIAN_POINT('Ctrl Pts',(-0.190741128502276,0.0587422201459823,
0.273746419409552));
#38357=CARTESIAN_POINT('Ctrl Pts',(-0.152744073944838,-0.128460400121777,
0.284865061392668));
#38358=CARTESIAN_POINT('Ctrl Pts',(0.0251731789602741,-0.19798772081443,
0.295983703375785));
#38359=CARTESIAN_POINT('Ctrl Pts',(0.180030707836241,-0.0861496997406464,
0.3071023453589));
#38360=CARTESIAN_POINT('Ctrl Pts',(0.169972297898904,0.104605183790867,
0.318220987342017));
#38361=CARTESIAN_POINT('Ctrl Pts',(0.00421188903066005,0.199537180797957,
0.329339629325133));
#38362=CARTESIAN_POINT('Ctrl Pts',(-0.165406792919015,0.111684463493277,
0.34045827130825));
#38363=CARTESIAN_POINT('Ctrl Pts',(-0.183505676565636,-0.0784760676748057,
0.351576913291366));
#38364=CARTESIAN_POINT('Ctrl Pts',(-0.0335053992900935,-0.196749116257395,
0.362695555274482));
#38365=CARTESIAN_POINT('Ctrl Pts',(0.147187277329603,-0.134791438607496,
0.373814197257599));
#38366=CARTESIAN_POINT('Ctrl Pts',(0.193050022360002,0.0506410445822938,
0.384932839240714));
#38367=CARTESIAN_POINT('Ctrl Pts',(0.0620705716495424,0.189684133929807,
0.396051481223831));
#38368=CARTESIAN_POINT('Ctrl Pts',(-0.125768215554202,0.154968327363698,
0.407170123206947));
#38369=CARTESIAN_POINT('Ctrl Pts',(-0.19839786099702,-0.0217051901949521,
0.418288765190064));
#38370=CARTESIAN_POINT('Ctrl Pts',(-0.0892864584974339,-0.178495811879663,
0.429407407173179));
#38371=CARTESIAN_POINT('Ctrl Pts',(0.101615213578872,-0.171776526041577,
0.440526049156296));
#38372=CARTESIAN_POINT('Ctrl Pts',(0.199432941554622,-0.00770249001709277,
0.451644691139412));
#38373=CARTESIAN_POINT('Ctrl Pts',(0.114561442891388,0.16342736102696,0.462763333122529));
#38374=CARTESIAN_POINT('Ctrl Pts',(-0.0752533075803338,0.184850659257176,
0.473881975105645));
#38375=CARTESIAN_POINT('Ctrl Pts',(-0.196132763527948,0.0369427340688636,
0.485000617088761));
#38376=CARTESIAN_POINT('Ctrl Pts',(-0.13734609908354,-0.144806338245697,
0.496119259071877));
#38377=CARTESIAN_POINT('Ctrl Pts',(0.0472555507281729,-0.19390652246629,
0.507237901054994));
#38378=CARTESIAN_POINT('Ctrl Pts',(0.188569065943703,-0.0653799196903168,
0.51835654303811));
#38379=CARTESIAN_POINT('Ctrl Pts',(0.157145135896933,0.123037525956625,
0.529475185021226));
#38380=CARTESIAN_POINT('Ctrl Pts',(-0.0182305561972616,0.198747259981946,
0.540593827004342));
#38381=CARTESIAN_POINT('Ctrl Pts',(-0.176906267902489,0.0923958814363803,
0.551712468987459));
#38382=CARTESIAN_POINT('Ctrl Pts',(-0.173528163328608,-0.0985941329968107,
0.562831110970574));
#38383=CARTESIAN_POINT('Ctrl Pts',(-0.0111907328205795,-0.199267644208816,
0.573949752953692));
#38384=CARTESIAN_POINT('Ctrl Pts',(0.161397894448518,-0.117403348321834,
0.585068394936807));
#38385=CARTESIAN_POINT('Ctrl Pts',(0.186139048335769,0.0720075080408093,
0.596187036919923));
#38386=CARTESIAN_POINT('Ctrl Pts',(0.0403687585131819,0.19545636307293,
0.60730567890304));
#38387=CARTESIAN_POINT('Ctrl Pts',(-0.142381065460884,0.139858709874703,
0.618424320886156));
#38388=CARTESIAN_POINT('Ctrl Pts',(-0.194703656429618,-0.0438555891823412,
0.629542962869273));
#38389=CARTESIAN_POINT('Ctrl Pts',(-0.0686692511086116,-0.187396265922711,
0.640661604852388));
#38390=CARTESIAN_POINT('Ctrl Pts',(0.120269167366484,-0.159273833100625,
0.651780246835506));
#38391=CARTESIAN_POINT('Ctrl Pts',(0.199035810790665,0.0147503407586138,
0.662898888818621));
#38392=CARTESIAN_POINT('Ctrl Pts',(0.0954770165847204,0.175262562555938,
0.674017530801738));
#38393=CARTESIAN_POINT('Ctrl Pts',(-0.09554286697633,0.17522667348191,0.685136172784854));
#38394=CARTESIAN_POINT('Ctrl Pts',(-0.199041339366714,0.0146755494853507,
0.69625481476797));
#38395=CARTESIAN_POINT('Ctrl Pts',(-0.120209309711463,-0.159319014522084,
0.707373456751086));
#38396=CARTESIAN_POINT('Ctrl Pts',(0.0687396627858533,-0.187370449350155,
0.718492098734203));
#38397=CARTESIAN_POINT('Ctrl Pts',(0.194720121977979,-0.0437824237162718,
0.729610740717318));
#38398=CARTESIAN_POINT('Ctrl Pts',(0.142328501723757,0.139912201493195,
0.740729382700435));
#38399=CARTESIAN_POINT('Ctrl Pts',(-0.0404422008722263,0.195441180200575,
0.751848024683551));
#38400=CARTESIAN_POINT('Ctrl Pts',(-0.186166092929526,0.0719375588474842,
0.762966666666667));
#38401=CARTESIAN_POINT('Ctrl Pts',(-0.161353767256008,-0.117463987340584,
0.774085308649784));
#38402=CARTESIAN_POINT('Ctrl Pts',(0.0112656093769942,-0.199263425080664,
0.7852039506329));
#38403=CARTESIAN_POINT('Ctrl Pts',(0.173565199074082,-0.0985289206269375,
0.796322592616017));
#38404=CARTESIAN_POINT('Ctrl Pts',(0.176871536488809,0.0924623496894334,
0.807441234599133));
#38405=CARTESIAN_POINT('Ctrl Pts',(0.0181558731034875,0.198754096312013,
0.818559876582249));
#38406=CARTESIAN_POINT('Ctrl Pts',(-0.157191357711808,0.122978467993954,
0.829678518565365));
#38407=CARTESIAN_POINT('Ctrl Pts',(-0.188544485301595,-0.06545077229961,
0.840797160548482));
#38408=CARTESIAN_POINT('Ctrl Pts',(-0.0471826845453332,-0.193924265639472,
0.851915802531597));
#38409=CARTESIAN_POINT('Ctrl Pts',(0.137400502187529,-0.144754718502077,
0.863034444514714));
#38410=CARTESIAN_POINT('Ctrl Pts',(0.196118868016023,0.0370164308726493,
0.87415308649783));
#38411=CARTESIAN_POINT('Ctrl Pts',(0.0751838422178375,0.184878923522181,
0.885271728480947));
#38412=CARTESIAN_POINT('Ctrl Pts',(-0.114622844578058,0.163384301706618,
0.896390370464062));
#38413=CARTESIAN_POINT('Ctrl Pts',(-0.199430033414812,-0.0077774291863319,
0.90750901244718));
#38414=CARTESIAN_POINT('Ctrl Pts',(-0.101550658722561,-0.171814696636568,
0.918627654430294));
#38415=CARTESIAN_POINT('Ctrl Pts',(0.0893535233606871,-0.178462249679383,
0.929746296413413));
#38416=CARTESIAN_POINT('Ctrl Pts',(0.198406004704164,-0.0216306363946107,
0.940864938396527));
#38417=CARTESIAN_POINT('Ctrl Pts',(0.12570997209806,0.155015572087487,0.951983580379645));
#38418=CARTESIAN_POINT('Ctrl Pts',(-0.0621418372793996,0.18966080308943,
0.963102222362759));
#38419=CARTESIAN_POINT('Ctrl Pts',(-0.193069049565776,0.050568487910749,
0.974220864345877));
#38420=CARTESIAN_POINT('Ctrl Pts',(-0.147136594843111,-0.134846713542859,
0.985339506328992));
#38421=CARTESIAN_POINT('Ctrl Pts',(0.0335792850651442,-0.196736556142493,
0.99645814831211));
#38422=CARTESIAN_POINT('Ctrl Pts',(0.183535233538869,-0.0784070240605622,
1.00757679029522));
#38423=CARTESIAN_POINT('Ctrl Pts',(0.165364659137136,0.111746450372967,
1.01869543227834));
#38424=CARTESIAN_POINT('Ctrl Pts',(-0.00428657180698079,0.199535886614283,
1.02981407426146));
#38425=CARTESIAN_POINT('Ctrl Pts',(-0.170012155281541,0.104540731136874,
1.04093271624457));
#38426=CARTESIAN_POINT('Ctrl Pts',(-0.179997252133044,-0.0862162458906591,
1.05205135822769));
#38427=CARTESIAN_POINT('Ctrl Pts',(-0.0251008199743871,-0.197999253599851,
1.06317000021081));
#38428=CARTESIAN_POINT('Ctrl Pts',(0.152796215902707,-0.128399021223231,
1.07428864219392));
#38429=CARTESIAN_POINT('Ctrl Pts',(0.190711651044001,0.0588063231359589,
1.08540728417704));
#38430=CARTESIAN_POINT('Ctrl Pts',(0.0539529066393858,0.192169106390877,
1.09652592616015));
#38431=CARTESIAN_POINT('Ctrl Pts',(-0.132278503412967,0.149446025304978,
1.10764456814327));
#38432=CARTESIAN_POINT('Ctrl Pts',(-0.197242652143987,-0.0300795429882017,
1.11876321012639));
#38433=CARTESIAN_POINT('Ctrl Pts',(-0.0817058724297523,-0.182236293883171,
1.12988185210951));
#38434=CARTESIAN_POINT('Ctrl Pts',(0.109041866382002,-0.167090592797485,
1.14100049409262));
#38435=CARTESIAN_POINT('Ctrl Pts',(0.169055718360052,-0.0554926552610627,
1.14841292208137));
#38436=CARTESIAN_POINT('Ctrl Pts',(0.16883199391646,0.000672513670271936,
1.15211913607574));
#38437=CARTESIAN_POINT('Ctrl Pts',(-0.0802959149489932,0.163459616787394,
-0.00766913607573554));
#38438=CARTESIAN_POINT('Ctrl Pts',(-0.134673860605774,0.136747655843322,
-0.00396292208136346));
#38439=CARTESIAN_POINT('Ctrl Pts',(-0.213734155664247,0.0252529773779836,
0.00344950590738073));
#38440=CARTESIAN_POINT('Ctrl Pts',(-0.136915832429422,-0.166322257224481,
0.014568147890497));
#38441=CARTESIAN_POINT('Ctrl Pts',(0.0655021664869751,-0.205011034068591,
0.0256867898736133));
#38442=CARTESIAN_POINT('Ctrl Pts',(0.20782545237117,-0.0561654367873057,
0.0368054318567295));
#38443=CARTESIAN_POINT('Ctrl Pts',(0.159819640148463,0.144267659192936,
0.0479240738398458));
#38444=CARTESIAN_POINT('Ctrl Pts',(-0.0346130996849898,0.212473254047885,
0.0590427158229621));
#38445=CARTESIAN_POINT('Ctrl Pts',(-0.197325502634714,0.0860819657174806,
0.0701613578060782));
#38446=CARTESIAN_POINT('Ctrl Pts',(-0.179286136672128,-0.119184009808233,
0.0812799997891947));
#38447=CARTESIAN_POINT('Ctrl Pts',(0.00299076046828686,-0.215261823504807,
0.0923986417723108));
#38448=CARTESIAN_POINT('Ctrl Pts',(0.182526073013706,-0.114155950949091,
0.103517283755427));
#38449=CARTESIAN_POINT('Ctrl Pts',(0.194860591616173,0.0915246053141843,
0.114635925738543));
#38450=CARTESIAN_POINT('Ctrl Pts',(0.0286938251999433,0.213363139543668,
0.12575456772166));
#38451=CARTESIAN_POINT('Ctrl Pts',(-0.163757451921909,0.139752576117334,
0.136873209704776));
#38452=CARTESIAN_POINT('Ctrl Pts',(-0.20619994469249,-0.0618778274775138,
0.147991851687892));
#38453=CARTESIAN_POINT('Ctrl Pts',(-0.0597542656570052,-0.206825237330522,
0.159110493671008));
#38454=CARTESIAN_POINT('Ctrl Pts',(0.141428872795678,-0.162311872087351,
0.170229135654125));
#38455=CARTESIAN_POINT('Ctrl Pts',(0.213057049201279,0.0308862702088754,
0.181347777637241));
#38456=CARTESIAN_POINT('Ctrl Pts',(0.0895157141781652,0.195791217246742,
0.192466419620357));
#38457=CARTESIAN_POINT('Ctrl Pts',(-0.116025892730732,0.181342931797682,
0.203585061603473));
#38458=CARTESIAN_POINT('Ctrl Pts',(-0.215282751312695,0.000776644692787891,
0.21470370358659));
#38459=CARTESIAN_POINT('Ctrl Pts',(-0.1173312682795,-0.180501078038335,
0.225822345569706));
#38460=CARTESIAN_POINT('Ctrl Pts',(0.0881007459369614,-0.196431984868673,
0.236940987552822));
#38461=CARTESIAN_POINT('Ctrl Pts',(0.212828655167567,-0.0324226703065412,
0.248059629535939));
#38462=CARTESIAN_POINT('Ctrl Pts',(0.142596282698117,0.16128721621003,0.259178271519055));
#38463=CARTESIAN_POINT('Ctrl Pts',(-0.0582604709802392,0.207251015763547,
0.270296913502171));
#38464=CARTESIAN_POINT('Ctrl Pts',(-0.205748105739819,0.0633638933400953,
0.281415555485287));
#38465=CARTESIAN_POINT('Ctrl Pts',(-0.16476154945659,-0.138567304257714,
0.292534197468403));
#38466=CARTESIAN_POINT('Ctrl Pts',(0.0271537341065049,-0.213564839618882,
0.30365283945152));
#38467=CARTESIAN_POINT('Ctrl Pts',(0.19419501920302,-0.092927716590924,
0.314771481434636));
#38468=CARTESIAN_POINT('Ctrl Pts',(0.183345241771109,0.11283522638527,0.325890123417753));
#38469=CARTESIAN_POINT('Ctrl Pts',(0.0045432686513366,0.215236206769919,
0.337008765400868));
#38470=CARTESIAN_POINT('Ctrl Pts',(-0.178420535659039,0.120471483967528,
0.348127407383985));
#38471=CARTESIAN_POINT('Ctrl Pts',(-0.197943388729784,-0.08465034466758,
0.359246049367101));
#38472=CARTESIAN_POINT('Ctrl Pts',(-0.0361415101720502,-0.212228785127794,
0.370364691350217));
#38473=CARTESIAN_POINT('Ctrl Pts',(0.158767559662444,-0.145396451102085,
0.381483333333334));
#38474=CARTESIAN_POINT('Ctrl Pts',(0.208238656893164,0.0546253399951339,
0.39260197531645));
#38475=CARTESIAN_POINT('Ctrl Pts',(0.0669541102087431,0.204607949797729,
0.403720617299566));
#38476=CARTESIAN_POINT('Ctrl Pts',(-0.135663306156047,0.167160800898631,
0.414839259282683));
#38477=CARTESIAN_POINT('Ctrl Pts',(-0.214007248481188,-0.0234128937078206,
0.425957901265799));
#38478=CARTESIAN_POINT('Ctrl Pts',(-0.0963112667326238,-0.192539361935742,
0.437076543248915));
#38479=CARTESIAN_POINT('Ctrl Pts',(0.109610013699538,-0.185291421525797,
0.448195185232032));
#38480=CARTESIAN_POINT('Ctrl Pts',(0.215123766275159,-0.00830850033729405,
0.459313827215147));
#38481=CARTESIAN_POINT('Ctrl Pts',(0.123574816038915,0.176285367615161,
0.470432469198265));
#38482=CARTESIAN_POINT('Ctrl Pts',(-0.0811740268440561,0.199394190888763,
0.48155111118138));
#38483=CARTESIAN_POINT('Ctrl Pts',(-0.211563939493572,0.0398492848144611,
0.492669753164497));
#38484=CARTESIAN_POINT('Ctrl Pts',(-0.148152105102257,-0.156199294966507,
0.503788395147612));
#38485=CARTESIAN_POINT('Ctrl Pts',(0.0509734849759847,-0.20916254402657,
0.51490703713073));
#38486=CARTESIAN_POINT('Ctrl Pts',(0.203405151388631,-0.0705238284754304,
0.526025679113844));
#38487=CARTESIAN_POINT('Ctrl Pts',(0.169508874624462,0.132717773556567,
0.537144321096963));
#38488=CARTESIAN_POINT('Ctrl Pts',(-0.019664885248515,0.21438413719869,
0.548262963080077));
#38489=CARTESIAN_POINT('Ctrl Pts',(-0.190824757094816,0.0996653303509719,
0.559381605063195));
#38490=CARTESIAN_POINT('Ctrl Pts',(-0.187180872723762,-0.106351242967042,
0.570500247046309));
#38491=CARTESIAN_POINT('Ctrl Pts',(-0.012071188305083,-0.214945463797604,
0.581618889029427));
#38492=CARTESIAN_POINT('Ctrl Pts',(0.174096228296046,-0.126640314621194,
0.592737531012542));
#38493=CARTESIAN_POINT('Ctrl Pts',(0.200783946807991,0.0776728568965356,
0.60385617299566));
#38494=CARTESIAN_POINT('Ctrl Pts',(0.0435448592570146,0.210834321747079,
0.614974814978775));
#38495=CARTESIAN_POINT('Ctrl Pts',(-0.153583208518367,0.150862401066228,
0.626093456961893));
#38496=CARTESIAN_POINT('Ctrl Pts',(-0.210022394255324,-0.0473060239877022,
0.637212098945007));
#38497=CARTESIAN_POINT('Ctrl Pts',(-0.074071955267899,-0.202140078749996,
0.648330740928124));
#38498=CARTESIAN_POINT('Ctrl Pts',(0.129731608273796,-0.171805051756223,
0.65944938291124));
#38499=CARTESIAN_POINT('Ctrl Pts',(0.214695390376071,0.015910856216126,
0.670568024894357));
#38500=CARTESIAN_POINT('Ctrl Pts',(0.102988880574655,0.189051729619815,
0.681686666877473));
#38501=CARTESIAN_POINT('Ctrl Pts',(-0.103059911890458,0.189013016894061,
0.692805308860589));
#38502=CARTESIAN_POINT('Ctrl Pts',(-0.214701353924984,0.0158301805751674,
0.703923950843705));
#38503=CARTESIAN_POINT('Ctrl Pts',(-0.129667041186295,-0.171853787925252,
0.715042592826822));
#38504=CARTESIAN_POINT('Ctrl Pts',(0.0741479067384996,-0.20211223100189,
0.726161234809938));
#38505=CARTESIAN_POINT('Ctrl Pts',(0.210040155266868,-0.0472271020678894,
0.737279876793055));
#38506=CARTESIAN_POINT('Ctrl Pts',(0.153526509213771,0.150920101255294,
0.748398518776171));
#38507=CARTESIAN_POINT('Ctrl Pts',(-0.0436240798549652,0.210817944328893,
0.759517160759286));
#38508=CARTESIAN_POINT('Ctrl Pts',(-0.200813119194563,0.0775974042967894,
0.770635802742404));
#38509=CARTESIAN_POINT('Ctrl Pts',(-0.174048629299744,-0.126705724547931,
0.781754444725519));
#38510=CARTESIAN_POINT('Ctrl Pts',(0.0121519559390324,-0.214940912720278,
0.792873086708636));
#38511=CARTESIAN_POINT('Ctrl Pts',(0.187220822337856,-0.106280899870737,
0.803991728691751));
#38512=CARTESIAN_POINT('Ctrl Pts',(0.190787293110882,0.0997370281398245,
0.815110370674869));
#38513=CARTESIAN_POINT('Ctrl Pts',(0.0195843262983046,0.21439151139204,
0.826229012657984));
#38514=CARTESIAN_POINT('Ctrl Pts',(-0.169558733042143,0.132654069078969,
0.837347654641101));
#38515=CARTESIAN_POINT('Ctrl Pts',(-0.203378636810517,-0.0706002555693802,
0.848466296624217));
#38516=CARTESIAN_POINT('Ctrl Pts',(-0.0508948858861673,-0.209181683182873,
0.859584938607333));
#38517=CARTESIAN_POINT('Ctrl Pts',(0.148210788489943,-0.156143613926181,
0.870703580590451));
#38518=CARTESIAN_POINT('Ctrl Pts',(0.211548950721726,0.0399287798761521,
0.881822222573564));
#38519=CARTESIAN_POINT('Ctrl Pts',(0.0810990961415922,0.199424678906897,
0.892940864556684));
#38520=CARTESIAN_POINT('Ctrl Pts',(-0.123641048638147,0.176238920508216,
0.904059506539796));
#38521=CARTESIAN_POINT('Ctrl Pts',(-0.215120629331062,-0.00838933551026959,
0.915178148522916));
#38522=CARTESIAN_POINT('Ctrl Pts',(-0.109540379848118,-0.185332595276186,
0.926296790506031));
#38523=CARTESIAN_POINT('Ctrl Pts',(0.0963836080712942,-0.19250315915564,
0.937415432489146));
#38524=CARTESIAN_POINT('Ctrl Pts',(0.214016032912378,-0.0233324742234878,
0.948534074472264));
#38525=CARTESIAN_POINT('Ctrl Pts',(0.135600480268067,0.167211762704833,
0.95965271645538));
#38526=CARTESIAN_POINT('Ctrl Pts',(-0.0670309828185569,0.204582783352242,
0.970771358438496));
#38527=CARTESIAN_POINT('Ctrl Pts',(-0.208259181106143,0.0545470747680921,
0.981890000421612));
#38528=CARTESIAN_POINT('Ctrl Pts',(-0.158712889620009,-0.145456074914393,
0.993008642404728));
#38529=CARTESIAN_POINT('Ctrl Pts',(0.0362212090727357,-0.212215236818265,
1.00412728438785));
#38530=CARTESIAN_POINT('Ctrl Pts',(0.197975271162805,-0.0845758688953388,
1.01524592637096));
#38531=CARTESIAN_POINT('Ctrl Pts',(0.178375086909329,0.120538347801125,
1.02636456835408));
#38532=CARTESIAN_POINT('Ctrl Pts',(-0.00462382725911752,0.215234810763501,
1.03748321033719));
#38533=CARTESIAN_POINT('Ctrl Pts',(-0.183388235020868,0.112765702777161,
1.04860185232031));
#38534=CARTESIAN_POINT('Ctrl Pts',(-0.194158931298892,-0.0929994984054507,
1.05972049430343));
#38535=CARTESIAN_POINT('Ctrl Pts',(-0.0270756821184746,-0.213577279771527,
1.07083913628654));
#38536=CARTESIAN_POINT('Ctrl Pts',(0.164817793797518,-0.138501096239512,
1.08195777826966));
#38537=CARTESIAN_POINT('Ctrl Pts',(0.20571630907777,0.0634330397736036,
1.09307642025277));
#38538=CARTESIAN_POINT('Ctrl Pts',(0.058197770073898,0.207288432925282,
1.10419506223589));
#38539=CARTESIAN_POINT('Ctrl Pts',(-0.142685805211597,0.161204019596003,
1.11531370421901));
#38540=CARTESIAN_POINT('Ctrl Pts',(-0.212761151034289,-0.0324461171008946,
1.12643234620212));
#38541=CARTESIAN_POINT('Ctrl Pts',(-0.0881342614057178,-0.196574134576644,
1.13755098818524));
#38542=CARTESIAN_POINT('Ctrl Pts',(0.117620974724197,-0.180236812191326,
1.14866963016836));
#38543=CARTESIAN_POINT('Ctrl Pts',(0.182356548323819,-0.0598586618003602,
1.1560820581571));
#38544=CARTESIAN_POINT('Ctrl Pts',(0.182115221868229,0.000725425160419088,
1.15978827215147));
#38545=CARTESIAN_POINT('Ctrl Pts',(-0.0861525859670525,0.175382131162755,
-1.38777878078145E-17));
#38546=CARTESIAN_POINT('Ctrl Pts',(-0.144496782441849,0.146721837385112,
0.00370621399437207));
#38547=CARTESIAN_POINT('Ctrl Pts',(-0.229323624142731,0.0270948940037977,
0.0111186419831162));
#38548=CARTESIAN_POINT('Ctrl Pts',(-0.14690228053469,-0.178453568564088,
0.0222372839662325));
#38549=CARTESIAN_POINT('Ctrl Pts',(0.0702798023147504,-0.219964250335881,
0.0333559259493488));
#38550=CARTESIAN_POINT('Ctrl Pts',(0.222983948348091,-0.0602620646924488,
0.044474567932465));
#38551=CARTESIAN_POINT('Ctrl Pts',(0.171476659751129,0.154790339194469,
0.0555932099155814));
#38552=CARTESIAN_POINT('Ctrl Pts',(-0.0371377304572895,0.22797075413722,
0.0667118518986976));
#38553=CARTESIAN_POINT('Ctrl Pts',(-0.211718147056775,0.0923606631345987,
0.0778304938818138));
#38554=CARTESIAN_POINT('Ctrl Pts',(-0.192363015131696,-0.12787712372945,
0.0889491358649302));
#38555=CARTESIAN_POINT('Ctrl Pts',(0.00320890232727887,-0.230962717925356,
0.100067777848046));
#38556=CARTESIAN_POINT('Ctrl Pts',(0.195839267869742,-0.122482325334233,
0.111186419831163));
#38557=CARTESIAN_POINT('Ctrl Pts',(0.209073448897961,0.0982002812028443,
0.122305061814279));
#38558=CARTESIAN_POINT('Ctrl Pts',(0.0307867124228199,0.228925546628532,
0.133423703797395));
#38559=CARTESIAN_POINT('Ctrl Pts',(-0.175701689972769,0.149945932314417,
0.144542345780511));
#38560=CARTESIAN_POINT('Ctrl Pts',(-0.221239878427269,-0.0663911091192784,
0.155660987763628));
#38561=CARTESIAN_POINT('Ctrl Pts',(-0.0641126576885465,-0.221910779030204,
0.166779629746744));
#38562=CARTESIAN_POINT('Ctrl Pts',(0.151744495713052,-0.174150671579767,
0.17789827172986));
#38563=CARTESIAN_POINT('Ctrl Pts',(0.228597130487397,0.0331390712847842,
0.189016913712977));
#38564=CARTESIAN_POINT('Ctrl Pts',(0.0960448643749269,0.210071953052146,
0.200135555696093));
#38565=CARTESIAN_POINT('Ctrl Pts',(-0.124488658037438,0.194569829998722,
0.211254197679209));
#38566=CARTESIAN_POINT('Ctrl Pts',(-0.230985172178094,0.000833292063536468,
0.222372839662325));
#38567=CARTESIAN_POINT('Ctrl Pts',(-0.12588924584139,-0.193666572611094,
0.233491481645442));
#38568=CARTESIAN_POINT('Ctrl Pts',(0.0945266903418065,-0.210759457362527,
0.244610123628558));
#38569=CARTESIAN_POINT('Ctrl Pts',(0.228352077714336,-0.0347875342430591,
0.255728765611674));
#38570=CARTESIAN_POINT('Ctrl Pts',(0.152997054850621,0.173051278744978,
0.26684740759479));
#38571=CARTESIAN_POINT('Ctrl Pts',(-0.0625099077306038,0.222367613142842,
0.277966049577907));
#38572=CARTESIAN_POINT('Ctrl Pts',(-0.220755082977362,0.0679855665342084,
0.289084691561023));
#38573=CARTESIAN_POINT('Ctrl Pts',(-0.176779024968342,-0.148674208393651,
0.300203333544139));
#38574=CARTESIAN_POINT('Ctrl Pts',(0.0291342892527361,-0.229141958423335,
0.311321975527256));
#38575=CARTESIAN_POINT('Ctrl Pts',(0.208359330569799,-0.0997057334412016,
0.322440617510372));
#38576=CARTESIAN_POINT('Ctrl Pts',(0.196718185643314,0.121065268979674,
0.333559259493488));
#38577=CARTESIAN_POINT('Ctrl Pts',(0.00487464827201324,0.230935232741881,
0.344677901476604));
#38578=CARTESIAN_POINT('Ctrl Pts',(-0.191434278399063,0.129258504441778,
0.355796543459721));
#38579=CARTESIAN_POINT('Ctrl Pts',(-0.212381100893932,-0.0908246216603541,
0.366915185442837));
#38580=CARTESIAN_POINT('Ctrl Pts',(-0.038777621054007,-0.227708453998192,
0.378033827425954));
#38581=CARTESIAN_POINT('Ctrl Pts',(0.170347841995286,-0.156001463596674,
0.389152469409069));
#38582=CARTESIAN_POINT('Ctrl Pts',(0.223427291426326,0.058609635407974,
0.400271111392186));
#38583=CARTESIAN_POINT('Ctrl Pts',(0.0718376487679439,0.219531765665651,
0.411389753375301));
#38584=CARTESIAN_POINT('Ctrl Pts',(-0.145558396757891,0.179353274433565,
0.422508395358419));
#38585=CARTESIAN_POINT('Ctrl Pts',(-0.229616635965357,-0.0251205972206891,
0.433627037341534));
#38586=CARTESIAN_POINT('Ctrl Pts',(-0.103336074967814,-0.206582911991821,
0.444745679324651));
#38587=CARTESIAN_POINT('Ctrl Pts',(0.117604813820203,-0.198806317010017,
0.455864321307767));
#38588=CARTESIAN_POINT('Ctrl Pts',(0.230814590995695,-0.00891451065749571,
0.466982963290884));
#38589=CARTESIAN_POINT('Ctrl Pts',(0.132588189186442,0.189143374203362,
0.478101605273999));
#38590=CARTESIAN_POINT('Ctrl Pts',(-0.0870947461077786,0.21393772252035,
0.489220247257116));
#38591=CARTESIAN_POINT('Ctrl Pts',(-0.226995115459196,0.0427558355600586,
0.500338889240232));
#38592=CARTESIAN_POINT('Ctrl Pts',(-0.158958111120973,-0.167592251687317,
0.511457531223348));
#38593=CARTESIAN_POINT('Ctrl Pts',(0.0546914192237968,-0.224418565586851,
0.522576173206465));
#38594=CARTESIAN_POINT('Ctrl Pts',(0.21824123683356,-0.0756677372605439,
0.533694815189581));
#38595=CARTESIAN_POINT('Ctrl Pts',(0.181872613351991,0.14239802115651,0.544813457172697));
#38596=CARTESIAN_POINT('Ctrl Pts',(-0.0210992142997687,0.230021014415434,
0.555932099155813));
#38597=CARTESIAN_POINT('Ctrl Pts',(-0.204743246287144,0.106934779265563,
0.567050741138931));
#38598=CARTESIAN_POINT('Ctrl Pts',(-0.200833582118916,-0.114108352937273,
0.578169383122044));
#38599=CARTESIAN_POINT('Ctrl Pts',(-0.0129516437895867,-0.230623283386393,
0.589288025105164));
#38600=CARTESIAN_POINT('Ctrl Pts',(0.186794562143574,-0.135877280920554,
0.600406667088277));
#38601=CARTESIAN_POINT('Ctrl Pts',(0.215428845280213,0.083338205752262,
0.611525309071395));
#38602=CARTESIAN_POINT('Ctrl Pts',(0.0467209600008474,0.226212280421227,
0.622643951054511));
#38603=CARTESIAN_POINT('Ctrl Pts',(-0.164785351575852,0.161866092257753,
0.633762593037627));
#38604=CARTESIAN_POINT('Ctrl Pts',(-0.225341132081031,-0.0507564587930634,
0.644881235020743));
#38605=CARTESIAN_POINT('Ctrl Pts',(-0.0794746594271866,-0.21688389157728,
0.655999877003859));
#38606=CARTESIAN_POINT('Ctrl Pts',(0.139194049181108,-0.184336270411821,
0.667118518986976));
#38607=CARTESIAN_POINT('Ctrl Pts',(0.230354969961477,0.0170713716736379,
0.678237160970093));
#38608=CARTESIAN_POINT('Ctrl Pts',(0.11050074456459,0.202840896683692,0.689355802953208));
#38609=CARTESIAN_POINT('Ctrl Pts',(-0.110576956804586,0.202799360306213,
0.700474444936325));
#38610=CARTESIAN_POINT('Ctrl Pts',(-0.230361368483253,0.0169848116649841,
0.711593086919441));
#38611=CARTESIAN_POINT('Ctrl Pts',(-0.139124772661127,-0.184388561328419,
0.722711728902557));
#38612=CARTESIAN_POINT('Ctrl Pts',(0.0795561506911461,-0.216854012653626,
0.733830370885674));
#38613=CARTESIAN_POINT('Ctrl Pts',(0.225360188555757,-0.0506717804195071,
0.744949012868789));
#38614=CARTESIAN_POINT('Ctrl Pts',(0.164724516703786,0.161928001017393,
0.756067654851907));
#38615=CARTESIAN_POINT('Ctrl Pts',(-0.0468059588377044,0.226194708457211,
0.767186296835021));
#38616=CARTESIAN_POINT('Ctrl Pts',(-0.2154601454596,0.0832572497460946,
0.778304938818139));
#38617=CARTESIAN_POINT('Ctrl Pts',(-0.18674349134348,-0.135947461755279,
0.789423580801255));
#38618=CARTESIAN_POINT('Ctrl Pts',(0.0130383025010703,-0.230618400359892,
0.800542222784371));
#38619=CARTESIAN_POINT('Ctrl Pts',(0.200876445601631,-0.114032879114536,
0.811660864767487));
#38620=CARTESIAN_POINT('Ctrl Pts',(0.204703049732954,0.107011706590215,
0.822779506750604));
#38621=CARTESIAN_POINT('Ctrl Pts',(0.0210127794931219,0.230028926472067,
0.83389814873372));
#38622=CARTESIAN_POINT('Ctrl Pts',(-0.181926108372479,0.142329670163983,
0.845016790716836));
#38623=CARTESIAN_POINT('Ctrl Pts',(-0.218212788319439,-0.0757497388391501,
0.856135432699953));
#38624=CARTESIAN_POINT('Ctrl Pts',(-0.0546070872270015,-0.224439100726275,
0.867254074683069));
#38625=CARTESIAN_POINT('Ctrl Pts',(0.159021074792356,-0.167532509350284,
0.878372716666185));
#38626=CARTESIAN_POINT('Ctrl Pts',(0.226979033427429,0.0428411288796547,
0.889491358649301));
#38627=CARTESIAN_POINT('Ctrl Pts',(0.0870143500653468,0.213970434291613,
0.900610000632417));
#38628=CARTESIAN_POINT('Ctrl Pts',(-0.132659252698235,0.189093539309814,
0.911728642615534));
#38629=CARTESIAN_POINT('Ctrl Pts',(-0.230811225247311,-0.00900124183420705,
0.92284728459865));
#38630=CARTESIAN_POINT('Ctrl Pts',(-0.117530100973675,-0.198850493915805,
0.933965926581767));
#38631=CARTESIAN_POINT('Ctrl Pts',(0.103413692781901,-0.206544068631896,
0.945084568564882));
#38632=CARTESIAN_POINT('Ctrl Pts',(0.229626061120593,-0.0250343120523647,
0.956203210547999));
#38633=CARTESIAN_POINT('Ctrl Pts',(0.145490988438074,0.179407953322179,
0.967321852531115));
#38634=CARTESIAN_POINT('Ctrl Pts',(-0.0719201283577143,0.219504763615053,
0.978440494514231));
#38635=CARTESIAN_POINT('Ctrl Pts',(-0.22344931264651,0.0585256616254353,
0.989559136497349));
#38636=CARTESIAN_POINT('Ctrl Pts',(-0.170289184396906,-0.156065436285928,
1.00067777848046));
#38637=CARTESIAN_POINT('Ctrl Pts',(0.0388631330803271,-0.227693917494037,
1.01179642046358));
#38638=CARTESIAN_POINT('Ctrl Pts',(0.21241530878674,-0.0907447137301155,
1.0229150624467));
#38639=CARTESIAN_POINT('Ctrl Pts',(0.191385514681521,0.129330245229283,
1.03403370442981));
#38640=CARTESIAN_POINT('Ctrl Pts',(-0.00496108271125438,0.230933734912719,
1.04515234641293));
#38641=CARTESIAN_POINT('Ctrl Pts',(-0.196764314760194,0.120990674417448,
1.05627098839605));
#38642=CARTESIAN_POINT('Ctrl Pts',(-0.208320610464741,-0.0997827509202423,
1.06738963037916));
#38643=CARTESIAN_POINT('Ctrl Pts',(-0.0290505442625618,-0.229155305943203,
1.07850827236228));
#38644=CARTESIAN_POINT('Ctrl Pts',(0.17683937169233,-0.148603171255794,
1.08962691434539));
#38645=CARTESIAN_POINT('Ctrl Pts',(0.220720967111538,0.0680597564112484,
1.10074555632851));
#38646=CARTESIAN_POINT('Ctrl Pts',(0.0624426335084105,0.222407759459687,
1.11186419831163));
#38647=CARTESIAN_POINT('Ctrl Pts',(-0.153093107010227,0.172962013887028,
1.12298284029474));
#38648=CARTESIAN_POINT('Ctrl Pts',(-0.228279649924591,-0.0348126912135875,
1.13410148227786));
#38649=CARTESIAN_POINT('Ctrl Pts',(-0.0945626503816835,-0.210911975270116,
1.14522012426097));
#38650=CARTESIAN_POINT('Ctrl Pts',(0.126200083066393,-0.193383031585166,
1.15633876624409));
#38651=CARTESIAN_POINT('Ctrl Pts',(0.195657378287586,-0.0642246683396576,
1.16375119423284));
#38652=CARTESIAN_POINT('Ctrl Pts',(0.195398449819998,0.00077833665056624,
1.16745740822721));
#38653=CARTESIAN_POINT('Ctrl Pts',(-0.195093054978418,-5.50606481354719E-5,
1.06241303078758));
#38654=CARTESIAN_POINT('Ctrl Pts',(-0.195166977968097,-0.0292567552961119,
1.0640718973181));
#38655=CARTESIAN_POINT('Ctrl Pts',(-0.189027401228485,-0.0584289311968449,
1.06573076384863));
#38656=CARTESIAN_POINT('Ctrl Pts',(-0.17651621681362,-0.0845492725344543,
1.06738963037916));
#38657=CARTESIAN_POINT('Ctrl Pts',(-0.148563921730681,-0.142906935927896,
1.07109584437353));
#38658=CARTESIAN_POINT('Ctrl Pts',(-0.0888072329966215,-0.18603112093555,
1.07480205836791));
#38659=CARTESIAN_POINT('Ctrl Pts',(-0.0246139026371096,-0.194167857658142,
1.07850827236228));
#38660=CARTESIAN_POINT('Ctrl Pts',(0.0395794277224022,-0.202304594380734,
1.08221448635665));
#38661=CARTESIAN_POINT('Ctrl Pts',(0.108209399707366,-0.175453882818264,
1.08592070035102));
#38662=CARTESIAN_POINT('Ctrl Pts',(0.149837984936383,-0.125918039092522,
1.08962691434539));
#38663=CARTESIAN_POINT('Ctrl Pts',(0.191466570165399,-0.0763821953667804,
1.09333312833977));
#38664=CARTESIAN_POINT('Ctrl Pts',(0.206093768638468,-0.0041612194777677,
1.09703934233414));
#38665=CARTESIAN_POINT('Ctrl Pts',(0.187027645607817,0.0576739356414784,
1.10074555632851));
#38666=CARTESIAN_POINT('Ctrl Pts',(0.180418088670294,0.0791100177355746,
1.10203037088567));
#38667=CARTESIAN_POINT('Ctrl Pts',(0.169759382901609,0.0992979671982257,
1.10331518544284));
#38668=CARTESIAN_POINT('Ctrl Pts',(0.156057659382855,0.117255425406022,
1.1046));
#38669=CARTESIAN_POINT('Ctrl Pts',(-0.09055496143049,-0.12679201530598,
5.09575021068187E-18));
#38670=CARTESIAN_POINT('Ctrl Pts',(-0.0937460871048188,-0.125085822491965,
4.58984227758833E-18));
#38671=CARTESIAN_POINT('Ctrl Pts',(-0.0968677330061127,-0.123263760516135,
2.50662287286079E-17));
#38672=CARTESIAN_POINT('Ctrl Pts',(-0.0999128467894991,-0.121327242330634,
2.00577401909818E-17));
#38673=CARTESIAN_POINT('Ctrl Pts',(-0.107335152566795,-0.11660708041271,
6.42545598945985E-18));
#38674=CARTESIAN_POINT('Ctrl Pts',(-0.11430344392066,-0.111208610599775,
9.99023806675092E-18));
#38675=CARTESIAN_POINT('Ctrl Pts',(-0.120790707516777,-0.105232728283189,
2.60208521396521E-17));
#38676=CARTESIAN_POINT('Ctrl Pts',(-0.123891078118351,-0.102376755255687,
3.36821478247169E-17));
#38677=CARTESIAN_POINT('Ctrl Pts',(-0.126881418116351,-0.099388034385428,
-1.92452104322545E-17));
#38678=CARTESIAN_POINT('Ctrl Pts',(-0.129748204847616,-0.0962880923092239,
-1.51788304147971E-17));
#38679=CARTESIAN_POINT('Ctrl Pts',(-0.135037647654988,-0.0905684598931024,
-7.67604539740766E-18));
#38680=CARTESIAN_POINT('Ctrl Pts',(-0.139916189540312,-0.0844627163539483,
6.65058155921973E-18));
#38681=CARTESIAN_POINT('Ctrl Pts',(-0.144364609008094,-0.0780350740853688,
-6.07153216591882E-18));
#38682=CARTESIAN_POINT('Ctrl Pts',(-0.146693883418799,-0.0746694421422029,
-1.2733065360948E-17));
#38683=CARTESIAN_POINT('Ctrl Pts',(-0.148905919766188,-0.0712140221787596,
5.51914947350105E-18));
#38684=CARTESIAN_POINT('Ctrl Pts',(-0.150994732263837,-0.0676811328914676,
3.46944695195361E-18));
#38685=CARTESIAN_POINT('Ctrl Pts',(-0.156930492501974,-0.0576417522477531,
-2.35517480854577E-18));
#38686=CARTESIAN_POINT('Ctrl Pts',(-0.161837586723136,-0.04704232833817,
1.0498384979768E-17));
#38687=CARTESIAN_POINT('Ctrl Pts',(-0.165656700638674,-0.0360824270657778,
6.93889390390723E-18));
#38688=CARTESIAN_POINT('Ctrl Pts',(-0.168566598677898,-0.0277317478433351,
4.22681033390876E-18));
#38689=CARTESIAN_POINT('Ctrl Pts',(-0.17084455406887,-0.0191704748820838,
-1.37633633951559E-17));
#38690=CARTESIAN_POINT('Ctrl Pts',(-0.172449224480544,-0.0104741012692795,
-1.56125112837913E-17));
#38691=CARTESIAN_POINT('Ctrl Pts',(-0.173092222694612,-0.00698942761839798,
-1.63534726558537E-17));
#38692=CARTESIAN_POINT('Ctrl Pts',(-0.173626618765139,-0.00348302750915761,
-1.21488779396688E-17));
#38693=CARTESIAN_POINT('Ctrl Pts',(-0.174048178602262,2.59546856150664E-5,
-1.38777878078145E-17));
#38694=CARTESIAN_POINT('Ctrl Pts',(-0.174866886128293,0.00684071709555691,
-1.72354879401115E-17));
#38695=CARTESIAN_POINT('Ctrl Pts',(-0.175263001859704,0.0136781916586682,
-1.47570089434246E-17));
#38696=CARTESIAN_POINT('Ctrl Pts',(-0.175222496230419,0.020502014676713,
-1.73472347597681E-17));
#38697=CARTESIAN_POINT('Ctrl Pts',(-0.175176789703203,0.0282020123806742,
-2.02700439806174E-17));
#38698=CARTESIAN_POINT('Ctrl Pts',(-0.174575488437737,0.0358847565960055,
-4.14656083691159E-17));
#38699=CARTESIAN_POINT('Ctrl Pts',(-0.173454133268089,0.0435109284941294,
-3.81639164714898E-17));
#38700=CARTESIAN_POINT('Ctrl Pts',(-0.172772227559337,0.0481484691182048,
-3.61561292739328E-17));
#38701=CARTESIAN_POINT('Ctrl Pts',(-0.171897804056446,0.0527651363053484,
-4.88916554017709E-17));
#38702=CARTESIAN_POINT('Ctrl Pts',(-0.170837068741884,0.0573521982187067,
-5.03069808033274E-17));
#38703=CARTESIAN_POINT('Ctrl Pts',(-0.170031029630167,0.0608378475218587,
-5.1382468357856E-17));
#38704=CARTESIAN_POINT('Ctrl Pts',(-0.169117246541092,0.0643057763689402,
-8.52354934901958E-18));
#38705=CARTESIAN_POINT('Ctrl Pts',(-0.168102750715484,0.0677391082731898,
-8.67361737988404E-18));
#38706=CARTESIAN_POINT('Ctrl Pts',(-0.164848133533702,0.0787536247692379,
-9.1550525709997E-18));
#38707=CARTESIAN_POINT('Ctrl Pts',(-0.160552714845615,0.0894467883889295,
-1.4615508474092E-17));
#38708=CARTESIAN_POINT('Ctrl Pts',(-0.155326482610649,0.0996955319262882,
-3.12250225675825E-17));
#38709=CARTESIAN_POINT('Ctrl Pts',(-0.152120282364142,0.105982953261303,
-4.14146631703528E-17));
#38710=CARTESIAN_POINT('Ctrl Pts',(-0.148562901683281,0.112103241720107,
-3.61201279282247E-17));
#38711=CARTESIAN_POINT('Ctrl Pts',(-0.144672442230625,0.118026999364952,
-4.16333634234434E-17));
#38712=CARTESIAN_POINT('Ctrl Pts',(-0.141744976772053,0.122484466690154,
-4.57819239401724E-17));
#38713=CARTESIAN_POINT('Ctrl Pts',(-0.138624730042886,0.126835138052646,
-6.23512024481927E-18));
#38714=CARTESIAN_POINT('Ctrl Pts',(-0.135339728450536,0.131039395408961,
-6.93889390390723E-18));
#38715=CARTESIAN_POINT('Ctrl Pts',(-0.127443588741529,0.141145144987709,
-8.63055065945266E-18));
#38716=CARTESIAN_POINT('Ctrl Pts',(-0.118584883784043,0.150432575075823,
-5.34207396488032E-18));
#38717=CARTESIAN_POINT('Ctrl Pts',(-0.108881311648901,0.158738497602418,
0.));
#38718=CARTESIAN_POINT('Ctrl Pts',(-0.101751737768341,0.16484116654483,
3.92501961933201E-18));
#38719=CARTESIAN_POINT('Ctrl Pts',(-0.0941648935161059,0.170414009123921,
-1.10648570806265E-17));
#38720=CARTESIAN_POINT('Ctrl Pts',(-0.0861525859670525,0.175382131162755,
-1.38777878078145E-17));
#38721=CARTESIAN_POINT('Origin',(0.,0.,0.));
#38722=CARTESIAN_POINT('Origin',(-0.0866025403784439,-0.15,-0.4));
#38723=CARTESIAN_POINT('',(-0.0866025403784439,-0.15,-0.4));
#38724=CARTESIAN_POINT('',(0.0866025403784439,-0.15,-0.4));
#38725=CARTESIAN_POINT('',(-0.043301270189222,-0.15,-0.4));
#38726=CARTESIAN_POINT('',(-0.0866025403784439,-0.15,-0.2));
#38727=CARTESIAN_POINT('',(-0.0866025403784439,-0.15,-0.4));
#38728=CARTESIAN_POINT('',(0.0866025403784439,-0.15,-0.2));
#38729=CARTESIAN_POINT('',(-0.0866025403784439,-0.15,-0.2));
#38730=CARTESIAN_POINT('',(0.0866025403784439,-0.15,-0.4));
#38731=CARTESIAN_POINT('Origin',(-0.173205080756888,2.12115047744981E-17,
-0.4));
#38732=CARTESIAN_POINT('',(-0.173205080756888,2.12115047744981E-17,-0.4));
#38733=CARTESIAN_POINT('',(-0.151554445662277,-0.0375,-0.4));
#38734=CARTESIAN_POINT('',(-0.173205080756888,2.77555756156289E-17,-0.2));
#38735=CARTESIAN_POINT('',(-0.173205080756888,2.12115047744981E-17,-0.4));
#38736=CARTESIAN_POINT('',(-0.173205080756888,2.12115047744981E-17,-0.2));
#38737=CARTESIAN_POINT('Origin',(-0.0866025403784438,0.15,-0.4));
#38738=CARTESIAN_POINT('',(-0.0866025403784438,0.15,-0.4));
#38739=CARTESIAN_POINT('',(-0.108253175473055,0.1125,-0.4));
#38740=CARTESIAN_POINT('',(-0.0866025403784438,0.15,-0.2));
#38741=CARTESIAN_POINT('',(-0.0866025403784438,0.15,-0.4));
#38742=CARTESIAN_POINT('',(-0.0866025403784438,0.15,-0.2));
#38743=CARTESIAN_POINT('Origin',(0.0866025403784439,0.15,-0.4));
#38744=CARTESIAN_POINT('',(0.0866025403784439,0.15,-0.4));
#38745=CARTESIAN_POINT('',(0.043301270189222,0.15,-0.4));
#38746=CARTESIAN_POINT('',(0.0866025403784439,0.15,-0.2));
#38747=CARTESIAN_POINT('',(0.0866025403784439,0.15,-0.4));
#38748=CARTESIAN_POINT('',(0.0866025403784439,0.15,-0.2));
#38749=CARTESIAN_POINT('Origin',(0.173205080756888,0.,-0.4));
#38750=CARTESIAN_POINT('',(0.173205080756888,0.,-0.4));
#38751=CARTESIAN_POINT('',(0.151554445662277,0.0375,-0.4));
#38752=CARTESIAN_POINT('',(0.173205080756888,0.,-0.2));
#38753=CARTESIAN_POINT('',(0.173205080756888,0.,-0.4));
#38754=CARTESIAN_POINT('',(0.173205080756888,0.,-0.2));
#38755=CARTESIAN_POINT('Origin',(0.0866025403784439,-0.15,-0.4));
#38756=CARTESIAN_POINT('',(0.108253175473055,-0.1125,-0.4));
#38757=CARTESIAN_POINT('',(0.0866025403784439,-0.15,-0.2));
#38758=CARTESIAN_POINT('Origin',(0.,2.77555756156289E-17,-0.2));
#38759=CARTESIAN_POINT('Origin',(0.,0.,0.));
#38760=CARTESIAN_POINT('',(-0.35,-4.28626379701574E-17,0.));
#38761=CARTESIAN_POINT('Origin',(0.,0.,0.));
#38762=CARTESIAN_POINT('Origin',(0.,0.,-0.4));
#38763=CARTESIAN_POINT('',(-0.35,-4.28626379701574E-17,-0.4));
#38764=CARTESIAN_POINT('',(-0.35,-4.28626379701574E-17,-0.4));
#38765=CARTESIAN_POINT('Origin',(0.,0.,-0.4));
#38766=CARTESIAN_POINT('Origin',(0.,0.,-0.4));
#38767=CARTESIAN_POINT('Origin',(0.,0.,1.2));
#38768=CARTESIAN_POINT('',(0.,0.,0.));
#38769=CARTESIAN_POINT('Origin',(0.,0.,0.));
#38770=CARTESIAN_POINT('',(-0.146530139441781,9.2983754875535E-5,0.0160655045842905));
#38771=CARTESIAN_POINT('',(-0.146482381647069,0.000161727750000726,0.00893449541570906));
#38772=CARTESIAN_POINT('',(-0.14635,-1.79227059055215E-17,0.));
#38773=CARTESIAN_POINT('',(0.0634007094575212,0.131904027763685,0.));
#38774=CARTESIAN_POINT('Ctrl Pts',(-0.146530139441781,9.2983754875535E-5,
0.0160655045842905));
#38775=CARTESIAN_POINT('Ctrl Pts',(-0.146562770122328,0.00491041321584185,
0.015802617364053));
#38776=CARTESIAN_POINT('Ctrl Pts',(-0.146345876989778,0.00972466734833348,
0.0155397301438155));
#38777=CARTESIAN_POINT('Ctrl Pts',(-0.145869825450435,0.0145129075872385,
0.015276842923578));
#38778=CARTESIAN_POINT('Ctrl Pts',(-0.141074879536054,0.0627416203906926,
0.0126289573514387));
#38779=CARTESIAN_POINT('Ctrl Pts',(-0.109987863649871,0.10833117855941,
0.00998107177929941));
#38780=CARTESIAN_POINT('Ctrl Pts',(-0.0668435938445389,0.130448755664999,
0.00733318620716011));
#38781=CARTESIAN_POINT('Ctrl Pts',(-0.0270149638383408,0.150866595604039,
0.00488879080477341));
#38782=CARTESIAN_POINT('Ctrl Pts',(0.0230889279919825,0.151281476944728,
0.00244439540238672));
#38783=CARTESIAN_POINT('Ctrl Pts',(0.0635548502597316,0.132093933345895,
1.98375346423187E-17));
#38784=CARTESIAN_POINT('',(-0.0634007094575231,0.131904027763684,0.));
#38785=CARTESIAN_POINT('Origin',(0.,0.,0.));
#38786=CARTESIAN_POINT('Ctrl Pts',(-0.063400709457523,0.131904027763684,
7.63278329429795E-17));
#38787=CARTESIAN_POINT('Ctrl Pts',(-0.107339749959442,0.110784382003545,
0.00265083470503432));
#38788=CARTESIAN_POINT('Ctrl Pts',(-0.139511904869873,0.0661645412785542,
0.00530166941006857));
#38789=CARTESIAN_POINT('Ctrl Pts',(-0.145460797893518,0.0180856147189845,
0.00795250411510281));
#38790=CARTESIAN_POINT('Ctrl Pts',(-0.146195379242097,0.0121487315761866,
0.00827983454863823));
#38791=CARTESIAN_POINT('Ctrl Pts',(-0.146530113272026,0.00615910494930538,
0.00860716498217364));
#38792=CARTESIAN_POINT('Ctrl Pts',(-0.146482381647069,0.000161727750000726,
0.00893449541570906));
#38793=CARTESIAN_POINT('Origin',(0.,0.,0.));
#38794=CARTESIAN_POINT('',(-0.146153148300412,8.02585168747302E-5,0.0660655045842906));
#38795=CARTESIAN_POINT('',(-0.146138869890956,7.0051777900314E-5,0.058934495415709));
#38796=CARTESIAN_POINT('',(-0.14635,-1.79227059055215E-17,0.));
#38797=CARTESIAN_POINT('Ctrl Pts',(-0.146153148300412,8.02585168747302E-5,
0.0660655045842906));
#38798=CARTESIAN_POINT('Ctrl Pts',(-0.146248563607689,0.0193075654691076,
0.0650232641302222));
#38799=CARTESIAN_POINT('Ctrl Pts',(-0.142725320554989,0.0385012587497889,
0.0639810236761539));
#38800=CARTESIAN_POINT('Ctrl Pts',(-0.135419901199499,0.0561272788093185,
0.0629387832220855));
#38801=CARTESIAN_POINT('Ctrl Pts',(-0.116859966748363,0.100907429136131,
0.0602908976499462));
#38802=CARTESIAN_POINT('Ctrl Pts',(-0.0738879770866151,0.13556903337647,
0.0576430120778069));
#38803=CARTESIAN_POINT('Ctrl Pts',(-0.0261938646990992,0.144231038496032,
0.0549951265056676));
#38804=CARTESIAN_POINT('Ctrl Pts',(0.0215002476884163,0.152893043615593,
0.0523472409335283));
#38805=CARTESIAN_POINT('Ctrl Pts',(0.0739164828016995,0.135555449614377,
0.049699355361389));
#38806=CARTESIAN_POINT('Ctrl Pts',(0.107036887564708,0.100160226311824,
0.0470514697892497));
#38807=CARTESIAN_POINT('Ctrl Pts',(0.140157292327717,0.0647650030092702,
0.0444035842171104));
#38808=CARTESIAN_POINT('Ctrl Pts',(0.153981866740452,0.0113121504053791,
0.0417556986449711));
#38809=CARTESIAN_POINT('Ctrl Pts',(0.142176802105062,-0.0357014716925755,
0.0391078130728318));
#38810=CARTESIAN_POINT('Ctrl Pts',(0.130371737469673,-0.0827150937905301,
0.0364599275006924));
#38811=CARTESIAN_POINT('Ctrl Pts',(0.0929370337861598,-0.123289485382548,
0.0338120419285532));
#38812=CARTESIAN_POINT('Ctrl Pts',(0.047024206385633,-0.138841291698229,
0.0311641563564138));
#38813=CARTESIAN_POINT('Ctrl Pts',(0.0011113789851062,-0.15439309801391,
0.0285162707842745));
#38814=CARTESIAN_POINT('Ctrl Pts',(-0.0532795721324345,-0.144922319053254,
0.0258683852121352));
#38815=CARTESIAN_POINT('Ctrl Pts',(-0.091223609719915,-0.11475299585383,
0.0232204996399959));
#38816=CARTESIAN_POINT('Ctrl Pts',(-0.125400489590719,-0.0875789416327165,
0.0208355012880941));
#38817=CARTESIAN_POINT('Ctrl Pts',(-0.146234103296486,-0.0436123029244358,
0.0184505029361923));
#38818=CARTESIAN_POINT('Ctrl Pts',(-0.146530139441781,9.2983754875535E-5,
0.0160655045842905));
#38819=CARTESIAN_POINT('Ctrl Pts',(-0.146482381647069,0.000161727750000726,
0.00893449541570906));
#38820=CARTESIAN_POINT('Ctrl Pts',(-0.146143566116611,-0.0424097233364945,
0.0112579996872079));
#38821=CARTESIAN_POINT('Ctrl Pts',(-0.126533645440834,-0.0853716986287587,
0.0135815039587068));
#38822=CARTESIAN_POINT('Ctrl Pts',(-0.0938693583126354,-0.112632000129883,
0.0159050082302056));
#38823=CARTESIAN_POINT('Ctrl Pts',(-0.0566033945712489,-0.143732676025031,
0.0185558429352399));
#38824=CARTESIAN_POINT('Ctrl Pts',(-0.00234583595161722,-0.154396015421179,
0.0212066776402742));
#38825=CARTESIAN_POINT('Ctrl Pts',(0.0439541262059228,-0.139833200290426,
0.0238575123453084));
#38826=CARTESIAN_POINT('Ctrl Pts',(0.0902540883634627,-0.125270385159674,
0.0265083470503427));
#38827=CARTESIAN_POINT('Ctrl Pts',(0.128596454058911,-0.0854814155020214,
0.029159181755377));
#38828=CARTESIAN_POINT('Ctrl Pts',(0.141395806078876,-0.0386806767328055,
0.0318100164604112));
#38829=CARTESIAN_POINT('Ctrl Pts',(0.154195158098842,0.00812006203641059,
0.0344608511654455));
#38830=CARTESIAN_POINT('Ctrl Pts',(0.141451496443324,0.0619325699171903,
0.0371116858704798));
#38831=CARTESIAN_POINT('Ctrl Pts',(0.109005912554766,0.0980207644158424,
0.0397625205755141));
#38832=CARTESIAN_POINT('Ctrl Pts',(0.0765603286662091,0.134108958914494,
0.0424133552805484));
#38833=CARTESIAN_POINT('Ctrl Pts',(0.0244128225446121,0.152472840031019,
0.0450641899855826));
#38834=CARTESIAN_POINT('Ctrl Pts',(-0.0234881253671046,0.144695681732891,
0.0477150246906169));
#38835=CARTESIAN_POINT('Ctrl Pts',(-0.0713890732788212,0.136918523434763,
0.0503658593956511));
#38836=CARTESIAN_POINT('Ctrl Pts',(-0.115043462980658,0.103000325721984,
0.0530166941006854));
#38837=CARTESIAN_POINT('Ctrl Pts',(-0.134410456092164,0.0585065536587812,
0.0556675288057197));
#38838=CARTESIAN_POINT('Ctrl Pts',(-0.142366606622288,0.0402280761403725,
0.0567565176757161));
#38839=CARTESIAN_POINT('Ctrl Pts',(-0.14622390219053,0.0201648150927879,
0.0578455065457126));
#38840=CARTESIAN_POINT('Ctrl Pts',(-0.146138869890956,7.0051777900314E-5,
0.058934495415709));
#38841=CARTESIAN_POINT('Origin',(0.,0.,0.));
#38842=CARTESIAN_POINT('',(-0.146239229308481,-0.000121680145597616,0.116065504584291));
#38843=CARTESIAN_POINT('',(-0.146251911109041,-0.00012571917928438,0.108934495415709));
#38844=CARTESIAN_POINT('',(-0.14635,-1.79227059055215E-17,0.));
#38845=CARTESIAN_POINT('Ctrl Pts',(-0.146239229308481,-0.000121680145597616,
0.116065504584291));
#38846=CARTESIAN_POINT('Ctrl Pts',(-0.145975985392548,0.0334333989639988,
0.114243910896391));
#38847=CARTESIAN_POINT('Ctrl Pts',(-0.134505001919181,0.0671510842014817,
0.112422317208492));
#38848=CARTESIAN_POINT('Ctrl Pts',(-0.113362446108109,0.09293957845923,
0.110600723520593));
#38849=CARTESIAN_POINT('Ctrl Pts',(-0.0826294298146382,0.130425974204838,
0.107952837948454));
#38850=CARTESIAN_POINT('Ctrl Pts',(-0.0314605739124977,0.151158147427946,
0.105304952376314));
#38851=CARTESIAN_POINT('Ctrl Pts',(0.0166981167953111,0.145636463652384,
0.102657066804175));
#38852=CARTESIAN_POINT('Ctrl Pts',(0.0648568075031199,0.140114779876822,
0.100009181232036));
#38853=CARTESIAN_POINT('Ctrl Pts',(0.110005333016597,0.10833923910259,0.0973612956598965));
#38854=CARTESIAN_POINT('Ctrl Pts',(0.1314562431614,0.0648696188566969,0.0947134100877572));
#38855=CARTESIAN_POINT('Ctrl Pts',(0.152907153306203,0.0213999986108032,
0.0920655245156179));
#38856=CARTESIAN_POINT('Ctrl Pts',(0.150660448082332,-0.0337637011067522,
0.0894176389434786));
#38857=CARTESIAN_POINT('Ctrl Pts',(0.125745602608234,-0.075344908113871,
0.0867697533713393));
#38858=CARTESIAN_POINT('Ctrl Pts',(0.100830757134136,-0.11692611512099,
0.0841218677992));
#38859=CARTESIAN_POINT('Ctrl Pts',(0.053247771409812,-0.144924829417672,
0.0814739822270607));
#38860=CARTESIAN_POINT('Ctrl Pts',(0.00479954857812182,-0.146511973337632,
0.0788260966549214));
#38861=CARTESIAN_POINT('Ctrl Pts',(-0.0436486742535683,-0.148099117257592,
0.0761782110827821));
#38862=CARTESIAN_POINT('Ctrl Pts',(-0.0929621341926243,-0.123274690800829,
0.0735303255106428));
#38863=CARTESIAN_POINT('Ctrl Pts',(-0.120544924541891,-0.0834131293658051,
0.0708824399385034));
#38864=CARTESIAN_POINT('Ctrl Pts',(-0.137270788050899,-0.059241570673742,
0.0692767948204325));
#38865=CARTESIAN_POINT('Ctrl Pts',(-0.146006154272575,-0.0295407674383123,
0.0676711497023615));
#38866=CARTESIAN_POINT('Ctrl Pts',(-0.146153148300412,8.02585168747302E-5,
0.0660655045842906));
#38867=CARTESIAN_POINT('Ctrl Pts',(-0.146138869890956,7.0051777900314E-5,
0.058934495415709));
#38868=CARTESIAN_POINT('Ctrl Pts',(-0.14601691516158,-0.0287501898739087,
0.0604963412507468));
#38869=CARTESIAN_POINT('Ctrl Pts',(-0.137785682499354,-0.0576352309664648,
0.0620581870857847));
#38870=CARTESIAN_POINT('Ctrl Pts',(-0.121906950385236,-0.0814126279516829,
0.0636200329208225));
#38871=CARTESIAN_POINT('Ctrl Pts',(-0.0949568550456235,-0.121768691085319,
0.0662708676258568));
#38872=CARTESIAN_POINT('Ctrl Pts',(-0.0459770678452217,-0.147411470938967,
0.068921702330891));
#38873=CARTESIAN_POINT('Ctrl Pts',(0.00254289383979588,-0.146569427669784,
0.0715725370359253));
#38874=CARTESIAN_POINT('Ctrl Pts',(0.0510628555248136,-0.145727384400601,
0.0742233717409596));
#38875=CARTESIAN_POINT('Ctrl Pts',(0.0991229916944473,-0.118400518008588,
0.0768742064459939));
#38876=CARTESIAN_POINT('Ctrl Pts',(0.124657213858417,-0.0771346353870958,
0.0795250411510281));
#38877=CARTESIAN_POINT('Ctrl Pts',(0.150191436022387,-0.0358687527656039,
0.0821758758560624));
#38878=CARTESIAN_POINT('Ctrl Pts',(0.153199744180694,0.0193361460853669,
0.0848267105610966));
#38879=CARTESIAN_POINT('Ctrl Pts',(0.132300679968259,0.0631324945868766,
0.0874775452661308));
#38880=CARTESIAN_POINT('Ctrl Pts',(0.111401615755824,0.106928843088387,
0.0901283799711651));
#38881=CARTESIAN_POINT('Ctrl Pts',(0.0665951791726482,0.139316641240435,
0.0927792146761994));
#38882=CARTESIAN_POINT('Ctrl Pts',(0.0184540622028837,0.145425561817519,
0.0954300493812337));
#38883=CARTESIAN_POINT('Ctrl Pts',(-0.0296870547668806,0.151534482394603,
0.098080884086268));
#38884=CARTESIAN_POINT('Ctrl Pts',(-0.0811628521232332,0.131364525396722,
0.100731718791302));
#38885=CARTESIAN_POINT('Ctrl Pts',(-0.11233861635763,0.0941764269143644,
0.103382553496337));
#38886=CARTESIAN_POINT('Ctrl Pts',(-0.134103588725605,0.0682140181085839,
0.105233200802794));
#38887=CARTESIAN_POINT('Ctrl Pts',(-0.145974404722175,0.0339570340187871,
0.107083848109252));
#38888=CARTESIAN_POINT('Ctrl Pts',(-0.146251911109041,-0.00012571917928438,
0.108934495415709));
#38889=CARTESIAN_POINT('Origin',(0.,0.,0.));
#38890=CARTESIAN_POINT('',(-0.146588437557148,-1.60561805771647E-5,0.166065504584291));
#38891=CARTESIAN_POINT('',(-0.146590338660816,-1.32548991986104E-5,0.158934495415709));
#38892=CARTESIAN_POINT('',(-0.14635,-1.79227059055215E-17,0.));
#38893=CARTESIAN_POINT('Ctrl Pts',(-0.146588437557148,-1.60561805771647E-5,
0.166065504584291));
#38894=CARTESIAN_POINT('Ctrl Pts',(-0.146514434076835,0.0476007616257437,
0.163464557662561));
#38895=CARTESIAN_POINT('Ctrl Pts',(-0.121147481081461,0.0952852365283555,
0.160863610740831));
#38896=CARTESIAN_POINT('Ctrl Pts',(-0.0815892695913163,0.121786698620987,
0.158262663819101));
#38897=CARTESIAN_POINT('Ctrl Pts',(-0.0413171607723027,0.148766426092319,
0.155614778246961));
#38898=CARTESIAN_POINT('Ctrl Pts',(0.0136630407409267,0.153791672495834,
0.152966892674822));
#38899=CARTESIAN_POINT('Ctrl Pts',(0.0581589346640781,0.134559827321239,
0.150319007102683));
#38900=CARTESIAN_POINT('Ctrl Pts',(0.10265482858723,0.115327982146644,0.147671121530543));
#38901=CARTESIAN_POINT('Ctrl Pts',(0.136666414920303,0.0718390453939375,
0.145023235958404));
#38902=CARTESIAN_POINT('Ctrl Pts',(0.144609292620067,0.0240200202446034,
0.142375350386265));
#38903=CARTESIAN_POINT('Ctrl Pts',(0.152552170319831,-0.0237990049047303,
0.139727464814125));
#38904=CARTESIAN_POINT('Ctrl Pts',(0.134426339386286,-0.0759481184506919,
0.137079579241986));
#38905=CARTESIAN_POINT('Ctrl Pts',(0.0985372115045479,-0.108532146892156,
0.134431693669847));
#38906=CARTESIAN_POINT('Ctrl Pts',(0.06264808362281,-0.141116175333621,
0.131783808097708));
#38907=CARTESIAN_POINT('Ctrl Pts',(0.00899565879287956,-0.154135118670589,
0.129135922525568));
#38908=CARTESIAN_POINT('Ctrl Pts',(-0.0378360619111076,-0.141623588974912,
0.126488036953429));
#38909=CARTESIAN_POINT('Ctrl Pts',(-0.0846677826150948,-0.129112059279235,
0.12384015138129));
#38910=CARTESIAN_POINT('Ctrl Pts',(-0.124678799193139,-0.0910700565509135,
0.12119226580915));
#38911=CARTESIAN_POINT('Ctrl Pts',(-0.13953571913976,-0.0449287460526992,
0.118544380237011));
#38912=CARTESIAN_POINT('Ctrl Pts',(-0.144171928689699,-0.0305300156868414,
0.117718088352771));
#38913=CARTESIAN_POINT('Ctrl Pts',(-0.146358639203649,-0.0153425769501271,
0.116891796468531));
#38914=CARTESIAN_POINT('Ctrl Pts',(-0.146239229308481,-0.000121680145597616,
0.116065504584291));
#38915=CARTESIAN_POINT('Ctrl Pts',(-0.146251911109041,-0.00012571917928438,
0.108934495415709));
#38916=CARTESIAN_POINT('Ctrl Pts',(-0.146371899997805,-0.01486250318061,
0.109734682814286));
#38917=CARTESIAN_POINT('Ctrl Pts',(-0.144324466618943,-0.0295667139196708,
0.110534870212863));
#38918=CARTESIAN_POINT('Ctrl Pts',(-0.139972258433256,-0.0435537680369422,
0.111335057611439));
#38919=CARTESIAN_POINT('Ctrl Pts',(-0.125554405162046,-0.0898896245390587,
0.113985892316474));
#38920=CARTESIAN_POINT('Ctrl Pts',(-0.0858429675071836,-0.128355097576459,
0.116636727021508));
#38921=CARTESIAN_POINT('Ctrl Pts',(-0.0390712063381835,-0.141289065177804,
0.119287561726542));
#38922=CARTESIAN_POINT('Ctrl Pts',(0.00770055483081633,-0.15422303277915,
0.121938396431576));
#38923=CARTESIAN_POINT('Ctrl Pts',(0.061532639513954,-0.141625494944442,
0.124589231136611));
#38924=CARTESIAN_POINT('Ctrl Pts',(0.0977084099269336,-0.109280503770194,
0.127240065841645));
#38925=CARTESIAN_POINT('Ctrl Pts',(0.133884180339913,-0.0769355125959451,
0.129890900546679));
#38926=CARTESIAN_POINT('Ctrl Pts',(0.152403636482735,-0.024843068082156,
0.132541735251714));
#38927=CARTESIAN_POINT('Ctrl Pts',(0.144763687764892,0.0230789149168219,
0.135192569956748));
#38928=CARTESIAN_POINT('Ctrl Pts',(0.137123739047049,0.0710008979157997,
0.137843404661782));
#38929=CARTESIAN_POINT('Ctrl Pts',(0.103324385468542,0.114752419399967,
0.140494239366816));
#38930=CARTESIAN_POINT('Ctrl Pts',(0.058884379534592,0.134245263752326,
0.143145074071851));
#38931=CARTESIAN_POINT('Ctrl Pts',(0.0144443736006417,0.153738108104685,
0.145795908776885));
#38932=CARTESIAN_POINT('Ctrl Pts',(-0.0406362846887521,0.148972275325237,
0.148446743481919));
#38933=CARTESIAN_POINT('Ctrl Pts',(-0.0810676758629916,0.122135962547369,
0.151097578186953));
#38934=CARTESIAN_POINT('Ctrl Pts',(-0.120911410803562,0.0956897062586433,
0.153709883929872));
#38935=CARTESIAN_POINT('Ctrl Pts',(-0.146528627904579,0.0478098809758598,
0.15632218967279));
#38936=CARTESIAN_POINT('Ctrl Pts',(-0.146590338660816,-1.32548991986104E-5,
0.158934495415709));
#38937=CARTESIAN_POINT('Origin',(0.,0.,0.));
#38938=CARTESIAN_POINT('',(-0.146286659309134,0.000131086592791319,0.21606550458429));
#38939=CARTESIAN_POINT('',(-0.146291727422766,0.000132510687651112,0.208934495415709));
#38940=CARTESIAN_POINT('',(-0.14635,-1.79227059055215E-17,0.));
#38941=CARTESIAN_POINT('Ctrl Pts',(-0.146286659309134,0.000131086592791319,
0.21606550458429));
#38942=CARTESIAN_POINT('Ctrl Pts',(-0.146403448836959,0.0136116234039521,
0.215333090000869));
#38943=CARTESIAN_POINT('Ctrl Pts',(-0.144693388849564,0.0270630787330369,
0.214600675417447));
#38944=CARTESIAN_POINT('Ctrl Pts',(-0.141038079685752,0.0399633448807191,
0.213868260834026));
#38945=CARTESIAN_POINT('Ctrl Pts',(-0.127823104703478,0.0866014503777888,
0.211220375261887));
#38946=CARTESIAN_POINT('Ctrl Pts',(-0.0891832035626152,0.126035366094718,
0.208572489689747));
#38947=CARTESIAN_POINT('Ctrl Pts',(-0.0428235107164534,0.140196133277333,
0.205924604117608));
#38948=CARTESIAN_POINT('Ctrl Pts',(0.00353618212970767,0.154356900459949,
0.203276718545469));
#38949=CARTESIAN_POINT('Ctrl Pts',(0.0576156666811676,0.143244519108251,
0.200628832973329));
#38950=CARTESIAN_POINT('Ctrl Pts',(0.0946352588096336,0.111950777776248,
0.19798094740119));
#38951=CARTESIAN_POINT('Ctrl Pts',(0.1316548509381,0.0806570364442455,0.195333061829051));
#38952=CARTESIAN_POINT('Ctrl Pts',(0.151614550643572,0.0291819351319375,
0.192685176256911));
#38953=CARTESIAN_POINT('Ctrl Pts',(0.145368652149886,-0.0188881928126718,
0.190037290684772));
#38954=CARTESIAN_POINT('Ctrl Pts',(0.1391227536562,-0.0669583207572802,
0.187389405112633));
#38955=CARTESIAN_POINT('Ctrl Pts',(0.106671256963357,-0.11162347533419,
0.184741519540494));
#38956=CARTESIAN_POINT('Ctrl Pts',(0.06288371648092,-0.132417699194711,
0.182093633968354));
#38957=CARTESIAN_POINT('Ctrl Pts',(0.0190961759984827,-0.153211923055232,
0.179445748396215));
#38958=CARTESIAN_POINT('Ctrl Pts',(-0.0360274082735484,-0.150135216199364,
0.176797862824076));
#38959=CARTESIAN_POINT('Ctrl Pts',(-0.0772289367619549,-0.124597352202288,
0.174149977251936));
#38960=CARTESIAN_POINT('Ctrl Pts',(-0.118430465250361,-0.0990594882052125,
0.171502091679797));
#38961=CARTESIAN_POINT('Ctrl Pts',(-0.145709937955143,-0.0510604670669293,
0.168854206107658));
#38962=CARTESIAN_POINT('Ctrl Pts',(-0.146567666245136,-0.00259385222821292,
0.166206320535519));
#38963=CARTESIAN_POINT('Ctrl Pts',(-0.146582871059412,-0.00173469218203314,
0.166159381885109));
#38964=CARTESIAN_POINT('Ctrl Pts',(-0.146589773079785,-0.000875385198767554,
0.1661124432347));
#38965=CARTESIAN_POINT('Ctrl Pts',(-0.146588437557148,-1.60561805771647E-5,
0.166065504584291));
#38966=CARTESIAN_POINT('Ctrl Pts',(-0.146590338660816,-1.32548991986104E-5,
0.158934495415709));
#38967=CARTESIAN_POINT('Ctrl Pts',(-0.146591248834288,-0.000718599514920206,
0.158973024377825));
#38968=CARTESIAN_POINT('Ctrl Pts',(-0.146586599823099,-0.0014239317987834,
0.15901155333994));
#38969=CARTESIAN_POINT('Ctrl Pts',(-0.146576355279203,-0.00212918280121965,
0.159050082302056));
#38970=CARTESIAN_POINT('Ctrl Pts',(-0.14587151946209,-0.0506512225956504,
0.16170091700709));
#38971=CARTESIAN_POINT('Ctrl Pts',(-0.118679723768778,-0.0987885094082227,
0.164351751712125));
#38972=CARTESIAN_POINT('Ctrl Pts',(-0.0774859020747837,-0.12443912668017,
0.167002586417159));
#38973=CARTESIAN_POINT('Ctrl Pts',(-0.0362920803807891,-0.150089743952118,
0.169653421122193));
#38974=CARTESIAN_POINT('Ctrl Pts',(0.0189037673138887,-0.153253691683441,
0.172304255827227));
#38975=CARTESIAN_POINT('Ctrl Pts',(0.0627588320121262,-0.132478263640569,
0.174955090532262));
#38976=CARTESIAN_POINT('Ctrl Pts',(0.106613896710364,-0.111702835597697,
0.177605925237296));
#38977=CARTESIAN_POINT('Ctrl Pts',(0.139128178412161,-0.0669880317806311,
0.18025675994233));
#38978=CARTESIAN_POINT('Ctrl Pts',(0.14537295917033,-0.0188643595177345,
0.182907594647365));
#38979=CARTESIAN_POINT('Ctrl Pts',(0.151617739928498,0.0292593127451622,
0.185558429352399));
#38980=CARTESIAN_POINT('Ctrl Pts',(0.131593019743037,0.0807918534538889,
0.188209264057433));
#38981=CARTESIAN_POINT('Ctrl Pts',(0.0944930167757219,0.11207243679613,
0.190860098762467));
#38982=CARTESIAN_POINT('Ctrl Pts',(0.0573930138084077,0.143353020138371,
0.193510933467502));
#38983=CARTESIAN_POINT('Ctrl Pts',(0.00321772805924021,0.154381646114126,
0.196161768172536));
#38984=CARTESIAN_POINT('Ctrl Pts',(-0.0431586156002514,0.14009459381994,
0.19881260287757));
#38985=CARTESIAN_POINT('Ctrl Pts',(-0.0895349592597434,0.125807541525753,
0.201463437582605));
#38986=CARTESIAN_POINT('Ctrl Pts',(-0.12811236082956,0.086204810961624,
0.204114272287639));
#38987=CARTESIAN_POINT('Ctrl Pts',(-0.141178260973432,0.0394697345298879,
0.206765106992673));
#38988=CARTESIAN_POINT('Ctrl Pts',(-0.144742548661738,0.0267207271363346,
0.207488236467018));
#38989=CARTESIAN_POINT('Ctrl Pts',(-0.146408370233879,0.0134409584703521,
0.208211365941364));
#38990=CARTESIAN_POINT('Ctrl Pts',(-0.146291727422766,0.000132510687651112,
0.208934495415709));
#38991=CARTESIAN_POINT('Origin',(0.,0.,0.));
#38992=CARTESIAN_POINT('',(-0.146128981728208,-5.54263297282837E-5,0.26606550458429));
#38993=CARTESIAN_POINT('',(-0.146122305401386,-4.76483376818115E-5,0.258934495415709));
#38994=CARTESIAN_POINT('',(-0.14635,-1.79227059055215E-17,0.));
#38995=CARTESIAN_POINT('Ctrl Pts',(-0.146128981728208,-5.54263297282837E-5,
0.26606550458429));
#38996=CARTESIAN_POINT('Ctrl Pts',(-0.146034100463789,0.0278452262029135,
0.264553736767038));
#38997=CARTESIAN_POINT('Ctrl Pts',(-0.138353701663978,0.055794258172635,
0.263041968949786));
#38998=CARTESIAN_POINT('Ctrl Pts',(-0.123420870545114,0.0790954965178402,
0.261530201132533));
#38999=CARTESIAN_POINT('Ctrl Pts',(-0.0972657774021095,0.119907989099794,
0.258882315560394));
#39000=CARTESIAN_POINT('Ctrl Pts',(-0.0488616113353708,0.146461941272529,
0.256234429988255));
#39001=CARTESIAN_POINT('Ctrl Pts',(-0.000387576818673938,0.146590104167151,
0.253586544416116));
#39002=CARTESIAN_POINT('Ctrl Pts',(0.0480864576980232,0.146718267061773,
0.250938658843976));
#39003=CARTESIAN_POINT('Ctrl Pts',(0.0966303606646785,0.120420640678281,
0.248290773271837));
#39004=CARTESIAN_POINT('Ctrl Pts',(0.123000898959779,0.0797470232084743,
0.245642887699697));
#39005=CARTESIAN_POINT('Ctrl Pts',(0.149371437254879,0.0390734057386676,
0.242995002127558));
#39006=CARTESIAN_POINT('Ctrl Pts',(0.153568610878424,-0.0159762028174541,
0.240347116555419));
#39007=CARTESIAN_POINT('Ctrl Pts',(0.133669238840564,-0.0601775991819374,
0.23769923098328));
#39008=CARTESIAN_POINT('Ctrl Pts',(0.113769866802704,-0.104378995546421,
0.235051345411141));
#39009=CARTESIAN_POINT('Ctrl Pts',(0.0697739491034383,-0.137732179719266,
0.232403459839001));
#39010=CARTESIAN_POINT('Ctrl Pts',(0.0218407929672104,-0.144954436352131,
0.229755574266862));
#39011=CARTESIAN_POINT('Ctrl Pts',(-0.0260923631690164,-0.152176692984997,
0.227107688694722));
#39012=CARTESIAN_POINT('Ctrl Pts',(-0.0779627577422058,-0.133268022077883,
0.224459803122583));
#39013=CARTESIAN_POINT('Ctrl Pts',(-0.110002930616958,-0.0968925389857218,
0.221811917550444));
#39014=CARTESIAN_POINT('Ctrl Pts',(-0.133180677518425,-0.0705786441192844,
0.219896446561726));
#39015=CARTESIAN_POINT('Ctrl Pts',(-0.145981221709449,-0.0351243244252332,
0.217980975573008));
#39016=CARTESIAN_POINT('Ctrl Pts',(-0.146286659309134,0.000131086592791319,
0.21606550458429));
#39017=CARTESIAN_POINT('Ctrl Pts',(-0.146291727422766,0.000132510687651112,
0.208934495415709));
#39018=CARTESIAN_POINT('Ctrl Pts',(-0.14598078316578,-0.035344904233501,
0.210862200646398));
#39019=CARTESIAN_POINT('Ctrl Pts',(-0.13300294931328,-0.0710261241835679,
0.212789905877087));
#39020=CARTESIAN_POINT('Ctrl Pts',(-0.109555772823034,-0.0973996609618648,
0.214717611107776));
#39021=CARTESIAN_POINT('Ctrl Pts',(-0.0773129858108336,-0.133666557722538,
0.21736844581281));
#39022=CARTESIAN_POINT('Ctrl Pts',(-0.0252730130685043,-0.152332928944543,
0.220019280517844));
#39023=CARTESIAN_POINT('Ctrl Pts',(0.0226703353838526,-0.144828233467297,
0.222670115222879));
#39024=CARTESIAN_POINT('Ctrl Pts',(0.0706136838362102,-0.137323537990051,
0.225320949927913));
#39025=CARTESIAN_POINT('Ctrl Pts',(0.114460407998596,-0.103647775813554,
0.227971784632947));
#39026=CARTESIAN_POINT('Ctrl Pts',(0.134078573855527,-0.0592629508888991,
0.230622619337982));
#39027=CARTESIAN_POINT('Ctrl Pts',(0.153696739712459,-0.014878125964245,
0.233273454043016));
#39028=CARTESIAN_POINT('Ctrl Pts',(0.149086347263938,0.0402157617085659,
0.23592428874805));
#39029=CARTESIAN_POINT('Ctrl Pts',(0.122364227775469,0.080722717223899,
0.238575123453084));
#39030=CARTESIAN_POINT('Ctrl Pts',(0.0956421082870006,0.121229672739232,
0.241225958158119));
#39031=CARTESIAN_POINT('Ctrl Pts',(0.0468082617585844,0.147149696097087,
0.243876792863153));
#39032=CARTESIAN_POINT('Ctrl Pts',(-0.00171557347725478,0.146581779641701,
0.246527627568187));
#39033=CARTESIAN_POINT('Ctrl Pts',(-0.050239408713094,0.146013863186315,
0.249178462273221));
#39034=CARTESIAN_POINT('Ctrl Pts',(-0.0984532326563563,0.118958006917689,
0.251829296978256));
#39035=CARTESIAN_POINT('Ctrl Pts',(-0.124219986251493,0.0778367286753789,
0.25448013168329));
#39036=CARTESIAN_POINT('Ctrl Pts',(-0.13865248336877,0.054803841451165,
0.255964919594096));
#39037=CARTESIAN_POINT('Ctrl Pts',(-0.146042539478052,0.0273581331787701,
0.257449707504903));
#39038=CARTESIAN_POINT('Ctrl Pts',(-0.146122305401386,-4.76483376818114E-5,
0.258934495415709));
#39039=CARTESIAN_POINT('Origin',(0.,0.,0.));
#39040=CARTESIAN_POINT('',(-0.146489966325848,-0.000104789085069334,0.31606550458429));
#39041=CARTESIAN_POINT('',(-0.146466968003471,-0.000114397412080779,0.308934495415709));
#39042=CARTESIAN_POINT('',(-0.14635,-1.79227059055215E-17,0.));
#39043=CARTESIAN_POINT('Ctrl Pts',(-0.146489966325848,-0.000104789085069334,
0.31606550458429));
#39044=CARTESIAN_POINT('Ctrl Pts',(-0.146149966214897,0.0419143941805715,
0.313774383533207));
#39045=CARTESIAN_POINT('Ctrl Pts',(-0.127114021003857,0.084202434124342,
0.311483262482124));
#39046=CARTESIAN_POINT('Ctrl Pts',(-0.09522591597141,0.111448794443947,
0.309192141431041));
#39047=CARTESIAN_POINT('Ctrl Pts',(-0.0583723183850411,0.142937852758646,
0.306544255858902));
#39048=CARTESIAN_POINT('Ctrl Pts',(-0.00435235065556675,0.154336043577878,
0.303896370286762));
#39049=CARTESIAN_POINT('Ctrl Pts',(0.0420815742217502,0.140420618022043,
0.301248484714623));
#39050=CARTESIAN_POINT('Ctrl Pts',(0.0885154990990669,0.126505192466209,
0.298600599142484));
#39051=CARTESIAN_POINT('Ctrl Pts',(0.127363381124227,0.0872761505353081,
0.295952713570344));
#39052=CARTESIAN_POINT('Ctrl Pts',(0.140824787209621,0.0407085760419468,
0.293304827998205));
#39053=CARTESIAN_POINT('Ctrl Pts',(0.154286193295015,-0.00585899845141487,
0.290656942426066));
#39054=CARTESIAN_POINT('Ctrl Pts',(0.142361123440642,-0.0597651055072374,
0.288009056853927));
#39055=CARTESIAN_POINT('Ctrl Pts',(0.110513747042986,-0.0963095040482439,
0.285361171281788));
#39056=CARTESIAN_POINT('Ctrl Pts',(0.07866637064533,-0.13285390258925,0.282713285709648));
#39057=CARTESIAN_POINT('Ctrl Pts',(0.0268966877043911,-0.152036592615441,
0.280065400137508));
#39058=CARTESIAN_POINT('Ctrl Pts',(-0.0210739885810971,-0.145067900862674,
0.277417514565369));
#39059=CARTESIAN_POINT('Ctrl Pts',(-0.0690446648665853,-0.138099209109907,
0.27476962899323));
#39060=CARTESIAN_POINT('Ctrl Pts',(-0.113216334496623,-0.104979135578184,
0.272121743421091));
#39061=CARTESIAN_POINT('Ctrl Pts',(-0.133349159202006,-0.0608835823167352,
0.269473857848951));
#39062=CARTESIAN_POINT('Ctrl Pts',(-0.141987470405663,-0.0419636782623391,
0.268337740094064));
#39063=CARTESIAN_POINT('Ctrl Pts',(-0.146200286519779,-0.0210232140769756,
0.267201622339177));
#39064=CARTESIAN_POINT('Ctrl Pts',(-0.146128981728208,-5.54263297282837E-5,
0.26606550458429));
#39065=CARTESIAN_POINT('Ctrl Pts',(-0.146122305401386,-4.76483376818114E-5,
0.258934495415709));
#39066=CARTESIAN_POINT('Ctrl Pts',(-0.146184947882857,-0.0215701994360498,
0.260100542209937));
#39067=CARTESIAN_POINT('Ctrl Pts',(-0.141739031650533,-0.0430681260504587,
0.261266589004165));
#39068=CARTESIAN_POINT('Ctrl Pts',(-0.132654825339554,-0.0623847627977247,
0.262432635798393));
#39069=CARTESIAN_POINT('Ctrl Pts',(-0.112003227585469,-0.106298275812525,
0.265083470503427));
#39070=CARTESIAN_POINT('Ctrl Pts',(-0.0673803488302883,-0.138938601626132,
0.267734305208461));
#39071=CARTESIAN_POINT('Ctrl Pts',(-0.019274489346019,-0.145319150065199,
0.270385139913496));
#39072=CARTESIAN_POINT('Ctrl Pts',(0.02883137013825,-0.151699698504265,
0.27303597461853));
#39073=CARTESIAN_POINT('Ctrl Pts',(0.0804202103516079,-0.131820469568792,
0.275686809323564));
#39074=CARTESIAN_POINT('Ctrl Pts',(0.11180535579315,-0.0948088800228575,
0.278337644028599));
#39075=CARTESIAN_POINT('Ctrl Pts',(0.143190501234693,-0.0577972904769225,
0.280988478733633));
#39076=CARTESIAN_POINT('Ctrl Pts',(0.154371951904419,-0.00365334032052542,
0.283639313438667));
#39077=CARTESIAN_POINT('Ctrl Pts',(0.14021581852446,0.0427631330787578,
0.286290148143701));
#39078=CARTESIAN_POINT('Ctrl Pts',(0.126059685144501,0.0891796064780407,
0.288940982848735));
#39079=CARTESIAN_POINT('Ctrl Pts',(0.0865659677148572,0.12786860312021,
0.29159181755377));
#39080=CARTESIAN_POINT('Ctrl Pts',(0.0398679459367864,0.141066325542232,
0.294242652258804));
#39081=CARTESIAN_POINT('Ctrl Pts',(-0.00683007584128473,0.154264047964254,
0.296893486963838));
#39082=CARTESIAN_POINT('Ctrl Pts',(-0.0607324019677826,0.141970496166129,
0.299544321668873));
#39083=CARTESIAN_POINT('Ctrl Pts',(-0.0970901351530201,0.109830173318867,
0.302195156373907));
#39084=CARTESIAN_POINT('Ctrl Pts',(-0.127901447813816,0.0825928994431667,
0.304441602721174));
#39085=CARTESIAN_POINT('Ctrl Pts',(-0.14611277332701,0.0411022848956265,
0.306688049068442));
#39086=CARTESIAN_POINT('Ctrl Pts',(-0.146466968003471,-0.000114397412080779,
0.308934495415709));
#39087=CARTESIAN_POINT('Origin',(0.,0.,0.));
#39088=CARTESIAN_POINT('',(-0.146456696168336,0.00011684297731019,0.36606550458429));
#39089=CARTESIAN_POINT('',(-0.146490622007778,0.000105425447882283,0.358934495415709));
#39090=CARTESIAN_POINT('',(-0.14635,-1.79227059055215E-17,0.));
#39091=CARTESIAN_POINT('Ctrl Pts',(-0.146456696168336,0.00011684297731019,
0.36606550458429));
#39092=CARTESIAN_POINT('Ctrl Pts',(-0.146524266643172,0.00787170677865199,
0.365642915871516));
#39093=CARTESIAN_POINT('Ctrl Pts',(-0.145961554618594,0.0156167466990778,
0.365220327158741));
#39094=CARTESIAN_POINT('Ctrl Pts',(-0.14473428578122,0.0232550097723626,
0.364797738445966));
#39095=CARTESIAN_POINT('Ctrl Pts',(-0.137044379852877,0.0711153666076302,
0.362149852873827));
#39096=CARTESIAN_POINT('Ctrl Pts',(-0.103263231798211,0.11478354525948,
0.359501967301688));
#39097=CARTESIAN_POINT('Ctrl Pts',(-0.0588696551343872,0.134250410014218,
0.356854081729549));
#39098=CARTESIAN_POINT('Ctrl Pts',(-0.0144760784705634,0.153717274768956,
0.354206196157409));
#39099=CARTESIAN_POINT('Ctrl Pts',(0.040529926802418,0.148982825626583,
0.35155831058527));
#39100=CARTESIAN_POINT('Ctrl Pts',(0.0809441375650951,0.122216428534895,
0.34891042501313));
#39101=CARTESIAN_POINT('Ctrl Pts',(0.121358348327771,0.0954500314432082,
0.346262539440991));
#39102=CARTESIAN_POINT('Ctrl Pts',(0.147180764580144,0.0466516864022081,
0.343614653868852));
#39103=CARTESIAN_POINT('Ctrl Pts',(0.146579333092572,-0.00181878629327471,
0.340966768296713));
#39104=CARTESIAN_POINT('Ctrl Pts',(0.145977901604999,-0.0502892589887582,
0.338318882724573));
#39105=CARTESIAN_POINT('Ctrl Pts',(0.11895262237748,-0.0984318593387246,
0.335670997152434));
#39106=CARTESIAN_POINT('Ctrl Pts',(0.0778867105927371,-0.124187234331756,
0.333023111580295));
#39107=CARTESIAN_POINT('Ctrl Pts',(0.036820798807994,-0.149942609324788,
0.330375226008155));
#39108=CARTESIAN_POINT('Ctrl Pts',(-0.0182857455339734,-0.153310758960884,
0.327727340436016));
#39109=CARTESIAN_POINT('Ctrl Pts',(-0.062182630799685,-0.132748368261283,
0.325079454863877));
#39110=CARTESIAN_POINT('Ctrl Pts',(-0.106079516065397,-0.112185977561681,
0.322431569291738));
#39111=CARTESIAN_POINT('Ctrl Pts',(-0.138766742254852,-0.0676930465263806,
0.319783683719598));
#39112=CARTESIAN_POINT('Ctrl Pts',(-0.145266741627948,-0.0196566181036479,
0.317135798147459));
#39113=CARTESIAN_POINT('Ctrl Pts',(-0.146142523114734,-0.0131843998326608,
0.316779033626403));
#39114=CARTESIAN_POINT('Ctrl Pts',(-0.14654290982994,-0.00664785401210523,
0.316422269105347));
#39115=CARTESIAN_POINT('Ctrl Pts',(-0.146489966325848,-0.000104789085069334,
0.31606550458429));
#39116=CARTESIAN_POINT('Ctrl Pts',(-0.146466968003471,-0.000114397412080779,
0.308934495415709));
#39117=CARTESIAN_POINT('Ctrl Pts',(-0.146530727462368,-0.00753391423752658,
0.309338883773476));
#39118=CARTESIAN_POINT('Ctrl Pts',(-0.146015835709215,-0.0149445544285316,
0.309743272131243));
#39119=CARTESIAN_POINT('Ctrl Pts',(-0.144891626709003,-0.0222615773186769,
0.31014766048901));
#39120=CARTESIAN_POINT('Ctrl Pts',(-0.137522244835771,-0.0702259112125575,
0.312798495194044));
#39121=CARTESIAN_POINT('Ctrl Pts',(-0.103970340845329,-0.114167485103918,
0.315449329899078));
#39122=CARTESIAN_POINT('Ctrl Pts',(-0.0596410500115333,-0.133910815353779,
0.318100164604112));
#39123=CARTESIAN_POINT('Ctrl Pts',(-0.015311759177738,-0.15365414560364,
0.320750999309147));
#39124=CARTESIAN_POINT('Ctrl Pts',(0.0397949184994109,-0.149199232212,0.323401834014181));
#39125=CARTESIAN_POINT('Ctrl Pts',(0.0803771156598139,-0.122591519257586,
0.326052668719215));
#39126=CARTESIAN_POINT('Ctrl Pts',(0.120959312820217,-0.0959838063031723,
0.32870350342425));
#39127=CARTESIAN_POINT('Ctrl Pts',(0.147017029463874,-0.0472232937859833,
0.331354338129284));
#39128=CARTESIAN_POINT('Ctrl Pts',(0.146586036983397,0.00130195078264539,
0.334005172834318));
#39129=CARTESIAN_POINT('Ctrl Pts',(0.146155044502921,0.0498271953512744,
0.336656007539352));
#39130=CARTESIAN_POINT('Ctrl Pts',(0.119235342898311,0.0981171719713431,
0.339306842244386));
#39131=CARTESIAN_POINT('Ctrl Pts',(0.0781869354735432,0.123999856599104,
0.341957676949421));
#39132=CARTESIAN_POINT('Ctrl Pts',(0.0371385280487761,0.149882541226865,
0.344608511654455));
#39133=CARTESIAN_POINT('Ctrl Pts',(-0.0180385851961482,0.153357933862318,
0.347259346359489));
#39134=CARTESIAN_POINT('Ctrl Pts',(-0.0620101968435835,0.132830330894432,
0.349910181064524));
#39135=CARTESIAN_POINT('Ctrl Pts',(-0.105981808491019,0.112302727926544,
0.352561015769558));
#39136=CARTESIAN_POINT('Ctrl Pts',(-0.138747918540966,0.0677721293553162,
0.355211850474592));
#39137=CARTESIAN_POINT('Ctrl Pts',(-0.145264183888347,0.0196844656531965,
0.357862685179626));
#39138=CARTESIAN_POINT('Ctrl Pts',(-0.146142422968675,0.0132033812753397,
0.358219955258321));
#39139=CARTESIAN_POINT('Ctrl Pts',(-0.146543841751789,0.00665768391130569,
0.358577225337015));
#39140=CARTESIAN_POINT('Ctrl Pts',(-0.146490622007778,0.000105425447882283,
0.358934495415709));
#39141=CARTESIAN_POINT('Origin',(0.,0.,0.));
#39142=CARTESIAN_POINT('',(-0.146117527463381,3.66422859593568E-5,0.416065504584291));
#39143=CARTESIAN_POINT('',(-0.146131941026353,6.08514395597815E-5,0.408934495415709));
#39144=CARTESIAN_POINT('',(-0.14635,-1.79227059055215E-17,0.));
#39145=CARTESIAN_POINT('Ctrl Pts',(-0.146117527463381,3.66422859593568E-5,
0.416065504584291));
#39146=CARTESIAN_POINT('Ctrl Pts',(-0.146167164015074,0.0222235765819606,
0.414863562637685));
#39147=CARTESIAN_POINT('Ctrl Pts',(-0.141430069804178,0.0443904018142415,
0.413661620691079));
#39148=CARTESIAN_POINT('Ctrl Pts',(-0.131797444393702,0.0641735569006793,
0.412459678744474));
#39149=CARTESIAN_POINT('Ctrl Pts',(-0.11057671079816,0.107755970404684,
0.409811793172335));
#39150=CARTESIAN_POINT('Ctrl Pts',(-0.0655968071821861,0.139769869286095,
0.407163907600195));
#39151=CARTESIAN_POINT('Ctrl Pts',(-0.0174679796227892,0.145546147336919,
0.404516022028056));
#39152=CARTESIAN_POINT('Ctrl Pts',(0.0306608479366084,0.151322425387742,
0.401868136455917));
#39153=CARTESIAN_POINT('Ctrl Pts',(0.0819385994394289,0.130861082607978,
0.399220250883777));
#39154=CARTESIAN_POINT('Ctrl Pts',(0.112869404704651,0.0935377150207321,
0.396572365311638));
#39155=CARTESIAN_POINT('Ctrl Pts',(0.143800209969873,0.0562143474334866,
0.393924479739499));
#39156=CARTESIAN_POINT('Ctrl Pts',(0.154384068997497,0.00202895503876042,
0.391276594167359));
#39157=CARTESIAN_POINT('Ctrl Pts',(0.139771347867625,-0.0441902675604103,
0.38862870859522));
#39158=CARTESIAN_POINT('Ctrl Pts',(0.125158626737753,-0.0904094901595803,
0.385980823023081));
#39159=CARTESIAN_POINT('Ctrl Pts',(0.0853493254503865,-0.128662542963195,
0.383332937450942));
#39160=CARTESIAN_POINT('Ctrl Pts',(0.0385844175605987,-0.141421539587247,
0.380685051878802));
#39161=CARTESIAN_POINT('Ctrl Pts',(-0.00818049032918902,-0.154180536211298,
0.378037166306663));
#39162=CARTESIAN_POINT('Ctrl Pts',(-0.0619010048213979,-0.141445476655787,
0.375389280734523));
#39163=CARTESIAN_POINT('Ctrl Pts',(-0.0979619301664915,-0.109051679368689,
0.372741395162384));
#39164=CARTESIAN_POINT('Ctrl Pts',(-0.128267720099621,-0.081827763001475,
0.370516098303019));
#39165=CARTESIAN_POINT('Ctrl Pts',(-0.146100878890467,-0.0407192549596569,
0.368290801443655));
#39166=CARTESIAN_POINT('Ctrl Pts',(-0.146456696168336,0.00011684297731019,
0.36606550458429));
#39167=CARTESIAN_POINT('Ctrl Pts',(-0.146490622007778,0.000105425447882283,
0.358934495415709));
#39168=CARTESIAN_POINT('Ctrl Pts',(-0.146148967529651,-0.0419580697355662,
0.361228060042049));
#39169=CARTESIAN_POINT('Ctrl Pts',(-0.12707053516474,-0.0842919640484707,
0.363521624668389));
#39170=CARTESIAN_POINT('Ctrl Pts',(-0.0951239884102214,-0.111537384525928,
0.365815189294729));
#39171=CARTESIAN_POINT('Ctrl Pts',(-0.0582011069398996,-0.143026842169921,
0.368466023999764));
#39172=CARTESIAN_POINT('Ctrl Pts',(-0.00408892335444046,-0.154361028624896,
0.371116858704798));
#39173=CARTESIAN_POINT('Ctrl Pts',(0.0423673101370894,-0.140335926848737,
0.373767693409832));
#39174=CARTESIAN_POINT('Ctrl Pts',(0.0888235436286192,-0.126310825072579,
0.376418528114866));
#39175=CARTESIAN_POINT('Ctrl Pts',(0.12762382702622,-0.0869264350652862,
0.379069362819901));
#39176=CARTESIAN_POINT('Ctrl Pts',(0.140953266768128,-0.0402658398230972,
0.381720197524935));
#39177=CARTESIAN_POINT('Ctrl Pts',(0.154282706510036,0.00639475541909176,
0.384371032229969));
#39178=CARTESIAN_POINT('Ctrl Pts',(0.142141302596253,0.0603315558961778,
0.387021866935004));
#39179=CARTESIAN_POINT('Ctrl Pts',(0.110103699587577,0.0967798361409283,
0.389672701640038));
#39180=CARTESIAN_POINT('Ctrl Pts',(0.0780660965789003,0.133228116385679,
0.392323536345072));
#39181=CARTESIAN_POINT('Ctrl Pts',(0.0261322944753315,0.152187876398094,
0.394974371050106));
#39182=CARTESIAN_POINT('Ctrl Pts',(-0.0218526425106493,0.144953866566232,
0.397625205755141));
#39183=CARTESIAN_POINT('Ctrl Pts',(-0.0698375794966294,0.13771985673437,
0.400276040460175));
#39184=CARTESIAN_POINT('Ctrl Pts',(-0.113873651365021,0.104292077058233,
0.402926875165209));
#39185=CARTESIAN_POINT('Ctrl Pts',(-0.133741989653421,0.0600186737328441,
0.405577709870243));
#39186=CARTESIAN_POINT('Ctrl Pts',(-0.142128499086628,0.0413306833614836,
0.406696638385399));
#39187=CARTESIAN_POINT('Ctrl Pts',(-0.14620899575881,0.0207103068323409,
0.407815566900554));
#39188=CARTESIAN_POINT('Ctrl Pts',(-0.146131941026353,6.08514395597814E-5,
0.408934495415709));
#39189=CARTESIAN_POINT('Origin',(0.,0.,0.));
#39190=CARTESIAN_POINT('',(-0.146320034481408,-0.000132042578932776,0.466065504584291));
#39191=CARTESIAN_POINT('',(-0.146267142220666,-0.000128791573925899,0.458934495415709));
#39192=CARTESIAN_POINT('',(-0.14635,-1.79227059055215E-17,0.));
#39193=CARTESIAN_POINT('Ctrl Pts',(-0.146320034481408,-0.000132042578932776,
0.466065504584291));
#39194=CARTESIAN_POINT('Ctrl Pts',(-0.145990955376697,0.0363120653110472,
0.464084209403854));
#39195=CARTESIAN_POINT('Ctrl Pts',(-0.132207444595406,0.0729769481781354,
0.462102914223418));
#39196=CARTESIAN_POINT('Ctrl Pts',(-0.107565849799547,0.0995912952759384,
0.460121619042982));
#39197=CARTESIAN_POINT('Ctrl Pts',(-0.074633794052009,0.135159819536245,
0.457473733470842));
#39198=CARTESIAN_POINT('Ctrl Pts',(-0.0223083694375825,0.15277731788608,
0.454825847898703));
#39199=CARTESIAN_POINT('Ctrl Pts',(0.0254312589463019,0.144368338990174,
0.452177962326564));
#39200=CARTESIAN_POINT('Ctrl Pts',(0.0731708873301868,0.135959360094269,
0.449530076754424));
#39201=CARTESIAN_POINT('Ctrl Pts',(0.116324719483529,0.101523903952622,
0.446882191182285));
#39202=CARTESIAN_POINT('Ctrl Pts',(0.13512098610947,0.0568421509649556,
0.444234305610146));
#39203=CARTESIAN_POINT('Ctrl Pts',(0.153917252735412,0.0121603979772891,
0.441586420038006));
#39204=CARTESIAN_POINT('Ctrl Pts',(0.148355953833953,-0.0427676518563976,
0.438938534465867));
#39205=CARTESIAN_POINT('Ctrl Pts',(0.120984436568095,-0.0827743147100686,
0.436290648893728));
#39206=CARTESIAN_POINT('Ctrl Pts',(0.0936129193022383,-0.122780977563739,
0.433642763321588));
#39207=CARTESIAN_POINT('Ctrl Pts',(0.044431183671984,-0.147866253437395,
0.430994877749449));
#39208=CARTESIAN_POINT('Ctrl Pts',(-0.0040248096733416,-0.146535421965135,
0.42834699217731));
#39209=CARTESIAN_POINT('Ctrl Pts',(-0.0524808030186669,-0.145204590492875,
0.425699106605171));
#39210=CARTESIAN_POINT('Ctrl Pts',(-0.100211054079063,-0.117457651674699,
0.423051221033031));
#39211=CARTESIAN_POINT('Ctrl Pts',(-0.125345397821707,-0.0760087182023128,
0.420403335460892));
#39212=CARTESIAN_POINT('Ctrl Pts',(-0.139070629946179,-0.0533744994995956,
0.418957391835358));
#39213=CARTESIAN_POINT('Ctrl Pts',(-0.146057814383464,-0.0266543774475973,
0.417511448209824));
#39214=CARTESIAN_POINT('Ctrl Pts',(-0.146117527463381,3.66422859593568E-5,
0.416065504584291));
#39215=CARTESIAN_POINT('Ctrl Pts',(-0.146131941026353,6.08514395597814E-5,
0.408934495415709));
#39216=CARTESIAN_POINT('Ctrl Pts',(-0.146026446689573,-0.0282099702486701,
0.410466401605588));
#39217=CARTESIAN_POINT('Ctrl Pts',(-0.138128084958642,-0.0565352970304639,
0.411998307795467));
#39218=CARTESIAN_POINT('Ctrl Pts',(-0.122817836477901,-0.0800308731172956,
0.413530213985346));
#39219=CARTESIAN_POINT('Ctrl Pts',(-0.0963247403055724,-0.120687989667408,
0.41618104869038));
#39220=CARTESIAN_POINT('Ctrl Pts',(-0.0476379432525075,-0.146883195792991,
0.418831883395415));
#39221=CARTESIAN_POINT('Ctrl Pts',(0.000888321221429993,-0.146589129065305,
0.421482718100449));
#39222=CARTESIAN_POINT('Ctrl Pts',(0.0494145856953668,-0.146295062337618,
0.424133552805483));
#39223=CARTESIAN_POINT('Ctrl Pts',(0.097780317590176,-0.119511722756663,
0.426784387510517));
#39224=CARTESIAN_POINT('Ctrl Pts',(0.123778732978107,-0.0785365161302261,
0.429435222215552));
#39225=CARTESIAN_POINT('Ctrl Pts',(0.149777148366038,-0.0375613095037888,
0.432086056920586));
#39226=CARTESIAN_POINT('Ctrl Pts',(0.15340824724709,0.0176057641681304,
0.43473689162562));
#39227=CARTESIAN_POINT('Ctrl Pts',(0.13300479146532,0.0616351303104708,
0.437387726330655));
#39228=CARTESIAN_POINT('Ctrl Pts',(0.112601335683551,0.105664496452811,
0.440038561035689));
#39229=CARTESIAN_POINT('Ctrl Pts',(0.0681633252389606,0.138556155065572,
0.442689395740723));
#39230=CARTESIAN_POINT('Ctrl Pts',(0.0200942611983476,0.145208074081285,
0.445340230445757));
#39231=CARTESIAN_POINT('Ctrl Pts',(-0.0279748028422658,0.151859993096997,
0.447991065150791));
#39232=CARTESIAN_POINT('Ctrl Pts',(-0.0796749204789013,0.132272172515661,
0.450641899855826));
#39233=CARTESIAN_POINT('Ctrl Pts',(-0.111268479500082,0.095438314693151,
0.45329273456086));
#39234=CARTESIAN_POINT('Ctrl Pts',(-0.133681961086661,0.0693071974766942,
0.455173321512477));
#39235=CARTESIAN_POINT('Ctrl Pts',(-0.145975937294016,0.0344962574238126,
0.457053908464093));
#39236=CARTESIAN_POINT('Ctrl Pts',(-0.146267142220666,-0.000128791573925899,
0.458934495415709));
#39237=CARTESIAN_POINT('Origin',(0.,0.,-0.0924367114736154));
#39238=CARTESIAN_POINT('',(-0.117750885282186,-0.00010626111879085,0.482563288526385));
#39239=CARTESIAN_POINT('',(-0.117972864089022,-5.93608753193428E-7,0.492436711473616));
#39240=CARTESIAN_POINT('',(-0.117775,-8.88924268665971E-15,-0.0924367114736154));
#39241=CARTESIAN_POINT('',(-0.117668597464311,0.00500517689817391,0.532225000000001));
#39242=CARTESIAN_POINT('Ctrl Pts',(-0.117750885282186,-0.000106261118790843,
0.482563288526385));
#39243=CARTESIAN_POINT('Ctrl Pts',(-0.117839983816431,-0.00997354393438475,
0.483229878918088));
#39244=CARTESIAN_POINT('Ctrl Pts',(-0.112189023051801,-0.0589364681957879,
0.486544354881929));
#39245=CARTESIAN_POINT('Ctrl Pts',(-0.0439766578214066,-0.132120623957634,
0.492506716417911));
#39246=CARTESIAN_POINT('Ctrl Pts',(0.087240331747497,-0.108512430051717,
0.500450373134329));
#39247=CARTESIAN_POINT('Ctrl Pts',(0.138438921804208,0.0144739368962113,
0.508394029850746));
#39248=CARTESIAN_POINT('Ctrl Pts',(0.0629040591690992,0.12431971381125,
0.516337686567165));
#39249=CARTESIAN_POINT('Ctrl Pts',(-0.0705459363093062,0.119993110375402,
0.524281343283582));
#39250=CARTESIAN_POINT('Ctrl Pts',(-0.116003159314893,0.0441585924901374,
0.529577114427861));
#39251=CARTESIAN_POINT('Ctrl Pts',(-0.117668597464311,0.00500517689817385,
0.532225));
#39252=CARTESIAN_POINT('',(-0.0334019664626897,0.112939183906319,0.532225000000001));
#39253=CARTESIAN_POINT('Origin',(0.,0.,0.532225));
#39254=CARTESIAN_POINT('Ctrl Pts',(-0.117972864533492,-5.93610086620396E-7,
0.492436711473617));
#39255=CARTESIAN_POINT('Ctrl Pts',(-0.117972892941239,-0.000127136793190444,
0.492445300790573));
#39256=CARTESIAN_POINT('Ctrl Pts',(-0.117912463615216,-0.0393074137896712,
0.495104724812564));
#39257=CARTESIAN_POINT('Ctrl Pts',(-0.0749307309976486,-0.117412744486246,
0.500414983539588));
#39258=CARTESIAN_POINT('Ctrl Pts',(0.0581614397283287,-0.126517333775439,
0.508367487654693));
#39259=CARTESIAN_POINT('Ctrl Pts',(0.138005962114904,-0.01953005209576,
0.516319991769794));
#39260=CARTESIAN_POINT('Ctrl Pts',(0.0908022345067483,0.105567300931769,
0.524272495884898));
#39261=CARTESIAN_POINT('Ctrl Pts',(0.00421962447768953,0.124065836989857,
0.529574165294966));
#39262=CARTESIAN_POINT('Ctrl Pts',(-0.0334019664626881,0.11293918390632,
0.532225));
#39263=CARTESIAN_POINT('Origin',(0.,0.,-0.0924367114736154));
#39264=CARTESIAN_POINT('',(-0.117587917984282,2.94878389348885E-5,0.432563288526385));
#39265=CARTESIAN_POINT('',(-0.117708320294082,-0.000103644876124687,0.442436711473616));
#39266=CARTESIAN_POINT('',(-0.117775,-8.88924268665971E-15,-0.0924367114736154));
#39267=CARTESIAN_POINT('Ctrl Pts',(-0.117587917984282,2.94878389348868E-5,
0.432563288526385));
#39268=CARTESIAN_POINT('Ctrl Pts',(-0.117539863949521,-0.0214500806552194,
0.434009232151918));
#39269=CARTESIAN_POINT('Ctrl Pts',(-0.101619941365326,-0.082330436444606,
0.438103061349591));
#39270=CARTESIAN_POINT('Ctrl Pts',(-0.00382300141363195,-0.139182551176009,
0.444844776119403));
#39271=CARTESIAN_POINT('Ctrl Pts',(0.11491384000461,-0.0786205074584852,
0.452788432835821));
#39272=CARTESIAN_POINT('Ctrl Pts',(0.128340187352459,0.0539893538840985,
0.460732089552239));
#39273=CARTESIAN_POINT('Ctrl Pts',(0.024156191824071,0.137125039167645,
0.468675746268657));
#39274=CARTESIAN_POINT('Ctrl Pts',(-0.0915696283436722,0.0981611996792526,
0.475952812593373));
#39275=CARTESIAN_POINT('Ctrl Pts',(-0.117486059238065,0.0292220942398885,
0.480581993345948));
#39276=CARTESIAN_POINT('Ctrl Pts',(-0.117750885282186,-0.000106261118790843,
0.482563288526385));
#39277=CARTESIAN_POINT('Ctrl Pts',(-0.117708320294082,-0.000103644876124676,
0.442436711473616));
#39278=CARTESIAN_POINT('Ctrl Pts',(-0.117804303693274,-0.0115163291952777,
0.443206959227034));
#39279=CARTESIAN_POINT('Ctrl Pts',(-0.111033657777347,-0.0620947057757177,
0.446628041685486));
#39280=CARTESIAN_POINT('Ctrl Pts',(-0.038636663810782,-0.133821400192823,
0.452699958848972));
#39281=CARTESIAN_POINT('Ctrl Pts',(0.0916608011058181,-0.104875817685159,
0.460652462964076));
#39282=CARTESIAN_POINT('Ctrl Pts',(0.137790741908166,0.0203740232160909,
0.468604967079177));
#39283=CARTESIAN_POINT('Ctrl Pts',(0.0573828398023632,0.126918127906013,
0.476557471194281));
#39284=CARTESIAN_POINT('Ctrl Pts',(-0.0755630108222985,0.116919225220885,
0.484501385992427));
#39285=CARTESIAN_POINT('Ctrl Pts',(-0.117964125743295,0.0389266160426656,
0.489794466085539));
#39286=CARTESIAN_POINT('Ctrl Pts',(-0.117972864533492,-5.93610086620396E-7,
0.492436711473617));
#39287=CARTESIAN_POINT('Origin',(0.,0.,-0.0924367114736154));
#39288=CARTESIAN_POINT('',(-0.117860863622998,9.40292562467743E-5,0.382563288526384));
#39289=CARTESIAN_POINT('',(-0.11759951728308,4.89701284099239E-5,0.392436711473616));
#39290=CARTESIAN_POINT('',(-0.117775,-8.88924268665971E-15,-0.0924367114736154));
#39291=CARTESIAN_POINT('Ctrl Pts',(-0.117860863622998,9.40292562467788E-5,
0.382563288526384));
#39292=CARTESIAN_POINT('Ctrl Pts',(-0.117574520063714,-0.0327687752160871,
0.384788585385749));
#39293=CARTESIAN_POINT('Ctrl Pts',(-0.0861467637051906,-0.105215176336211,
0.389661767817253));
#39294=CARTESIAN_POINT('Ctrl Pts',(0.0366482838797405,-0.134325140358292,
0.397182835820896));
#39295=CARTESIAN_POINT('Ctrl Pts',(0.132757756905765,-0.0419728350502109,
0.405126492537314));
#39296=CARTESIAN_POINT('Ctrl Pts',(0.107205710503746,0.0888440680441954,
0.413070149253731));
#39297=CARTESIAN_POINT('Ctrl Pts',(-0.0165914302528927,0.138242796692368,
0.42101380597015));
#39298=CARTESIAN_POINT('Ctrl Pts',(-0.105417454577164,0.0750219551131263,
0.427511519061034));
#39299=CARTESIAN_POINT('Ctrl Pts',(-0.117627862944144,0.0178843985783384,
0.431361346579779));
#39300=CARTESIAN_POINT('Ctrl Pts',(-0.117587917984282,2.94878389348868E-5,
0.432563288526385));
#39301=CARTESIAN_POINT('Ctrl Pts',(-0.11759951728308,4.89701284099274E-5,
0.392436711473616));
#39302=CARTESIAN_POINT('Ctrl Pts',(-0.11751462083269,-0.0227019422346301,
0.393968617663495));
#39303=CARTESIAN_POINT('Ctrl Pts',(-0.100159557717256,-0.0849411572528722,
0.398151358558408));
#39304=CARTESIAN_POINT('Ctrl Pts',(0.000844063931402275,-0.139284651766041,
0.404984934158356));
#39305=CARTESIAN_POINT('Ctrl Pts',(0.117610871049501,-0.0746230633995127,
0.412937438273457));
#39306=CARTESIAN_POINT('Ctrl Pts',(0.126377239427685,0.0585638604483229,
0.420889942388562));
#39307=CARTESIAN_POINT('Ctrl Pts',(0.0190929207373193,0.137972437690235,
0.428842446503664));
#39308=CARTESIAN_POINT('Ctrl Pts',(-0.0936346562739906,0.0952629110198009,
0.436024702865349));
#39309=CARTESIAN_POINT('Ctrl Pts',(-0.117473973452704,0.0277608248588199,
0.440556124522));
#39310=CARTESIAN_POINT('Ctrl Pts',(-0.117708320294082,-0.000103644876124676,
0.442436711473616));
#39311=CARTESIAN_POINT('Origin',(0.,0.,-0.0924367114736154));
#39312=CARTESIAN_POINT('',(-0.117887637745315,-8.43288998643762E-5,0.332563288526385));
#39313=CARTESIAN_POINT('',(-0.11788816540462,8.48410121138156E-5,0.342436711473616));
#39314=CARTESIAN_POINT('',(-0.117775,-8.88924268665971E-15,-0.0924367114736154));
#39315=CARTESIAN_POINT('Ctrl Pts',(-0.117887637745315,-8.43288998643547E-5,
0.332563288526385));
#39316=CARTESIAN_POINT('Ctrl Pts',(-0.117930243971446,-0.00534985313478999,
0.332920053047441));
#39317=CARTESIAN_POINT('Ctrl Pts',(-0.115216603610867,-0.0496516091215746,
0.335924703140636));
#39318=CARTESIAN_POINT('Ctrl Pts',(-0.0590623637863932,-0.126087177724698,
0.34157723880597));
#39319=CARTESIAN_POINT('Ctrl Pts',(0.0739784273282333,-0.117955633685244,
0.349520895522388));
#39320=CARTESIAN_POINT('Ctrl Pts',(0.139224117680559,-0.00172752115601949,
0.357464552238807));
#39321=CARTESIAN_POINT('Ctrl Pts',(0.0768824352591712,0.11608372080921,
0.365408208955224));
#39322=CARTESIAN_POINT('Ctrl Pts',(-0.0559156297430559,0.12751384888047,
0.373351865671643));
#39323=CARTESIAN_POINT('Ctrl Pts',(-0.114624951070718,0.0516215456314347,
0.379070225528695));
#39324=CARTESIAN_POINT('Ctrl Pts',(-0.117915240887596,0.00633474728975054,
0.382140699813609));
#39325=CARTESIAN_POINT('Ctrl Pts',(-0.117860863622998,9.40292562467788E-5,
0.382563288526384));
#39326=CARTESIAN_POINT('Ctrl Pts',(-0.11788816540462,8.4841012113826E-5,
0.342436711473616));
#39327=CARTESIAN_POINT('Ctrl Pts',(-0.1176132193427,-0.0337657100314819,
0.344730276099956));
#39328=CARTESIAN_POINT('Ctrl Pts',(-0.0845149237619996,-0.107208837865588,
0.34967467543133));
#39329=CARTESIAN_POINT('Ctrl Pts',(0.0402561631274929,-0.133343040355529,
0.357269909467738));
#39330=CARTESIAN_POINT('Ctrl Pts',(0.133929618074243,-0.0382594079720193,
0.365222413582842));
#39331=CARTESIAN_POINT('Ctrl Pts',(0.104617274119081,0.0919573329132998,
0.373174917697944));
#39332=CARTESIAN_POINT('Ctrl Pts',(-0.020763734615072,0.137730870367254,
0.381127421813047));
#39333=CARTESIAN_POINT('Ctrl Pts',(-0.106598215372521,0.0725739208566139,
0.387548019738271));
#39334=CARTESIAN_POINT('Ctrl Pts',(-0.117661526993468,0.0166665964275914,
0.391317782958461));
#39335=CARTESIAN_POINT('Ctrl Pts',(-0.11759951728308,4.89701284099274E-5,
0.392436711473616));
#39336=CARTESIAN_POINT('Origin',(0.,0.,-0.0924367114736154));
#39337=CARTESIAN_POINT('',(-0.117597135791184,-4.46042773137295E-5,0.282563288526384));
#39338=CARTESIAN_POINT('',(-0.117869129870917,-9.20611903598989E-5,0.292436711473616));
#39339=CARTESIAN_POINT('',(-0.117775,-8.88924268665971E-15,-0.0924367114736154));
#39340=CARTESIAN_POINT('Ctrl Pts',(-0.117597135791184,-4.46042773137294E-5,
0.282563288526384));
#39341=CARTESIAN_POINT('Ctrl Pts',(-0.117654518243026,-0.0169184081852861,
0.283699406281271));
#39342=CARTESIAN_POINT('Ctrl Pts',(-0.106362773508523,-0.0730457989372372,
0.287483409608297));
#39343=CARTESIAN_POINT('Ctrl Pts',(-0.0200165152988323,-0.137788527592198,
0.293915298507463));
#39344=CARTESIAN_POINT('Ctrl Pts',(0.104968269293632,-0.0914767820950745,
0.301858955223881));
#39345=CARTESIAN_POINT('Ctrl Pts',(0.133758329466478,0.0386658573002006,
0.309802611940298));
#39346=CARTESIAN_POINT('Ctrl Pts',(0.0399699596916912,0.133374441107753,
0.317746268656717));
#39347=CARTESIAN_POINT('Ctrl Pts',(-0.084590271720082,0.107092283864913,
0.325333160852078));
#39348=CARTESIAN_POINT('Ctrl Pts',(-0.117614023033548,0.0337305621770822,
0.330272167475301));
#39349=CARTESIAN_POINT('Ctrl Pts',(-0.117887637745315,-8.43288998643547E-5,
0.332563288526385));
#39350=CARTESIAN_POINT('Ctrl Pts',(-0.117869129870917,-9.2061190359885E-5,
0.292436711473616));
#39351=CARTESIAN_POINT('Ctrl Pts',(-0.117920440224669,-0.00606290911736031,
0.292841099831383));
#39352=CARTESIAN_POINT('Ctrl Pts',(-0.114789890532149,-0.0511197142210238,
0.295896322894184));
#39353=CARTESIAN_POINT('Ctrl Pts',(-0.0566691588697243,-0.127238089669758,
0.301602380662019));
#39354=CARTESIAN_POINT('Ctrl Pts',(0.0763719541489209,-0.116482829853556,
0.309554884777122));
#39355=CARTESIAN_POINT('Ctrl Pts',(0.139281709756163,0.00123707506708643,
0.317507388892225));
#39356=CARTESIAN_POINT('Ctrl Pts',(0.0742909098282569,0.117820990265484,
0.325459893007327));
#39357=CARTESIAN_POINT('Ctrl Pts',(-0.0589202520252667,0.1262114453589,
0.33341239712243));
#39358=CARTESIAN_POINT('Ctrl Pts',(-0.115211084829427,0.0497097039247984,
0.339071336611193));
#39359=CARTESIAN_POINT('Ctrl Pts',(-0.11793099393452,0.00535776373524371,
0.342079441394922));
#39360=CARTESIAN_POINT('Ctrl Pts',(-0.11788816540462,8.4841012113826E-5,
0.342436711473616));
#39361=CARTESIAN_POINT('Origin',(0.,0.,-0.0924367114736154));
#39362=CARTESIAN_POINT('',(-0.117724026649356,0.00010549178999148,0.232563288526384));
#39363=CARTESIAN_POINT('',(-0.117591763024586,-3.83449468523145E-5,0.242436711473616));
#39364=CARTESIAN_POINT('',(-0.117775,-8.88924268665971E-15,-0.0924367114736154));
#39365=CARTESIAN_POINT('Ctrl Pts',(-0.117724026649356,0.000105491789991495,
0.232563288526384));
#39366=CARTESIAN_POINT('Ctrl Pts',(-0.117478226080151,-0.0282662610808501,
0.234478759515102));
#39367=CARTESIAN_POINT('Ctrl Pts',(-0.0929369215417509,-0.0962395631396471,
0.239042116075959));
#39368=CARTESIAN_POINT('Ctrl Pts',(0.0207448421498254,-0.137680756627218,
0.246253358208955));
#39369=CARTESIAN_POINT('Ctrl Pts',(0.126961839902422,-0.0571579428392388,
0.254197014925373));
#39370=CARTESIAN_POINT('Ctrl Pts',(0.116828827462796,0.075745391244066,
0.262140671641791));
#39371=CARTESIAN_POINT('Ctrl Pts',(-0.000368128572008151,0.139234348141551,
0.270084328358209));
#39372=CARTESIAN_POINT('Ctrl Pts',(-0.100514230788311,0.0842953826634335,
0.27689186731974));
#39373=CARTESIAN_POINT('Ctrl Pts',(-0.117520780198996,0.0224084148687892,
0.281051520709132));
#39374=CARTESIAN_POINT('Ctrl Pts',(-0.117597135791184,-4.46042773137294E-5,
0.282563288526384));
#39375=CARTESIAN_POINT('Ctrl Pts',(-0.117591763024586,-3.83449468523075E-5,
0.242436711473616));
#39376=CARTESIAN_POINT('Ctrl Pts',(-0.117642174491994,-0.017358594045656,
0.243602758267844));
#39377=CARTESIAN_POINT('Ctrl Pts',(-0.10593062496396,-0.0739889980249599,
0.247419639767106));
#39378=CARTESIAN_POINT('Ctrl Pts',(-0.0183140487741412,-0.138077951344142,
0.253887355971402));
#39379=CARTESIAN_POINT('Ctrl Pts',(0.106234136865658,-0.0900845891054932,
0.261839860086505));
#39380=CARTESIAN_POINT('Ctrl Pts',(0.133228916899009,0.040632262203075,
0.269792364201608));
#39381=CARTESIAN_POINT('Ctrl Pts',(0.0378813411502606,0.134037043471229,
0.27774486831671));
#39382=CARTESIAN_POINT('Ctrl Pts',(-0.085634823441202,0.105866601183683,
0.285292984074047));
#39383=CARTESIAN_POINT('Ctrl Pts',(-0.117584092098319,0.0330770181317487,
0.290190265126349));
#39384=CARTESIAN_POINT('Ctrl Pts',(-0.117869129870917,-9.2061190359885E-5,
0.292436711473616));
#39385=CARTESIAN_POINT('Origin',(0.,0.,-0.0924367114736154));
#39386=CARTESIAN_POINT('',(-0.117966882359366,-1.29211934964908E-5,0.182563288526384));
#39387=CARTESIAN_POINT('',(-0.117728105208174,0.000106637828744482,0.192436711473616));
#39388=CARTESIAN_POINT('',(-0.117775,-8.88924268665971E-15,-0.0924367114736154));
#39389=CARTESIAN_POINT('Ctrl Pts',(-0.117966882359366,-1.29211934964912E-5,
0.182563288526384));
#39390=CARTESIAN_POINT('Ctrl Pts',(-0.117967957119725,-0.000704465266726215,
0.182610227176794));
#39391=CARTESIAN_POINT('Ctrl Pts',(-0.117649070375187,-0.0404061166150831,
0.185305051399342));
#39392=CARTESIAN_POINT('Ctrl Pts',(-0.0733536600413758,-0.118345172107485,
0.19064776119403));
#39393=CARTESIAN_POINT('Ctrl Pts',(0.0597282696676458,-0.12577310138558,
0.198591417910448));
#39394=CARTESIAN_POINT('Ctrl Pts',(0.138074187460599,-0.0179404007303906,
0.206535074626866));
#39395=CARTESIAN_POINT('Ctrl Pts',(0.0898865489335327,0.106333191146418,
0.214478731343283));
#39396=CARTESIAN_POINT('Ctrl Pts',(-0.0406746665030564,0.133161220808791,
0.222422388059702));
#39397=CARTESIAN_POINT('Ctrl Pts',(-0.111466604862902,0.0609145729578186,
0.228450573787402));
#39398=CARTESIAN_POINT('Ctrl Pts',(-0.117818012892196,0.0109539388206346,
0.231830873942963));
#39399=CARTESIAN_POINT('Ctrl Pts',(-0.117724026649356,0.000105491789991495,
0.232563288526384));
#39400=CARTESIAN_POINT('Ctrl Pts',(-0.117728105208174,0.000106637828744488,
0.192436711473616));
#39401=CARTESIAN_POINT('Ctrl Pts',(-0.11747787316262,-0.0284437724366353,
0.194364416704305));
#39402=CARTESIAN_POINT('Ctrl Pts',(-0.0926723165398222,-0.0966441001570621,
0.198942956640028));
#39403=CARTESIAN_POINT('Ctrl Pts',(0.0215406810767683,-0.137611496939632,
0.206172331280785));
#39404=CARTESIAN_POINT('Ctrl Pts',(0.127397488829925,-0.056309900280862,
0.214124835395888));
#39405=CARTESIAN_POINT('Ctrl Pts',(0.116266864218555,0.0767003345124148,
0.222077339510991));
#39406=CARTESIAN_POINT('Ctrl Pts',(-0.0016300870944122,0.139277664563073,
0.230029843626094));
#39407=CARTESIAN_POINT('Ctrl Pts',(-0.100962832358778,0.0835357163242542,
0.236816300946969));
#39408=CARTESIAN_POINT('Ctrl Pts',(-0.117527571486354,0.0220164272984534,
0.240951923562809));
#39409=CARTESIAN_POINT('Ctrl Pts',(-0.117591763024586,-3.83449468523075E-5,
0.242436711473616));
#39410=CARTESIAN_POINT('Origin',(0.,0.,-0.0924367114736154));
#39411=CARTESIAN_POINT('',(-0.117685857408994,-9.79219620674319E-5,0.132563288526384));
#39412=CARTESIAN_POINT('',(-0.117968412270431,-1.06668654225733E-5,0.142436711473616));
#39413=CARTESIAN_POINT('',(-0.117775,-8.88924268665971E-15,-0.0924367114736154));
#39414=CARTESIAN_POINT('Ctrl Pts',(-0.117685857408994,-9.79219620674231E-5,
0.132563288526384));
#39415=CARTESIAN_POINT('Ctrl Pts',(-0.117781952389543,-0.0123469217649596,
0.133389580410625));
#39416=CARTESIAN_POINT('Ctrl Pts',(-0.110383000729775,-0.063735125339128,
0.136863757867004));
#39417=CARTESIAN_POINT('Ctrl Pts',(-0.03593748288359,-0.134517045800752,
0.142985820895522));
#39418=CARTESIAN_POINT('Ctrl Pts',(0.0935927050428541,-0.103086105216301,
0.150929477611941));
#39419=CARTESIAN_POINT('Ctrl Pts',(0.137352931996012,0.0228147184504364,
0.158873134328358));
#39420=CARTESIAN_POINT('Ctrl Pts',(0.0552405729858772,0.127807739141585,
0.166816791044776));
#39421=CARTESIAN_POINT('Ctrl Pts',(-0.0767108666901454,0.115747243191764,
0.174713509110785));
#39422=CARTESIAN_POINT('Ctrl Pts',(-0.117907328140755,0.0383066600647174,
0.179962341604654));
#39423=CARTESIAN_POINT('Ctrl Pts',(-0.117966882359366,-1.29211934964912E-5,
0.182563288526384));
#39424=CARTESIAN_POINT('Ctrl Pts',(-0.117968412270431,-1.06668654225827E-5,
0.142436711473616));
#39425=CARTESIAN_POINT('Ctrl Pts',(-0.117969144731522,-0.000578292161741028,
0.142475240435732));
#39426=CARTESIAN_POINT('Ctrl Pts',(-0.117707998838203,-0.0401984655398319,
0.145164604102881));
#39427=CARTESIAN_POINT('Ctrl Pts',(-0.0736248085349355,-0.118238371369349,
0.150504802475065));
#39428=CARTESIAN_POINT('Ctrl Pts',(0.0596315829014974,-0.125876921640408,
0.158457306590168));
#39429=CARTESIAN_POINT('Ctrl Pts',(0.138129079193178,-0.0179243554725553,
0.166409810705271));
#39430=CARTESIAN_POINT('Ctrl Pts',(0.0897844651888838,0.106487909275724,
0.174362314820374));
#39431=CARTESIAN_POINT('Ctrl Pts',(-0.0410080379701501,0.133113732800722,
0.182314818935477));
#39432=CARTESIAN_POINT('Ctrl Pts',(-0.111567175621,0.0606792399755161,0.188339617819891));
#39433=CARTESIAN_POINT('Ctrl Pts',(-0.117821973380904,0.0108165964048154,
0.19171358199927));
#39434=CARTESIAN_POINT('Ctrl Pts',(-0.117728105208174,0.000106637828744488,
0.192436711473616));
#39435=CARTESIAN_POINT('Origin',(0.,0.,-0.0924367114736154));
#39436=CARTESIAN_POINT('',(-0.117616583813332,6.45879523355414E-5,0.0825632885263843));
#39437=CARTESIAN_POINT('',(-0.117696063073914,-0.000101172369946279,0.092436711473616));
#39438=CARTESIAN_POINT('',(-0.117775,-8.88924268665971E-15,-0.0924367114736154));
#39439=CARTESIAN_POINT('Ctrl Pts',(-0.117616583813332,6.4587952335533E-5,
0.0825632885263843));
#39440=CARTESIAN_POINT('Ctrl Pts',(-0.117498290532644,-0.023772899795338,
0.0841689336444552));
#39441=CARTESIAN_POINT('Ctrl Pts',(-0.0988756392612849,-0.087091103874762,
0.0884224643346654));
#39442=CARTESIAN_POINT('Ctrl Pts',(0.00455872999049264,-0.139160029798142,
0.0953238805970148));
#39443=CARTESIAN_POINT('Ctrl Pts',(0.119435794773867,-0.0715642270726515,
0.103267537313433));
#39444=CARTESIAN_POINT('Ctrl Pts',(0.124859895376695,0.0616145512171006,
0.111211194029851));
#39445=CARTESIAN_POINT('Ctrl Pts',(0.0158602180480347,0.138328544685192,
0.119154850746269));
#39446=CARTESIAN_POINT('Ctrl Pts',(-0.094824103560013,0.0934823880103396,
0.126272215578446));
#39447=CARTESIAN_POINT('Ctrl Pts',(-0.117474012159943,0.0269054906934358,
0.130741694838485));
#39448=CARTESIAN_POINT('Ctrl Pts',(-0.117685857408994,-9.79219620674231E-5,
0.132563288526384));
#39449=CARTESIAN_POINT('Ctrl Pts',(-0.117696063073914,-0.000101172369946261,
0.092436711473616));
#39450=CARTESIAN_POINT('Ctrl Pts',(-0.117792623998916,-0.0119605829319943,
0.0932368988721926));
#39451=CARTESIAN_POINT('Ctrl Pts',(-0.110686607712821,-0.0629944099979452,
0.0966879209758034));
#39452=CARTESIAN_POINT('Ctrl Pts',(-0.0371242974264225,-0.134248668971966,
0.102789777784449));
#39453=CARTESIAN_POINT('Ctrl Pts',(0.0928396337021713,-0.10383510521762,
0.110742281899551));
#39454=CARTESIAN_POINT('Ctrl Pts',(0.137550169005636,0.0219289054269618,
0.118694786014654));
#39455=CARTESIAN_POINT('Ctrl Pts',(0.0559501922162531,0.127555870431356,
0.126647290129757));
#39456=CARTESIAN_POINT('Ctrl Pts',(-0.0763838391282559,0.116105719252975,
0.134561265282744));
#39457=CARTESIAN_POINT('Ctrl Pts',(-0.117918750607874,0.0384749486295239,
0.139824405730697));
#39458=CARTESIAN_POINT('Ctrl Pts',(-0.117968412270431,-1.06668654225827E-5,
0.142436711473616));
#39459=CARTESIAN_POINT('Origin',(0.,0.,-0.0924367114736154));
#39460=CARTESIAN_POINT('',(-0.117919967015755,7.48285734863531E-5,0.0325632885263843));
#39461=CARTESIAN_POINT('',(-0.117605093279175,5.63740904734461E-5,0.042436711473616));
#39462=CARTESIAN_POINT('',(-0.117775,-8.88924268665971E-15,-0.0924367114736154));
#39463=CARTESIAN_POINT('Ctrl Pts',(-0.117919967015755,7.48285734863559E-5,
0.0325632885263843));
#39464=CARTESIAN_POINT('Ctrl Pts',(-0.117681732256532,-0.0350969523534404,
0.0349482868782861));
#39465=CARTESIAN_POINT('Ctrl Pts',(-0.0823020584651488,-0.1097611636214,
0.0399811708023271));
#39466=CARTESIAN_POINT('Ctrl Pts',(0.0446654385229893,-0.131869273048715,
0.0476619402985074));
#39467=CARTESIAN_POINT('Ctrl Pts',(0.135042047193827,-0.033912683303242,
0.0556055970149253));
#39468=CARTESIAN_POINT('Ctrl Pts',(0.101666114468308,0.0951356880412728,
0.0635492537313433));
#39469=CARTESIAN_POINT('Ctrl Pts',(-0.0248796065525388,0.136992916606216,
0.0714929104477611));
#39470=CARTESIAN_POINT('Ctrl Pts',(-0.107654697213721,0.0702257630245385,
0.0778309220461081));
#39471=CARTESIAN_POINT('Ctrl Pts',(-0.117693369175918,0.0155377418730691,
0.0815210480723159));
#39472=CARTESIAN_POINT('Ctrl Pts',(-0.117616583813332,6.4587952335533E-5,
0.0825632885263843));
#39473=CARTESIAN_POINT('Ctrl Pts',(-0.117605093279175,5.6374090473453E-5,
0.042436711473616));
#39474=CARTESIAN_POINT('Ctrl Pts',(-0.117506950346121,-0.0231366833782073,
0.0439985573086537));
#39475=CARTESIAN_POINT('Ctrl Pts',(-0.0996401976376468,-0.0858346907547986,
0.0482112378487256));
#39476=CARTESIAN_POINT('Ctrl Pts',(0.00241643506700816,-0.139265216174241,
0.0550747530938317));
#39477=CARTESIAN_POINT('Ctrl Pts',(0.118445458723555,-0.0732914200146354,
0.0630272572089346));
#39478=CARTESIAN_POINT('Ctrl Pts',(0.125708256673902,0.0599868231457294,
0.0709797613240373));
#39479=CARTESIAN_POINT('Ctrl Pts',(0.0175344664057042,0.138178956948752,
0.0789322654391402));
#39480=CARTESIAN_POINT('Ctrl Pts',(-0.0942361274410431,0.0943834610594897,
0.0860845821556665));
#39481=CARTESIAN_POINT('Ctrl Pts',(-0.117472740117216,0.0273268854223547,
0.0905860641671583));
#39482=CARTESIAN_POINT('Ctrl Pts',(-0.117696063073914,-0.000101172369946261,
0.092436711473616));
#39483=CARTESIAN_POINT('Origin',(0.,0.,0.55));
#39484=CARTESIAN_POINT('',(-0.143213254968838,-6.38556725402083E-7,0.507000235761732));
#39485=CARTESIAN_POINT('Ctrl Pts',(-0.0334019664626817,0.112939183906321,
0.532225));
#39486=CARTESIAN_POINT('Ctrl Pts',(-0.025060850432499,0.115799622360937,
0.531847620192936));
#39487=CARTESIAN_POINT('Ctrl Pts',(-0.0164290366846974,0.117635249741265,
0.531473612813392));
#39488=CARTESIAN_POINT('Ctrl Pts',(-0.00767275263448023,0.118510014194121,
0.531100586051555));
#39489=CARTESIAN_POINT('Ctrl Pts',(-0.00421690952474848,0.118855257529045,
0.530953363558858));
#39490=CARTESIAN_POINT('Ctrl Pts',(-0.000739669302851069,0.119050301419728,
0.530806218229583));
#39491=CARTESIAN_POINT('Ctrl Pts',(0.00274357664202706,0.119096927952431,
0.530659241408731));
#39492=CARTESIAN_POINT('Ctrl Pts',(0.00973382066470735,0.119190498962541,
0.5303642855372));
#39493=CARTESIAN_POINT('Ctrl Pts',(0.0167166427004772,0.118687723090435,
0.530071327820757));
#39494=CARTESIAN_POINT('Ctrl Pts',(0.023612882680227,0.11761343656186,0.529779224661465));
#39495=CARTESIAN_POINT('Ctrl Pts',(0.0274136336191392,0.117021360946144,
0.529618236737583));
#39496=CARTESIAN_POINT('Ctrl Pts',(0.0311881579134606,0.116255363574116,
0.529457508384123));
#39497=CARTESIAN_POINT('Ctrl Pts',(0.0349231679080101,0.115317271371855,
0.529296848155877));
#39498=CARTESIAN_POINT('Ctrl Pts',(0.037971953630239,0.114551532560831,
0.529165705639333));
#39499=CARTESIAN_POINT('Ctrl Pts',(0.0409939934565533,0.113670841591964,
0.529034622190513));
#39500=CARTESIAN_POINT('Ctrl Pts',(0.0439689729533011,0.112680856226694,
0.528904071147902));
#39501=CARTESIAN_POINT('Ctrl Pts',(0.0505577881110133,0.110488293021555,
0.528614934133899));
#39502=CARTESIAN_POINT('Ctrl Pts',(0.0569328249215936,0.107756906396238,
0.528327689901185));
#39503=CARTESIAN_POINT('Ctrl Pts',(0.0630179104963209,0.104502120084129,
0.528041256645784));
#39504=CARTESIAN_POINT('Ctrl Pts',(0.0668676595642169,0.102442968997859,
0.527860043720435));
#39505=CARTESIAN_POINT('Ctrl Pts',(0.0706013360983203,0.100173990889927,
0.527679155388847));
#39506=CARTESIAN_POINT('Ctrl Pts',(0.0741982818595768,0.0976957705995567,
0.527498317717128));
#39507=CARTESIAN_POINT('Ctrl Pts',(0.0762868294587642,0.0962568050489885,
0.527393315276118));
#39508=CARTESIAN_POINT('Ctrl Pts',(0.0783301222953497,0.0947465519651971,
0.527288283929736));
#39509=CARTESIAN_POINT('Ctrl Pts',(0.0803210903525092,0.0931669243552789,
0.527183314414725));
#39510=CARTESIAN_POINT('Ctrl Pts',(0.0873333522084643,0.0876034185040368,
0.526813607967904));
#39511=CARTESIAN_POINT('Ctrl Pts',(0.0936466399845286,0.0812254488323135,
0.526447434844115));
#39512=CARTESIAN_POINT('Ctrl Pts',(0.0992257444432458,0.0742158265894858,
0.526082561055055));
#39513=CARTESIAN_POINT('Ctrl Pts',(0.101943770530818,0.0708008813664647,
0.525904801974781));
#39514=CARTESIAN_POINT('Ctrl Pts',(0.104487132714136,0.0672353052679948,
0.525727351283807));
#39515=CARTESIAN_POINT('Ctrl Pts',(0.106849003984973,0.0635370592318222,
0.525549950667934));
#39516=CARTESIAN_POINT('Ctrl Pts',(0.108451822333258,0.0610273472604538,
0.525429562666425));
#39517=CARTESIAN_POINT('Ctrl Pts',(0.109972218146102,0.0584542637442968,
0.525309095710787));
#39518=CARTESIAN_POINT('Ctrl Pts',(0.111403508282751,0.0558304813946845,
0.525188806889777));
#39519=CARTESIAN_POINT('Ctrl Pts',(0.115946659550801,0.0475021629053002,
0.524806990306466));
#39520=CARTESIAN_POINT('Ctrl Pts',(0.119574294719482,0.0387078320373927,
0.524428851599571));
#39521=CARTESIAN_POINT('Ctrl Pts',(0.122229265704535,0.02963297991244,0.524051927142185));
#39522=CARTESIAN_POINT('Ctrl Pts',(0.123491040005696,0.0253201586942182,
0.523872793887439));
#39523=CARTESIAN_POINT('Ctrl Pts',(0.124532521003962,0.0209434889498052,
0.523693934885913));
#39524=CARTESIAN_POINT('Ctrl Pts',(0.125343829183128,0.0165211886089503,
0.523515085689393));
#39525=CARTESIAN_POINT('Ctrl Pts',(0.126073723283802,0.0125426623065107,
0.523354183856031));
#39526=CARTESIAN_POINT('Ctrl Pts',(0.126617185118597,0.00852274589339418,
0.523193115530006));
#39527=CARTESIAN_POINT('Ctrl Pts',(0.126964066890117,0.00450317609134152,
0.523032822082874));
#39528=CARTESIAN_POINT('Ctrl Pts',(0.127610380106321,-0.00298612228009172,
0.522734161899901));
#39529=CARTESIAN_POINT('Ctrl Pts',(0.127580071374667,-0.0104910608890547,
0.522437493943663));
#39530=CARTESIAN_POINT('Ctrl Pts',(0.126833825603371,-0.0179253657039838,
0.52214162882945));
#39531=CARTESIAN_POINT('Ctrl Pts',(0.126370997360361,-0.0225361874571381,
0.521958130662699));
#39532=CARTESIAN_POINT('Ctrl Pts',(0.125632379838884,-0.0271199619342287,
0.521774941316387));
#39533=CARTESIAN_POINT('Ctrl Pts',(0.124632255285918,-0.0316602427367966,
0.52159177704026));
#39534=CARTESIAN_POINT('Ctrl Pts',(0.123677051866189,-0.0359965943804856,
0.521416839686298));
#39535=CARTESIAN_POINT('Ctrl Pts',(0.122480780227546,-0.0402989646849493,
0.521241685776095));
#39536=CARTESIAN_POINT('Ctrl Pts',(0.121065837229724,-0.044520244829744,
0.521067408183846));
#39537=CARTESIAN_POINT('Ctrl Pts',(0.118338362465597,-0.0526572758514579,
0.520731466922931));
#39538=CARTESIAN_POINT('Ctrl Pts',(0.114798640009948,-0.0605127756442529,
0.520398022841861));
#39539=CARTESIAN_POINT('Ctrl Pts',(0.11054080941355,-0.0679858568570343,
0.520065383890604));
#39540=CARTESIAN_POINT('Ctrl Pts',(0.108372779925159,-0.0717910482735648,
0.5198960086562));
#39541=CARTESIAN_POINT('Ctrl Pts',(0.10601800718922,-0.0754969965361626,
0.51972684216845));
#39542=CARTESIAN_POINT('Ctrl Pts',(0.103485875290119,-0.0790891197455118,
0.519557661047695));
#39543=CARTESIAN_POINT('Ctrl Pts',(0.101239265068231,-0.0822761972920135,
0.519407556688845));
#39544=CARTESIAN_POINT('Ctrl Pts',(0.0988505693656959,-0.0853758696950735,
0.519257316754896));
#39545=CARTESIAN_POINT('Ctrl Pts',(0.0963426843438634,-0.0883583266502687,
0.51910776182463));
#39546=CARTESIAN_POINT('Ctrl Pts',(0.0906830843157466,-0.0950889037383469,
0.518770257880003));
#39547=CARTESIAN_POINT('Ctrl Pts',(0.084404823468622,-0.101245530098652,
0.518435260730044));
#39548=CARTESIAN_POINT('Ctrl Pts',(0.077590384105458,-0.106717161154373,
0.51810105566737));
#39549=CARTESIAN_POINT('Ctrl Pts',(0.072812396824573,-0.110553629893275,
0.517866725672845));
#39550=CARTESIAN_POINT('Ctrl Pts',(0.0677701261881638,-0.114053116790221,
0.517632785084427));
#39551=CARTESIAN_POINT('Ctrl Pts',(0.0624852082906241,-0.117169678449436,
0.517398642838002));
#39552=CARTESIAN_POINT('Ctrl Pts',(0.060232694538615,-0.11849800523378,
0.517298847790998));
#39553=CARTESIAN_POINT('Ctrl Pts',(0.0579421351333471,-0.119753052219492,
0.517199285984453));
#39554=CARTESIAN_POINT('Ctrl Pts',(0.0556164103289471,-0.120931647626768,
0.517099943244175));
#39555=CARTESIAN_POINT('Ctrl Pts',(0.0470766353824801,-0.125259304756293,
0.516735168941155));
#39556=CARTESIAN_POINT('Ctrl Pts',(0.0380619111816488,-0.128561628767388,
0.516373216300106));
#39557=CARTESIAN_POINT('Ctrl Pts',(0.0287540615399164,-0.13087769180711,
0.516011917283344));
#39558=CARTESIAN_POINT('Ctrl Pts',(0.0244834739512418,-0.131940337901829,
0.515846147620515));
#39559=CARTESIAN_POINT('Ctrl Pts',(0.0201508023558736,-0.132794720803219,
0.515680515553343));
#39560=CARTESIAN_POINT('Ctrl Pts',(0.0157724288157125,-0.133441328903782,
0.515514811679433));
#39561=CARTESIAN_POINT('Ctrl Pts',(0.0127414878228209,-0.13388894512025,
0.515400102721983));
#39562=CARTESIAN_POINT('Ctrl Pts',(0.0096905970655013,-0.134236406792975,
0.515285434752076));
#39563=CARTESIAN_POINT('Ctrl Pts',(0.00663678161128016,-0.134483505205774,
0.515171166690044));
#39564=CARTESIAN_POINT('Ctrl Pts',(-0.00335208404858516,-0.135291750788136,
0.514797402021565));
#39565=CARTESIAN_POINT('Ctrl Pts',(-0.0134050142894213,-0.135035519709951,
0.514426646108251));
#39566=CARTESIAN_POINT('Ctrl Pts',(-0.0233297246571887,-0.13373576937046,
0.514056571073779));
#39567=CARTESIAN_POINT('Ctrl Pts',(-0.0275876193693317,-0.133178151073044,
0.5138978016514));
#39568=CARTESIAN_POINT('Ctrl Pts',(-0.0318220223293205,-0.132427814053447,
0.513739157550061));
#39569=CARTESIAN_POINT('Ctrl Pts',(-0.0360175989408762,-0.131483472271743,
0.513580454950452));
#39570=CARTESIAN_POINT('Ctrl Pts',(-0.0391091145169674,-0.130787632915777,
0.513463514752696));
#39571=CARTESIAN_POINT('Ctrl Pts',(-0.0421792587373029,-0.12998615137042,
0.513346550232001));
#39572=CARTESIAN_POINT('Ctrl Pts',(-0.0452082926810733,-0.129082949079949,
0.513230012664731));
#39573=CARTESIAN_POINT('Ctrl Pts',(-0.0547989520179786,-0.126223190608758,
0.512861026338271));
#39574=CARTESIAN_POINT('Ctrl Pts',(-0.0640135938008781,-0.122340292920341,
0.512494993993967));
#39575=CARTESIAN_POINT('Ctrl Pts',(-0.0726621826878073,-0.117434240919462,
0.512129678956248));
#39576=CARTESIAN_POINT('Ctrl Pts',(-0.0732258670681981,-0.11711448183293,
0.512105869016456));
#39577=CARTESIAN_POINT('Ctrl Pts',(-0.073787141143001,-0.116790358750658,
0.512082062123761));
#39578=CARTESIAN_POINT('Ctrl Pts',(-0.0743459493499517,-0.11646186427858,
0.5120582576589));
#39579=CARTESIAN_POINT('Ctrl Pts',(-0.0780940452153038,-0.11425855237787,
0.511898593904482));
#39580=CARTESIAN_POINT('Ctrl Pts',(-0.0817313018976771,-0.111858709629848,
0.511739039373249));
#39581=CARTESIAN_POINT('Ctrl Pts',(-0.085250803842968,-0.109275770384611,
0.511579407204066));
#39582=CARTESIAN_POINT('Ctrl Pts',(-0.0875213278289363,-0.107609447819153,
0.511476424260826));
#39583=CARTESIAN_POINT('Ctrl Pts',(-0.0897413530091093,-0.105867722400153,
0.511373470200391));
#39584=CARTESIAN_POINT('Ctrl Pts',(-0.0919020268850941,-0.104060687103246,
0.511270839257698));
#39585=CARTESIAN_POINT('Ctrl Pts',(-0.0994865656445924,-0.0977175136139456,
0.510910577410027));
#39586=CARTESIAN_POINT('Ctrl Pts',(-0.106368098520952,-0.0905540945926997,
0.510553119515254));
#39587=CARTESIAN_POINT('Ctrl Pts',(-0.112476669881714,-0.082740585635558,
0.510196385012091));
#39588=CARTESIAN_POINT('Ctrl Pts',(-0.115701946031867,-0.0786151162581588,
0.510008032086826));
#39589=CARTESIAN_POINT('Ctrl Pts',(-0.118711292938496,-0.0743076837297934,
0.509819880825374));
#39590=CARTESIAN_POINT('Ctrl Pts',(-0.121490605137305,-0.0698396458594739,
0.509631624987483));
#39591=CARTESIAN_POINT('Ctrl Pts',(-0.123158603264919,-0.0671581627195108,
0.509518643658775));
#39592=CARTESIAN_POINT('Ctrl Pts',(-0.124742701375389,-0.0644198867277164,
0.509405676189658));
#39593=CARTESIAN_POINT('Ctrl Pts',(-0.126234357059848,-0.06164059243669,
0.509293097144302));
#39594=CARTESIAN_POINT('Ctrl Pts',(-0.131306921574689,-0.0521892493795411,
0.508910257809098));
#39595=CARTESIAN_POINT('Ctrl Pts',(-0.135335100093566,-0.0422336175385342,
0.508530533331389));
#39596=CARTESIAN_POINT('Ctrl Pts',(-0.138212265982587,-0.0319628814891436,
0.508151426353207));
#39597=CARTESIAN_POINT('Ctrl Pts',(-0.139343321582236,-0.0279253063303673,
0.508002393907016));
#39598=CARTESIAN_POINT('Ctrl Pts',(-0.140295939750969,-0.0238387054236251,
0.507853456888584));
#39599=CARTESIAN_POINT('Ctrl Pts',(-0.14106118303298,-0.0197137190414539,
0.507704463579619));
#39600=CARTESIAN_POINT('Ctrl Pts',(-0.141663078970186,-0.0164692442413196,
0.507587274093027));
#39601=CARTESIAN_POINT('Ctrl Pts',(-0.142148737315268,-0.0132004963364534,
0.507470032942495));
#39602=CARTESIAN_POINT('Ctrl Pts',(-0.14251240365623,-0.00992818124989041,
0.507353216880015));
#39603=CARTESIAN_POINT('Ctrl Pts',(-0.14286252481498,-0.00677774740200931,
0.507240751769694));
#39604=CARTESIAN_POINT('Ctrl Pts',(-0.143100295244155,-0.00362062020727709,
0.507128557913111));
#39605=CARTESIAN_POINT('Ctrl Pts',(-0.143222931917338,-0.0004616047295162,
0.507016572073626));
#39606=CARTESIAN_POINT('Ctrl Pts',(-0.143228895796354,-0.000307980323141247,
0.507011126149655));
#39607=CARTESIAN_POINT('Ctrl Pts',(-0.143234587305958,-0.000154351422170947,
0.50700568071763));
#39608=CARTESIAN_POINT('Ctrl Pts',(-0.143240006909252,-7.18572550341278E-7,
0.507000235770275));
#39609=CARTESIAN_POINT('',(-0.00156805256656782,0.146109107730171,0.50365));
#39610=CARTESIAN_POINT('Ctrl Pts',(-0.0015703316452181,0.146071601053478,
0.50365));
#39611=CARTESIAN_POINT('Ctrl Pts',(-0.0117120407853717,0.144648246558049,
0.504950624278524));
#39612=CARTESIAN_POINT('Ctrl Pts',(-0.0216505365241647,0.142222557694311,
0.506260995613922));
#39613=CARTESIAN_POINT('Ctrl Pts',(-0.0312063389538959,0.13880538472021,
0.507590209176103));
#39614=CARTESIAN_POINT('Ctrl Pts',(-0.0379631701734481,0.136389129130603,
0.508530085419929));
#39615=CARTESIAN_POINT('Ctrl Pts',(-0.0445284394867549,0.133476109724793,
0.50947938238263));
#39616=CARTESIAN_POINT('Ctrl Pts',(-0.050827361354341,0.13005807034167,
0.510441315490383));
#39617=CARTESIAN_POINT('Ctrl Pts',(-0.0535603409840707,0.12857504956382,
0.510858679547901));
#39618=CARTESIAN_POINT('Ctrl Pts',(-0.056235007151428,0.127001156165417,
0.511277203939051));
#39619=CARTESIAN_POINT('Ctrl Pts',(-0.0588447172056459,0.125337452214503,
0.511696981696819));
#39620=CARTESIAN_POINT('Ctrl Pts',(-0.0624191770014244,0.123058715204999,
0.512271941629964));
#39621=CARTESIAN_POINT('Ctrl Pts',(-0.0658727208815536,0.120611069028702,
0.512849385708712));
#39622=CARTESIAN_POINT('Ctrl Pts',(-0.0691906694557284,0.117994047416377,
0.513430106410014));
#39623=CARTESIAN_POINT('Ctrl Pts',(-0.0733832729377804,0.114687144467415,
0.51416391273038));
#39624=CARTESIAN_POINT('Ctrl Pts',(-0.0773595119772722,0.111109779201256,
0.514902950893669));
#39625=CARTESIAN_POINT('Ctrl Pts',(-0.0811052238678245,0.107288843574283,
0.515648819828442));
#39626=CARTESIAN_POINT('Ctrl Pts',(-0.0841017207582698,0.104232169153142,
0.516245500515327));
#39627=CARTESIAN_POINT('Ctrl Pts',(-0.0869506135922833,0.101019546539762,
0.516846552684068));
#39628=CARTESIAN_POINT('Ctrl Pts',(-0.0896425492995218,0.097664267789728,
0.517452794926569));
#39629=CARTESIAN_POINT('Ctrl Pts',(-0.0913307146861822,0.0955601070428074,
0.517832981261246));
#39630=CARTESIAN_POINT('Ctrl Pts',(-0.0929559105919431,0.0934010507133458,
0.518214974249558));
#39631=CARTESIAN_POINT('Ctrl Pts',(-0.094511034598742,0.0911980939617143,
0.518597709131816));
#39632=CARTESIAN_POINT('Ctrl Pts',(-0.0989061554610084,0.0849720559509604,
0.519679401690337));
#39633=CARTESIAN_POINT('Ctrl Pts',(-0.102756278369653,0.0783797189661076,
0.520769927597638));
#39634=CARTESIAN_POINT('Ctrl Pts',(-0.106019480011838,0.0715022869017531,
0.521874709646989));
#39635=CARTESIAN_POINT('Ctrl Pts',(-0.10810684462629,0.0671030159085511,
0.522581403014228));
#39636=CARTESIAN_POINT('Ctrl Pts',(-0.109953633570546,0.0625869322502571,
0.523293929634644));
#39637=CARTESIAN_POINT('Ctrl Pts',(-0.111544021459737,0.0579753350677128,
0.524013708847662));
#39638=CARTESIAN_POINT('Ctrl Pts',(-0.11291963712523,0.0539865060717378,
0.524636286250227));
#39639=CARTESIAN_POINT('Ctrl Pts',(-0.114104149138597,0.0499208096400247,
0.525265113718246));
#39640=CARTESIAN_POINT('Ctrl Pts',(-0.115079157041328,0.0458232444145113,
0.525896440126774));
#39641=CARTESIAN_POINT('Ctrl Pts',(-0.117097797518837,0.0373397121269415,
0.527203528037759));
#39642=CARTESIAN_POINT('Ctrl Pts',(-0.118231089846825,0.0286982113614575,
0.528524583654289));
#39643=CARTESIAN_POINT('Ctrl Pts',(-0.118391363114938,0.0200276346563605,
0.529869408057975));
#39644=CARTESIAN_POINT('Ctrl Pts',(-0.118483921504357,0.0150203453896601,
0.530646048993314));
#39645=CARTESIAN_POINT('Ctrl Pts',(-0.118251089036742,0.0100034984621487,
0.531430617066573));
#39646=CARTESIAN_POINT('Ctrl Pts',(-0.117668597464311,0.00500517689817885,
0.532225));
#39647=CARTESIAN_POINT('',(-0.115076068242798,0.0902060425677366,0.50365));
#39648=CARTESIAN_POINT('Origin',(0.,0.,0.50365));
#39649=CARTESIAN_POINT('Ctrl Pts',(-0.143240006909252,-7.18572550341278E-7,
0.507000235770275));
#39650=CARTESIAN_POINT('Ctrl Pts',(-0.143520908694302,0.00796217822295569,
0.506718020385041));
#39651=CARTESIAN_POINT('Ctrl Pts',(-0.14307308860376,0.0159355469497794,
0.506437106818574));
#39652=CARTESIAN_POINT('Ctrl Pts',(-0.141950240996583,0.0238446282639654,
0.506156482679269));
#39653=CARTESIAN_POINT('Ctrl Pts',(-0.141327877173321,0.0282284164590215,
0.506000940367809));
#39654=CARTESIAN_POINT('Ctrl Pts',(-0.140497759623186,0.0325924948231262,
0.505845486973662));
#39655=CARTESIAN_POINT('Ctrl Pts',(-0.139466483050223,0.0369239027928834,
0.505689950104037));
#39656=CARTESIAN_POINT('Ctrl Pts',(-0.138800760016326,0.0397199694642927,
0.50558954592591));
#39657=CARTESIAN_POINT('Ctrl Pts',(-0.138051361267828,0.0425008441913541,
0.50548916176982));
#39658=CARTESIAN_POINT('Ctrl Pts',(-0.137223245651255,0.0452539885083259,
0.505389082377033));
#39659=CARTESIAN_POINT('Ctrl Pts',(-0.134183880382411,0.0553586297560613,
0.505021769136614));
#39660=CARTESIAN_POINT('Ctrl Pts',(-0.130080477516678,0.06512485891418,
0.504657328869907));
#39661=CARTESIAN_POINT('Ctrl Pts',(-0.125019236367424,0.0743847486871139,
0.504293559587933));
#39662=CARTESIAN_POINT('Ctrl Pts',(-0.122033398952289,0.0798475441810871,
0.504078956904408));
#39663=CARTESIAN_POINT('Ctrl Pts',(-0.118713161823888,0.0851340339476938,
0.503864587744543));
#39664=CARTESIAN_POINT('Ctrl Pts',(-0.115072616245007,0.0902061753896176,
0.50365));
#39665=CARTESIAN_POINT('',(-0.05,-6.12323399573676E-18,0.6));
#39666=CARTESIAN_POINT('',(-0.1,-1.22464679914735E-17,0.55));
#39667=CARTESIAN_POINT('Origin',(0.,0.,0.6));
#39668=CARTESIAN_POINT('Ctrl Pts',(0.0850780204044556,-0.119080027477571,
-0.0164977839420937));
#39669=CARTESIAN_POINT('Ctrl Pts',(0.124701079614845,-0.0907709019978731,
-0.0138498983699544));
#39670=CARTESIAN_POINT('Ctrl Pts',(0.172780327456066,0.00801716155080004,
-0.00855412722567576));
#39671=CARTESIAN_POINT('Ctrl Pts',(0.0867037234097596,0.149857524855506,
-0.000610470509257829));
#39672=CARTESIAN_POINT('Ctrl Pts',(-0.0789008477636886,0.153920736728128,
0.00733318620716008));
#39673=CARTESIAN_POINT('Ctrl Pts',(-0.172161895422237,0.0171520622219753,
0.015276842923578));
#39674=CARTESIAN_POINT('Ctrl Pts',(-0.107670523249975,-0.135451540092597,
0.0232204996399959));
#39675=CARTESIAN_POINT('Ctrl Pts',(0.0555023301026467,-0.163863876974566,
0.0311641563564139));
#39676=CARTESIAN_POINT('Ctrl Pts',(0.167806441153186,-0.042140702198512,
0.0391078130728317));
#39677=CARTESIAN_POINT('Ctrl Pts',(0.126332717914983,0.118217855613161,
0.0470514697892497));
#39678=CARTESIAN_POINT('Ctrl Pts',(-0.0309159874248675,0.170230637616809,
0.0549951265056676));
#39679=CARTESIAN_POINT('Ctrl Pts',(-0.159831956410111,0.066245824895792,
0.0629387832220855));
#39680=CARTESIAN_POINT('Ctrl Pts',(-0.14227559413168,-0.0984502643440673,
0.0708824399385034));
#39681=CARTESIAN_POINT('Ctrl Pts',(0.00566478568548768,-0.172923543714354,
0.0788260966549214));
#39682=CARTESIAN_POINT('Ctrl Pts',(0.148413742858461,-0.0889274008243077,
0.0867697533713393));
#39683=CARTESIAN_POINT('Ctrl Pts',(0.155153858530075,0.0765636983283585,
0.0947134100877573));
#39684=CARTESIAN_POINT('Ctrl Pts',(0.0197082819896427,0.171890320651054,
0.102657066804175));
#39685=CARTESIAN_POINT('Ctrl Pts',(-0.133798285716779,0.109693800981729,
0.110600723520593));
#39686=CARTESIAN_POINT('Ctrl Pts',(-0.164689815771182,-0.0530280538225922,
0.118544380237011));
#39687=CARTESIAN_POINT('Ctrl Pts',(-0.044656766037051,-0.167154062007556,
0.126488036953429));
#39688=CARTESIAN_POINT('Ctrl Pts',(0.11630050845274,-0.128097231996654,
0.134431693669847));
#39689=CARTESIAN_POINT('Ctrl Pts',(0.170678001253376,0.0283501086412318,
0.142375350386265));
#39690=CARTESIAN_POINT('Ctrl Pts',(0.0686432422541576,0.158816918899349,
0.150319007102683));
#39691=CARTESIAN_POINT('Ctrl Pts',(-0.0962973622855325,0.143741179688805,
0.1582626638191));
#39692=CARTESIAN_POINT('Ctrl Pts',(-0.172989410659926,-0.00306144592864502,
0.166206320535519));
#39693=CARTESIAN_POINT('Ctrl Pts',(-0.0911509925455794,-0.147058509343496,
0.174149977251936));
#39694=CARTESIAN_POINT('Ctrl Pts',(0.0742197602705133,-0.1562886299111,
0.182093633968354));
#39695=CARTESIAN_POINT('Ctrl Pts',(0.171574250349044,-0.0222931661803689,
0.190037290684772));
#39696=CARTESIAN_POINT('Ctrl Pts',(0.111695151232628,0.132132137756553,
0.19798094740119));
#39697=CARTESIAN_POINT('Ctrl Pts',(-0.0505433024217535,0.165469281811646,
0.205924604117608));
#39698=CARTESIAN_POINT('Ctrl Pts',(-0.16646300584434,0.0471675346608595,
0.213868260834026));
#39699=CARTESIAN_POINT('Ctrl Pts',(-0.129833152315396,-0.11435935117077,
0.221811917550444));
#39700=CARTESIAN_POINT('Ctrl Pts',(0.0257780314041745,-0.171085363892111,
0.229755574266861));
#39701=CARTESIAN_POINT('Ctrl Pts',(0.157765784501968,-0.0710258113735757,
0.23769923098328));
#39702=CARTESIAN_POINT('Ctrl Pts',(0.145174263631334,0.0941230142947892,
0.245642887699697));
#39703=CARTESIAN_POINT('Ctrl Pts',(-0.000457445268631668,0.173015893445265,
0.253586544416116));
#39704=CARTESIAN_POINT('Ctrl Pts',(-0.145669943468849,0.0933540369270586,
0.261530201132533));
#39705=CARTESIAN_POINT('Ctrl Pts',(-0.15738800412666,-0.0718590620464598,
0.269473857848952));
#39706=CARTESIAN_POINT('Ctrl Pts',(-0.0248729952365478,-0.171219282641631,
0.277417514565369));
#39707=CARTESIAN_POINT('Ctrl Pts',(0.130436053586269,-0.11367121256306,
0.285361171281788));
#39708=CARTESIAN_POINT('Ctrl Pts',(0.166211263149388,0.0480471086044073,
0.293304827998205));
#39709=CARTESIAN_POINT('Ctrl Pts',(0.0496676170739063,0.16573423439711,
0.301248484714623));
#39710=CARTESIAN_POINT('Ctrl Pts',(-0.112392286114514,0.131539661939415,
0.309192141431041));
#39711=CARTESIAN_POINT('Ctrl Pts',(-0.171453968444308,-0.0232001154910803,
0.317135798147459));
#39712=CARTESIAN_POINT('Ctrl Pts',(-0.0733922898759408,-0.156678908596981,
0.325079454863877));
#39713=CARTESIAN_POINT('Ctrl Pts',(0.0919273431499614,-0.146574459688691,
0.333023111580294));
#39714=CARTESIAN_POINT('Ctrl Pts',(0.173003180832518,-0.00214665863879225,
0.340966768296713));
#39715=CARTESIAN_POINT('Ctrl Pts',(0.0955359320753977,0.14424837648421,
0.34891042501313));
#39716=CARTESIAN_POINT('Ctrl Pts',(-0.0694820837435447,0.158451723911329,
0.356854081729549));
#39717=CARTESIAN_POINT('Ctrl Pts',(-0.170825527907542,0.0274471879557805,
0.364797738445966));
#39718=CARTESIAN_POINT('Ctrl Pts',(-0.115621519313607,-0.128710417100276,
0.372741395162384));
#39719=CARTESIAN_POINT('Ctrl Pts',(0.0455400241630207,-0.16691559576681,
0.380685051878803));
#39720=CARTESIAN_POINT('Ctrl Pts',(0.164967928025121,-0.0521564373559641,
0.38862870859522));
#39721=CARTESIAN_POINT('Ctrl Pts',(0.133216350942249,0.110399739828213,
0.396572365311638));
#39722=CARTESIAN_POINT('Ctrl Pts',(-0.0206169035662114,0.171783768167507,
0.404516022028056));
#39723=CARTESIAN_POINT('Ctrl Pts',(-0.155556614414135,0.0757420715232724,
0.412459678744474));
#39724=CARTESIAN_POINT('Ctrl Pts',(-0.14794130513946,-0.0897107128565239,
0.420403335460892));
#39725=CARTESIAN_POINT('Ctrl Pts',(-0.00475055195827078,-0.17295152931105,
0.42834699217731));
#39726=CARTESIAN_POINT('Ctrl Pts',(0.142794654932494,-0.0976957016900834,
0.436290648893728));
#39727=CARTESIAN_POINT('Ctrl Pts',(0.159478551636871,0.0670884478109748,
0.444234305610146));
#39728=CARTESIAN_POINT('Ctrl Pts',(0.0300170551768464,0.170394816235914,
0.452177962326563));
#39729=CARTESIAN_POINT('Ctrl Pts',(-0.126959218666436,0.117542321186412,
0.460121619042982));
#39730=CARTESIAN_POINT('Ctrl Pts',(-0.167575279308382,-0.043016329325927,
0.468065275759399));
#39731=CARTESIAN_POINT('Ctrl Pts',(-0.054646434915416,-0.164176211557628,
0.476008932475817));
#39732=CARTESIAN_POINT('Ctrl Pts',(0.108406899182729,-0.134840111552273,
0.483952589192236));
#39733=CARTESIAN_POINT('Ctrl Pts',(0.172027477869207,0.0179856562492908,
0.491896245908652));
#39734=CARTESIAN_POINT('Ctrl Pts',(0.0781660714022324,0.154482616143293,
0.499839902625072));
#39735=CARTESIAN_POINT('Ctrl Pts',(-0.0876620486424683,0.149106276403653,
0.507783559341488));
#39736=CARTESIAN_POINT('Ctrl Pts',(-0.144148268866352,0.0548725112369506,
0.513079330485768));
#39737=CARTESIAN_POINT('Ctrl Pts',(-0.146217781693075,0.00621955117001058,
0.515727216057907));
#39738=CARTESIAN_POINT('Ctrl Pts',(0.0795408277542857,-0.111329858282327,
-0.0109985226280625));
#39739=CARTESIAN_POINT('Ctrl Pts',(0.116585071529219,-0.0848631955302966,
-0.00835063705592319));
#39740=CARTESIAN_POINT('Ctrl Pts',(0.161535143861813,0.00749537498591264,
-0.00305486591164458));
#39741=CARTESIAN_POINT('Ctrl Pts',(0.0810607239872927,0.140104242147965,
0.00488879080477336));
#39742=CARTESIAN_POINT('Ctrl Pts',(-0.0737656883858339,0.143903005144011,
0.0128324475211912));
#39743=CARTESIAN_POINT('Ctrl Pts',(-0.160956961675077,0.0160357424907528,
0.0207761042376092));
#39744=CARTESIAN_POINT('Ctrl Pts',(-0.100662926844399,-0.12663585222528,
0.028719760954027));
#39745=CARTESIAN_POINT('Ctrl Pts',(0.0518900329094276,-0.153199008999282,
0.0366634176704451));
#39746=CARTESIAN_POINT('Ctrl Pts',(0.156884976500066,-0.039398029233422,
0.0446070743868629));
#39747=CARTESIAN_POINT('Ctrl Pts',(0.118110516766091,0.110523799755865,
0.052550731103281));
#39748=CARTESIAN_POINT('Ctrl Pts',(-0.0289038604674246,0.159151397279945,
0.0604943878196987));
#39749=CARTESIAN_POINT('Ctrl Pts',(-0.149429500757181,0.0619343012734311,
0.0684380445361168));
#39750=CARTESIAN_POINT('Ctrl Pts',(-0.133015771554951,-0.0920427565348621,
0.0763817012525346));
#39751=CARTESIAN_POINT('Ctrl Pts',(0.00529610045382266,-0.161669039075616,
0.0843253579689526));
#39752=CARTESIAN_POINT('Ctrl Pts',(0.138754426830263,-0.0831396762404221,
0.0922690146853704));
#39753=CARTESIAN_POINT('Ctrl Pts',(0.145055870812282,0.0715806492912723,
0.100212671401788));
#39754=CARTESIAN_POINT('Ctrl Pts',(0.0184255940091067,0.160703061995767,
0.108156328118206));
#39755=CARTESIAN_POINT('Ctrl Pts',(-0.125090197766985,0.102554522168261,
0.116099984834624));
#39756=CARTESIAN_POINT('Ctrl Pts',(-0.153971192640191,-0.0495767916930391,
0.124043641551042));
#39757=CARTESIAN_POINT('Ctrl Pts',(-0.0417503383192307,-0.156275056605288,
0.13198729826746));
#39758=CARTESIAN_POINT('Ctrl Pts',(0.108731240649445,-0.119760189736536,
0.139930954983878));
#39759=CARTESIAN_POINT('Ctrl Pts',(0.159569644834255,0.0265049785776333,
0.147874611700296));
#39760=CARTESIAN_POINT('Ctrl Pts',(0.0641756858313974,0.148480525646761,
0.155818268416713));
#39761=CARTESIAN_POINT('Ctrl Pts',(-0.0900299733154633,0.134385971376294,
0.163761925133132));
#39762=CARTESIAN_POINT('Ctrl Pts',(-0.161730619156435,-0.00286219568969563,
0.171705581849549));
#39763=CARTESIAN_POINT('Ctrl Pts',(-0.0852185483775114,-0.137487396931492,
0.179649238565968));
#39764=CARTESIAN_POINT('Ctrl Pts',(0.0693892634028907,-0.14611678706926,
0.187592895282385));
#39765=CARTESIAN_POINT('Ctrl Pts',(0.160407562719562,-0.0208422443637096,
0.195536551998804));
#39766=CARTESIAN_POINT('Ctrl Pts',(0.104425617132929,0.123532488886508,
0.203480208715221));
#39767=CARTESIAN_POINT('Ctrl Pts',(-0.0472537571155211,0.154699928144028,
0.211423865431639));
#39768=CARTESIAN_POINT('Ctrl Pts',(-0.155628976936467,0.0440976968224941,
0.219367522148057));
#39769=CARTESIAN_POINT('Ctrl Pts',(-0.121383129932039,-0.106916421072365,
0.227311178864475));
#39770=CARTESIAN_POINT('Ctrl Pts',(0.0241003016527248,-0.159950494803813,
0.235254835580893));
#39771=CARTESIAN_POINT('Ctrl Pts',(0.147497802968786,-0.0664031885287967,
0.243198492297311));
#39772=CARTESIAN_POINT('Ctrl Pts',(0.135725784908488,0.0879971399445481,
0.251142149013729));
#39773=CARTESIAN_POINT('Ctrl Pts',(-0.000427673036423806,0.161755378344027,
0.259085805730147));
#39774=CARTESIAN_POINT('Ctrl Pts',(-0.136189204066452,0.0872782104717779,
0.267029462446565));
#39775=CARTESIAN_POINT('Ctrl Pts',(-0.147144609939394,-0.067182208161988,
0.274973119162982));
#39776=CARTESIAN_POINT('Ctrl Pts',(-0.0232541685906426,-0.160075697625154,
0.282916775879401));
#39777=CARTESIAN_POINT('Ctrl Pts',(0.12194679215539,-0.106273069073731,
0.290860432595819));
#39778=CARTESIAN_POINT('Ctrl Pts',(0.155393618588418,0.0449200248363383,
0.298804089312236));
#39779=CARTESIAN_POINT('Ctrl Pts',(0.0464350646131678,0.154947636633991,
0.306747746028654));
#39780=CARTESIAN_POINT('Ctrl Pts',(-0.105077379894898,0.122978573589753,
0.314691402745072));
#39781=CARTESIAN_POINT('Ctrl Pts',(-0.160295109206645,-0.021690166054439,
0.32263505946149));
#39782=CARTESIAN_POINT('Ctrl Pts',(-0.0686156478460915,-0.146481664972887,
0.330578716177908));
#39783=CARTESIAN_POINT('Ctrl Pts',(0.0859443712093853,-0.137034851020875,
0.338522372894326));
#39784=CARTESIAN_POINT('Ctrl Pts',(0.161743493115198,-0.00200694614453471,
0.346466029610744));
#39785=CARTESIAN_POINT('Ctrl Pts',(0.0893180998033222,0.134860157925877,
0.354409686327162));
#39786=CARTESIAN_POINT('Ctrl Pts',(-0.0649599324100484,0.148139098901043,
0.36235334304358));
#39787=CARTESIAN_POINT('Ctrl Pts',(-0.159707569907411,0.0256608233143121,
0.370296999759998));
#39788=CARTESIAN_POINT('Ctrl Pts',(-0.108096442638088,-0.120333466482715,
0.378240656476415));
#39789=CARTESIAN_POINT('Ctrl Pts',(0.0425761107352605,-0.156052110630637,
0.386184313192834));
#39790=CARTESIAN_POINT('Ctrl Pts',(0.154231204318669,-0.0487619032540464,
0.394127969909251));
#39791=CARTESIAN_POINT('Ctrl Pts',(0.124546137462748,0.103214515900207,
0.402071626625669));
#39792=CARTESIAN_POINT('Ctrl Pts',(-0.0192750791284384,0.160603444342461,
0.410015283342087));
#39793=CARTESIAN_POINT('Ctrl Pts',(-0.145432413851821,0.0708124970015145,
0.417958940058505));
#39794=CARTESIAN_POINT('Ctrl Pts',(-0.138312737107664,-0.0838720074246256,
0.425902596774923));
#39795=CARTESIAN_POINT('Ctrl Pts',(-0.00444136844339109,-0.161695203266036,
0.433846253491342));
#39796=CARTESIAN_POINT('Ctrl Pts',(0.133501049956532,-0.0913373036128839,
0.441789910207758));
#39797=CARTESIAN_POINT('Ctrl Pts',(0.1490990968754,0.0627220831686826,0.449733566924177));
#39798=CARTESIAN_POINT('Ctrl Pts',(0.0280634340592545,0.159304890546491,
0.457677223640594));
#39799=CARTESIAN_POINT('Ctrl Pts',(-0.118696242528426,0.109892231611416,
0.465620880357014));
#39800=CARTESIAN_POINT('Ctrl Pts',(-0.156668859524218,-0.0402166673045443,
0.47356453707343));
#39801=CARTESIAN_POINT('Ctrl Pts',(-0.0510898425507461,-0.153491015690964,
0.481508193789849));
#39802=CARTESIAN_POINT('Ctrl Pts',(0.101351376704318,-0.126064217718754,
0.489451850506266));
#39803=CARTESIAN_POINT('Ctrl Pts',(0.160831292514208,0.0168150831315976,
0.497395507222684));
#39804=CARTESIAN_POINT('Ctrl Pts',(0.0730787339911879,0.144428315365945,
0.505339163939102));
#39805=CARTESIAN_POINT('Ctrl Pts',(-0.0819566778647476,0.13940188772757,
0.51328282065552));
#39806=CARTESIAN_POINT('Ctrl Pts',(-0.134766565682532,0.0513012049880128,
0.518578591799799));
#39807=CARTESIAN_POINT('Ctrl Pts',(-0.136701386950153,0.005814759746065,
0.521226477371938));
#39808=CARTESIAN_POINT('Ctrl Pts',(0.0740036351041157,-0.103579689087084,
-0.00549926131403131));
#39809=CARTESIAN_POINT('Ctrl Pts',(0.108469063443593,-0.0789554890627202,
-0.00285137574189201));
#39810=CARTESIAN_POINT('Ctrl Pts',(0.150289960267559,0.00697358842102527,
0.00244439540238661));
#39811=CARTESIAN_POINT('Ctrl Pts',(0.0754177245648256,0.130350959440424,
0.0103880521188046));
#39812=CARTESIAN_POINT('Ctrl Pts',(-0.0686305290079791,0.133885273559895,
0.0183317088352224));
#39813=CARTESIAN_POINT('Ctrl Pts',(-0.149752027927918,0.0149194227595303,
0.0262753655516404));
#39814=CARTESIAN_POINT('Ctrl Pts',(-0.0936553304388222,-0.117820164357962,
0.0342190222680582));
#39815=CARTESIAN_POINT('Ctrl Pts',(0.0482777357162085,-0.142534141023999,
0.0421626789844763));
#39816=CARTESIAN_POINT('Ctrl Pts',(0.145963511846947,-0.036655356268332,
0.050106335700894));
#39817=CARTESIAN_POINT('Ctrl Pts',(0.1098883156172,0.102829743898569,0.0580499924173122));
#39818=CARTESIAN_POINT('Ctrl Pts',(-0.0268917335099817,0.14807215694308,
0.0659936491337298));
#39819=CARTESIAN_POINT('Ctrl Pts',(-0.139027045104252,0.0576227776510703,
0.073937305850148));
#39820=CARTESIAN_POINT('Ctrl Pts',(-0.123755948978222,-0.0856352487256572,
0.0818809625665656));
#39821=CARTESIAN_POINT('Ctrl Pts',(0.00492741522215772,-0.150414534436879,
0.0898246192829839));
#39822=CARTESIAN_POINT('Ctrl Pts',(0.129095110802064,-0.0773519516565369,
0.0977682759994015));
#39823=CARTESIAN_POINT('Ctrl Pts',(0.134957883094489,0.0665976002541865,
0.10571193271582));
#39824=CARTESIAN_POINT('Ctrl Pts',(0.0171429060285707,0.14951580334048,
0.113655589432237));
#39825=CARTESIAN_POINT('Ctrl Pts',(-0.116382109817192,0.0954152433547932,
0.121599246148655));
#39826=CARTESIAN_POINT('Ctrl Pts',(-0.1432525695092,-0.046125529563486,
0.129542902865073));
#39827=CARTESIAN_POINT('Ctrl Pts',(-0.0388439106014103,-0.14539605120302,
0.137486559581491));
#39828=CARTESIAN_POINT('Ctrl Pts',(0.101161972846149,-0.111423147476419,
0.145430216297909));
#39829=CARTESIAN_POINT('Ctrl Pts',(0.148461288415133,0.0246598485140348,
0.153373873014327));
#39830=CARTESIAN_POINT('Ctrl Pts',(0.0597081294086373,0.138144132394173,
0.161317529730745));
#39831=CARTESIAN_POINT('Ctrl Pts',(-0.0837625843453943,0.125030763063784,
0.169261186447163));
#39832=CARTESIAN_POINT('Ctrl Pts',(-0.150471827652945,-0.00266294545074625,
0.177204843163581));
#39833=CARTESIAN_POINT('Ctrl Pts',(-0.0792861042094436,-0.127916284519489,
0.185148499879999));
#39834=CARTESIAN_POINT('Ctrl Pts',(0.0645587665352683,-0.13594494422742,
0.193092156596417));
#39835=CARTESIAN_POINT('Ctrl Pts',(0.149240875090081,-0.01939132254705,
0.201035813312835));
#39836=CARTESIAN_POINT('Ctrl Pts',(0.0971560830332309,0.114932840016463,
0.208979470029252));
#39837=CARTESIAN_POINT('Ctrl Pts',(-0.0439642118092888,0.143930574476409,
0.216923126745671));
#39838=CARTESIAN_POINT('Ctrl Pts',(-0.144794948028593,0.0410278589841287,
0.224866783462088));
#39839=CARTESIAN_POINT('Ctrl Pts',(-0.112933107548683,-0.0994734909739605,
0.232810440178506));
#39840=CARTESIAN_POINT('Ctrl Pts',(0.0224225719012751,-0.148815625715515,
0.240754096894924));
#39841=CARTESIAN_POINT('Ctrl Pts',(0.137229821435604,-0.0617805656840178,
0.248697753611342));
#39842=CARTESIAN_POINT('Ctrl Pts',(0.126277306185642,0.081871265594307,
0.25664141032776));
#39843=CARTESIAN_POINT('Ctrl Pts',(-0.000397900804215911,0.150494863242789,
0.264585067044178));
#39844=CARTESIAN_POINT('Ctrl Pts',(-0.126708464664056,0.0812023840164973,
0.272528723760596));
#39845=CARTESIAN_POINT('Ctrl Pts',(-0.136901215752127,-0.0625053542775162,
0.280472380477014));
#39846=CARTESIAN_POINT('Ctrl Pts',(-0.0216353419447375,-0.148932112608676,
0.288416037193432));
#39847=CARTESIAN_POINT('Ctrl Pts',(0.113457530724511,-0.0988749255844029,
0.29635969390985));
#39848=CARTESIAN_POINT('Ctrl Pts',(0.144575974027448,0.0417929410682694,
0.304303350626268));
#39849=CARTESIAN_POINT('Ctrl Pts',(0.0432025121524296,0.144161038870872,
0.312247007342686));
#39850=CARTESIAN_POINT('Ctrl Pts',(-0.0977624736752833,0.114417485240091,
0.320190664059103));
#39851=CARTESIAN_POINT('Ctrl Pts',(-0.149136249968981,-0.0201802166177978,
0.328134320775522));
#39852=CARTESIAN_POINT('Ctrl Pts',(-0.0638390058162424,-0.136284421348793,
0.336077977491939));
#39853=CARTESIAN_POINT('Ctrl Pts',(0.0799613992688094,-0.127495242353059,
0.344021634208357));
#39854=CARTESIAN_POINT('Ctrl Pts',(0.150483805397878,-0.00186723365027712,
0.351965290924775));
#39855=CARTESIAN_POINT('Ctrl Pts',(0.0831002675312467,0.125471939367544,
0.359908947641193));
#39856=CARTESIAN_POINT('Ctrl Pts',(-0.0604377810765522,0.137826473890756,
0.367852604357611));
#39857=CARTESIAN_POINT('Ctrl Pts',(-0.148589611907278,0.0238744586728436,
0.375796261074029));
#39858=CARTESIAN_POINT('Ctrl Pts',(-0.100571365962569,-0.111956515865154,
0.383739917790446));
#39859=CARTESIAN_POINT('Ctrl Pts',(0.0396121973075005,-0.145188625494464,
0.391683574506865));
#39860=CARTESIAN_POINT('Ctrl Pts',(0.143494480612217,-0.0453673691521286,
0.399627231223282));
#39861=CARTESIAN_POINT('Ctrl Pts',(0.115875923983247,0.0960292919722012,
0.407570887939701));
#39862=CARTESIAN_POINT('Ctrl Pts',(-0.0179332546906655,0.149423120517415,
0.415514544656118));
#39863=CARTESIAN_POINT('Ctrl Pts',(-0.135308213289508,0.0658829224797566,
0.423458201372536));
#39864=CARTESIAN_POINT('Ctrl Pts',(-0.128684169075867,-0.0780333019927274,
0.431401858088955));
#39865=CARTESIAN_POINT('Ctrl Pts',(-0.0041321849285115,-0.150438877221023,
0.439345514805372));
#39866=CARTESIAN_POINT('Ctrl Pts',(0.124207444980571,-0.0849789055356846,
0.44728917152179));
#39867=CARTESIAN_POINT('Ctrl Pts',(0.13871964211393,0.0583557185263908,
0.455232828238208));
#39868=CARTESIAN_POINT('Ctrl Pts',(0.0261098129416626,0.148214964857068,
0.463176484954626));
#39869=CARTESIAN_POINT('Ctrl Pts',(-0.110433266390416,0.10224214203642,
0.471120141671043));
#39870=CARTESIAN_POINT('Ctrl Pts',(-0.145762439740054,-0.0374170052831618,
0.479063798387463));
#39871=CARTESIAN_POINT('Ctrl Pts',(-0.0475332501860763,-0.142805819824299,
0.487007455103879));
#39872=CARTESIAN_POINT('Ctrl Pts',(0.0942958542259076,-0.117288323885235,
0.494951111820298));
#39873=CARTESIAN_POINT('Ctrl Pts',(0.149635107159208,0.0156445100139045,
0.502894768536715));
#39874=CARTESIAN_POINT('Ctrl Pts',(0.0679913965801436,0.134374014588598,
0.510838425253134));
#39875=CARTESIAN_POINT('Ctrl Pts',(-0.0762513070870269,0.129697499051486,
0.518782081969551));
#39876=CARTESIAN_POINT('Ctrl Pts',(-0.125384862498713,0.0477298987390752,
0.52407785311383));
#39877=CARTESIAN_POINT('Ctrl Pts',(-0.127184992207232,0.00540996832211942,
0.526725738685969));
#39878=CARTESIAN_POINT('Ctrl Pts',(0.0684664424539458,-0.0958295198918399,
-1.2490009027033E-16));
#39879=CARTESIAN_POINT('Ctrl Pts',(0.100353055357967,-0.0730477825951437,
0.00264788557213918));
#39880=CARTESIAN_POINT('Ctrl Pts',(0.139044776673305,0.00645180185613777,
0.00794365671641779));
#39881=CARTESIAN_POINT('Ctrl Pts',(0.0697747251423586,0.120597676732883,
0.0158873134328358));
#39882=CARTESIAN_POINT('Ctrl Pts',(-0.0634953696301243,0.123867541975778,
0.0238309701492536));
#39883=CARTESIAN_POINT('Ctrl Pts',(-0.138547094180758,0.0138031030283078,
0.0317746268656716));
#39884=CARTESIAN_POINT('Ctrl Pts',(-0.0866477340332458,-0.109004476490645,
0.0397182835820895));
#39885=CARTESIAN_POINT('Ctrl Pts',(0.0446654385229893,-0.131869273048715,
0.0476619402985074));
#39886=CARTESIAN_POINT('Ctrl Pts',(0.135042047193827,-0.033912683303242,
0.0556055970149253));
#39887=CARTESIAN_POINT('Ctrl Pts',(0.101666114468308,0.0951356880412728,
0.0635492537313433));
#39888=CARTESIAN_POINT('Ctrl Pts',(-0.0248796065525388,0.136992916606216,
0.0714929104477611));
#39889=CARTESIAN_POINT('Ctrl Pts',(-0.128624589451322,0.0533112540287094,
0.079436567164179));
#39890=CARTESIAN_POINT('Ctrl Pts',(-0.114496126401493,-0.079227740916452,
0.087380223880597));
#39891=CARTESIAN_POINT('Ctrl Pts',(0.00455872999049264,-0.139160029798142,
0.0953238805970148));
#39892=CARTESIAN_POINT('Ctrl Pts',(0.119435794773867,-0.0715642270726515,
0.103267537313433));
#39893=CARTESIAN_POINT('Ctrl Pts',(0.124859895376695,0.0616145512171006,
0.111211194029851));
#39894=CARTESIAN_POINT('Ctrl Pts',(0.0158602180480347,0.138328544685192,
0.119154850746269));
#39895=CARTESIAN_POINT('Ctrl Pts',(-0.107674021867399,0.0882759645413252,
0.127098507462686));
#39896=CARTESIAN_POINT('Ctrl Pts',(-0.132533946378209,-0.0426742674339329,
0.135042164179105));
#39897=CARTESIAN_POINT('Ctrl Pts',(-0.03593748288359,-0.134517045800752,
0.142985820895522));
#39898=CARTESIAN_POINT('Ctrl Pts',(0.0935927050428541,-0.103086105216301,
0.150929477611941));
#39899=CARTESIAN_POINT('Ctrl Pts',(0.137352931996012,0.0228147184504364,
0.158873134328358));
#39900=CARTESIAN_POINT('Ctrl Pts',(0.0552405729858772,0.127807739141585,
0.166816791044776));
#39901=CARTESIAN_POINT('Ctrl Pts',(-0.0774951953753252,0.115675554751273,
0.174760447761194));
#39902=CARTESIAN_POINT('Ctrl Pts',(-0.139213036149455,-0.00246369521179678,
0.182704104477612));
#39903=CARTESIAN_POINT('Ctrl Pts',(-0.0733536600413758,-0.118345172107485,
0.19064776119403));
#39904=CARTESIAN_POINT('Ctrl Pts',(0.0597282696676458,-0.12577310138558,
0.198591417910448));
#39905=CARTESIAN_POINT('Ctrl Pts',(0.138074187460599,-0.0179404007303906,
0.206535074626866));
#39906=CARTESIAN_POINT('Ctrl Pts',(0.0898865489335327,0.106333191146418,
0.214478731343283));
#39907=CARTESIAN_POINT('Ctrl Pts',(-0.0406746665030564,0.133161220808791,
0.222422388059702));
#39908=CARTESIAN_POINT('Ctrl Pts',(-0.133960919120719,0.0379580211457631,
0.230366044776119));
#39909=CARTESIAN_POINT('Ctrl Pts',(-0.104483085165326,-0.0920305608755558,
0.238309701492537));
#39910=CARTESIAN_POINT('Ctrl Pts',(0.0207448421498254,-0.137680756627218,
0.246253358208955));
#39911=CARTESIAN_POINT('Ctrl Pts',(0.126961839902422,-0.0571579428392388,
0.254197014925373));
#39912=CARTESIAN_POINT('Ctrl Pts',(0.116828827462796,0.075745391244066,
0.262140671641791));
#39913=CARTESIAN_POINT('Ctrl Pts',(-0.000368128572008151,0.139234348141551,
0.270084328358209));
#39914=CARTESIAN_POINT('Ctrl Pts',(-0.117227725261659,0.0751265575612168,
0.278027985074627));
#39915=CARTESIAN_POINT('Ctrl Pts',(-0.12665782156486,-0.0578285003930446,
0.285971641791045));
#39916=CARTESIAN_POINT('Ctrl Pts',(-0.0200165152988323,-0.137788527592198,
0.293915298507463));
#39917=CARTESIAN_POINT('Ctrl Pts',(0.104968269293632,-0.0914767820950745,
0.301858955223881));
#39918=CARTESIAN_POINT('Ctrl Pts',(0.133758329466478,0.0386658573002006,
0.309802611940298));
#39919=CARTESIAN_POINT('Ctrl Pts',(0.0399699596916912,0.133374441107753,
0.317746268656717));
#39920=CARTESIAN_POINT('Ctrl Pts',(-0.0904475674556682,0.10585639689043,
0.325689925373134));
#39921=CARTESIAN_POINT('Ctrl Pts',(-0.137977390731318,-0.0186702671811566,
0.333633582089553));
#39922=CARTESIAN_POINT('Ctrl Pts',(-0.0590623637863932,-0.126087177724698,
0.34157723880597));
#39923=CARTESIAN_POINT('Ctrl Pts',(0.0739784273282333,-0.117955633685244,
0.349520895522388));
#39924=CARTESIAN_POINT('Ctrl Pts',(0.139224117680559,-0.00172752115601949,
0.357464552238807));
#39925=CARTESIAN_POINT('Ctrl Pts',(0.0768824352591712,0.11608372080921,
0.365408208955224));
#39926=CARTESIAN_POINT('Ctrl Pts',(-0.0559156297430559,0.12751384888047,
0.373351865671643));
#39927=CARTESIAN_POINT('Ctrl Pts',(-0.137471653907146,0.0220880940313751,
0.381295522388059));
#39928=CARTESIAN_POINT('Ctrl Pts',(-0.0930462892870504,-0.103579565247593,
0.389239179104478));
#39929=CARTESIAN_POINT('Ctrl Pts',(0.0366482838797405,-0.134325140358292,
0.397182835820896));
#39930=CARTESIAN_POINT('Ctrl Pts',(0.132757756905765,-0.0419728350502109,
0.405126492537314));
#39931=CARTESIAN_POINT('Ctrl Pts',(0.107205710503746,0.0888440680441954,
0.413070149253731));
#39932=CARTESIAN_POINT('Ctrl Pts',(-0.0165914302528927,0.138242796692368,
0.42101380597015));
#39933=CARTESIAN_POINT('Ctrl Pts',(-0.125184012727194,0.0609533479579989,
0.428957462686568));
#39934=CARTESIAN_POINT('Ctrl Pts',(-0.119055601044071,-0.0721945965608292,
0.436901119402986));
#39935=CARTESIAN_POINT('Ctrl Pts',(-0.00382300141363195,-0.139182551176009,
0.444844776119403));
#39936=CARTESIAN_POINT('Ctrl Pts',(0.11491384000461,-0.0786205074584852,
0.452788432835821));
#39937=CARTESIAN_POINT('Ctrl Pts',(0.128340187352459,0.0539893538840985,
0.460732089552239));
#39938=CARTESIAN_POINT('Ctrl Pts',(0.024156191824071,0.137125039167645,
0.468675746268657));
#39939=CARTESIAN_POINT('Ctrl Pts',(-0.102170290252407,0.094592052461424,
0.476619402985075));
#39940=CARTESIAN_POINT('Ctrl Pts',(-0.13485601995589,-0.0346173432617789,
0.484563059701493));
#39941=CARTESIAN_POINT('Ctrl Pts',(-0.0439766578214066,-0.132120623957634,
0.492506716417911));
#39942=CARTESIAN_POINT('Ctrl Pts',(0.087240331747497,-0.108512430051717,
0.500450373134329));
#39943=CARTESIAN_POINT('Ctrl Pts',(0.138438921804208,0.0144739368962113,
0.508394029850746));
#39944=CARTESIAN_POINT('Ctrl Pts',(0.0629040591690992,0.12431971381125,
0.516337686567165));
#39945=CARTESIAN_POINT('Ctrl Pts',(-0.0705459363093062,0.119993110375402,
0.524281343283582));
#39946=CARTESIAN_POINT('Ctrl Pts',(-0.116003159314893,0.0441585924901374,
0.529577114427861));
#39947=CARTESIAN_POINT('Ctrl Pts',(-0.117668597464311,0.00500517689817385,
0.532225));
#39948=CARTESIAN_POINT('',(0.0684664424539457,-0.0958295198918399,0.));
#39949=CARTESIAN_POINT('Ctrl Pts',(0.0684664424539458,-0.0958295198918399,
-1.2490009027033E-16));
#39950=CARTESIAN_POINT('Ctrl Pts',(0.100353055357967,-0.0730477825951437,
0.00264788557213918));
#39951=CARTESIAN_POINT('Ctrl Pts',(0.139044776673305,0.00645180185613777,
0.00794365671641779));
#39952=CARTESIAN_POINT('Ctrl Pts',(0.0697747251423586,0.120597676732883,
0.0158873134328358));
#39953=CARTESIAN_POINT('Ctrl Pts',(-0.0634953696301243,0.123867541975778,
0.0238309701492536));
#39954=CARTESIAN_POINT('Ctrl Pts',(-0.116013612970437,0.0468487789511056,
0.0293896285137698));
#39955=CARTESIAN_POINT('Ctrl Pts',(-0.117946226519694,0.00395164958315818,
0.0323004013061468));
#39956=CARTESIAN_POINT('Ctrl Pts',(-0.117919967015755,7.48285734863559E-5,
0.0325632885263843));
#39957=CARTESIAN_POINT('Ctrl Pts',(0.0635548502597316,0.132093933345895,
7.26415455565288E-18));
#39958=CARTESIAN_POINT('Ctrl Pts',(0.0667625318922158,0.13018322972067,
8.97431508554919E-18));
#39959=CARTESIAN_POINT('Ctrl Pts',(0.0698866263065284,0.128144700630429,
-1.82766240468292E-17));
#39960=CARTESIAN_POINT('Ctrl Pts',(0.0729183991770622,0.125977863427922,
-1.55040910665427E-17));
#39961=CARTESIAN_POINT('Ctrl Pts',(0.0787736058599248,0.121793090949712,
-9.35723626730848E-18));
#39962=CARTESIAN_POINT('Ctrl Pts',(0.0842851176408076,0.117130107773036,
-2.42858544627756E-17));
#39963=CARTESIAN_POINT('Ctrl Pts',(0.0894225077026563,0.112048986470911,
-3.0140820395097E-17));
#39964=CARTESIAN_POINT('Ctrl Pts',(0.0927550575340165,0.108752937361409,
-3.39388512036349E-17));
#39965=CARTESIAN_POINT('Ctrl Pts',(0.095930929613759,0.105278801629612,
-4.52445550988079E-17));
#39966=CARTESIAN_POINT('Ctrl Pts',(0.0989262797420343,0.101660133512415,
-3.46944695195361E-17));
#39967=CARTESIAN_POINT('Ctrl Pts',(0.103069367071931,0.0966548895891983,
-2.01018763264428E-17));
#39968=CARTESIAN_POINT('Ctrl Pts',(0.106874603061403,0.0913668016366946,
-3.77038544403596E-17));
#39969=CARTESIAN_POINT('Ctrl Pts',(0.110317478847291,0.0858396385675292,
-3.33934269125535E-17));
#39970=CARTESIAN_POINT('Ctrl Pts',(0.112268215177796,0.082707943300496,
-3.09511350317464E-17));
#39971=CARTESIAN_POINT('Ctrl Pts',(0.114103333501928,0.079497785539906,
-4.97099315558713E-17));
#39972=CARTESIAN_POINT('Ctrl Pts',(0.115814486180912,0.0762220963964089,
-4.59701721133854E-17));
#39973=CARTESIAN_POINT('Ctrl Pts',(0.120425861906472,0.0673944601566279,
-3.58919154362862E-17));
#39974=CARTESIAN_POINT('Ctrl Pts',(0.124112940735196,0.0581470311761757,
-7.4029188042833E-18));
#39975=CARTESIAN_POINT('Ctrl Pts',(0.126786742395323,0.0486381528803429,
-1.99493199737333E-17));
#39976=CARTESIAN_POINT('Ctrl Pts',(0.128289456800478,0.0432940285927791,
-2.70005751402403E-17));
#39977=CARTESIAN_POINT('Ctrl Pts',(0.129471235246761,0.0378670663167402,
-8.81130640021771E-18));
#39978=CARTESIAN_POINT('Ctrl Pts',(0.130308765287913,0.0323855967712197,
-1.47451495458029E-17));
#39979=CARTESIAN_POINT('Ctrl Pts',(0.130909407220836,0.0284545133457784,
-1.90006566219738E-17));
#39980=CARTESIAN_POINT('Ctrl Pts',(0.131332629221345,0.0244917931761562,
-4.99383881545994E-18));
#39981=CARTESIAN_POINT('Ctrl Pts',(0.1315678106143,0.0205341495544984,-6.07153216591882E-18));
#39982=CARTESIAN_POINT('Ctrl Pts',(0.131851015138327,0.015768370408227,
-7.36928633144951E-18));
#39983=CARTESIAN_POINT('Ctrl Pts',(0.131863254926577,0.0110027231344166,
-1.87693227394301E-17));
#39984=CARTESIAN_POINT('Ctrl Pts',(0.131591710623677,0.00625556877829329,
-1.38777878078145E-17));
#39985=CARTESIAN_POINT('Ctrl Pts',(0.131146495407245,-0.00152771126671145,
-5.8577860622257E-18));
#39986=CARTESIAN_POINT('Ctrl Pts',(0.12993932260643,-0.00926206422336292,
-1.85374582714576E-17));
#39987=CARTESIAN_POINT('Ctrl Pts',(0.128016835267175,-0.0168585737917118,
-1.04083408558608E-17));
#39988=CARTESIAN_POINT('Ctrl Pts',(0.126984115402176,-0.0209392593575938,
-6.04154952851233E-18));
#39989=CARTESIAN_POINT('Ctrl Pts',(0.125742427413826,-0.0249846391579523,
1.89772622437785E-17));
#39990=CARTESIAN_POINT('Ctrl Pts',(0.124308621487175,-0.0289511201777135,
1.38777878078145E-17));
#39991=CARTESIAN_POINT('Ctrl Pts',(0.121785637190381,-0.0359307044717815,
4.90454136999372E-18));
#39992=CARTESIAN_POINT('Ctrl Pts',(0.118666317325564,-0.042682712152767,
2.07260850608487E-18));
#39993=CARTESIAN_POINT('Ctrl Pts',(0.114994151346376,-0.0491304207397526,
8.67361737988404E-18));
#39994=CARTESIAN_POINT('Ctrl Pts',(0.112470213235982,-0.0535620334499726,
1.32105958166033E-17));
#39995=CARTESIAN_POINT('Ctrl Pts',(0.109684704250007,-0.0578497076893306,
-2.69424258846107E-17));
#39996=CARTESIAN_POINT('Ctrl Pts',(0.106648013733876,-0.0619641182107045,
-2.60208521396521E-17));
#39997=CARTESIAN_POINT('Ctrl Pts',(0.104460102807982,-0.0649285176730499,
-2.53568657192706E-17));
#39998=CARTESIAN_POINT('Ctrl Pts',(0.102139560475227,-0.0678046962501359,
-1.87244270863087E-17));
#39999=CARTESIAN_POINT('Ctrl Pts',(0.0997061632112326,-0.0705633954799611,
-1.90819582357449E-17));
#40000=CARTESIAN_POINT('Ctrl Pts',(0.0939222145804643,-0.0771205552455056,
-1.9931775005426E-17));
#40001=CARTESIAN_POINT('Ctrl Pts',(0.087486631308301,-0.0830406987797476,
-2.77894727952103E-19));
#40002=CARTESIAN_POINT('Ctrl Pts',(0.0804584136226653,-0.0881761753022089,
-1.73472347597681E-18));
#40003=CARTESIAN_POINT('Ctrl Pts',(0.0766344364937381,-0.0909703324621629,
-2.52736822068868E-18));
#40004=CARTESIAN_POINT('Ctrl Pts',(0.0726345968903183,-0.0935314830199203,
-1.19936303452846E-17));
#40005=CARTESIAN_POINT('Ctrl Pts',(0.0684664424539472,-0.0958295198918389,
-1.04083408558608E-17));
#40006=CARTESIAN_POINT('Ctrl Pts',(-0.00157033164522019,0.146071601053478,
0.50365));
#40007=CARTESIAN_POINT('Ctrl Pts',(0.0218930565124332,0.146360870028846,
0.502379967541691));
#40008=CARTESIAN_POINT('Ctrl Pts',(0.0454120282149095,0.141318853716995,
0.501109935083381));
#40009=CARTESIAN_POINT('Ctrl Pts',(0.0661716191392787,0.130837066204352,
0.499839902625071));
#40010=CARTESIAN_POINT('Ctrl Pts',(0.109453206891224,0.108983629511958,
0.497192017052932));
#40011=CARTESIAN_POINT('Ctrl Pts',(0.140740342380216,0.0634846428806245,
0.494544131480792));
#40012=CARTESIAN_POINT('Ctrl Pts',(0.145780480343632,0.0152641882646972,
0.491896245908653));
#40013=CARTESIAN_POINT('Ctrl Pts',(0.150820618307048,-0.0329562663512301,
0.489248360336514));
#40014=CARTESIAN_POINT('Ctrl Pts',(0.129613758744889,-0.0838981889517511,
0.486600474764375));
#40015=CARTESIAN_POINT('Ctrl Pts',(0.0918347732807851,-0.114258500252904,
0.483952589192235));
#40016=CARTESIAN_POINT('Ctrl Pts',(0.0540557878166811,-0.144618811554058,
0.481304703620096));
#40017=CARTESIAN_POINT('Ctrl Pts',(-0.000295323549367926,-0.154397511555843,
0.478656818047957));
#40018=CARTESIAN_POINT('Ctrl Pts',(-0.0462923532978867,-0.139093547851452,
0.476008932475817));
#40019=CARTESIAN_POINT('Ctrl Pts',(-0.0922893830464049,-0.123789584147061,
0.473361046903678));
#40020=CARTESIAN_POINT('Ctrl Pts',(-0.129932331177393,-0.0834029567364939,
0.470713161331538));
#40021=CARTESIAN_POINT('Ctrl Pts',(-0.141984461802563,-0.0364498679458208,
0.468065275759399));
#40022=CARTESIAN_POINT('Ctrl Pts',(-0.145018518318758,-0.0246296902999453,
0.467398685367696));
#40023=CARTESIAN_POINT('Ctrl Pts',(-0.146430750426956,-0.0123933615350992,
0.466732094975993));
#40024=CARTESIAN_POINT('Ctrl Pts',(-0.146320034481408,-0.000132042578932776,
0.466065504584291));
#40025=CARTESIAN_POINT('Origin',(0.,0.,-0.0924367114736154));
#40026=CARTESIAN_POINT('',(-0.0684664424539447,-0.0958295198918406,0.));
#40027=CARTESIAN_POINT('Ctrl Pts',(-0.0686153921261821,-0.095961513397809,
-8.6871699070401E-17));
#40028=CARTESIAN_POINT('Ctrl Pts',(-0.0390777571216276,-0.11683521110507,
0.00245324280107157));
#40029=CARTESIAN_POINT('Ctrl Pts',(0.0440758903380829,-0.130444567971902,
0.00755732030717748));
#40030=CARTESIAN_POINT('Ctrl Pts',(0.134343829836486,-0.03677094505856,
0.0153122325183177));
#40031=CARTESIAN_POINT('Ctrl Pts',(0.103577487134497,0.0931457228401511,
0.0232647366334205));
#40032=CARTESIAN_POINT('Ctrl Pts',(-0.022319455813322,0.137480661654608,
0.0312172407485234));
#40033=CARTESIAN_POINT('Ctrl Pts',(-0.107013184840641,0.0716760847082379,
0.0376078990285884));
#40034=CARTESIAN_POINT('Ctrl Pts',(-0.117673522927843,0.0162276125558733,
0.0413477226036194));
#40035=CARTESIAN_POINT('Ctrl Pts',(-0.117605093279175,5.6374090473453E-5,
0.042436711473616));
#40036=CARTESIAN_POINT('Origin',(0.,0.,0.));
#40037=CARTESIAN_POINT('Ctrl Pts',(-0.0510216505388437,0.106149619882937,
-0.0164977839420935));
#40038=CARTESIAN_POINT('Ctrl Pts',(-0.0863815445949669,0.0891536084077042,
-0.0138469492370593));
#40039=CARTESIAN_POINT('Ctrl Pts',(-0.138162556478479,0.0173380738482791,
-0.00854527982699074));
#40040=CARTESIAN_POINT('Ctrl Pts',(-0.0892152289856901,-0.107087400898305,
-0.000592775711887911));
#40041=CARTESIAN_POINT('Ctrl Pts',(0.0417759011768067,-0.132831332515275,
0.00735972840321487));
#40042=CARTESIAN_POINT('Ctrl Pts',(0.134343829836486,-0.03677094505856,
0.0153122325183177));
#40043=CARTESIAN_POINT('Ctrl Pts',(0.103577487134497,0.0931457228401511,
0.0232647366334205));
#40044=CARTESIAN_POINT('Ctrl Pts',(-0.022319455813322,0.137480661654608,
0.0312172407485234));
#40045=CARTESIAN_POINT('Ctrl Pts',(-0.127711920735776,0.0555937658099327,
0.0391697448636261));
#40046=CARTESIAN_POINT('Ctrl Pts',(-0.115832853027164,-0.0773572203301017,
0.047122248978729));
#40047=CARTESIAN_POINT('Ctrl Pts',(0.00241643506700816,-0.139265216174241,
0.0550747530938317));
#40048=CARTESIAN_POINT('Ctrl Pts',(0.118445458723555,-0.0732914200146354,
0.0630272572089346));
#40049=CARTESIAN_POINT('Ctrl Pts',(0.125708256673902,0.0599868231457294,
0.0709797613240373));
#40050=CARTESIAN_POINT('Ctrl Pts',(0.0175344664057042,0.138178956948752,
0.0789322654391402));
#40051=CARTESIAN_POINT('Ctrl Pts',(-0.106740805893122,0.0894837054538652,
0.0868847695542431));
#40052=CARTESIAN_POINT('Ctrl Pts',(-0.132997503503664,-0.0413835288220579,
0.0948372736693457));
#40053=CARTESIAN_POINT('Ctrl Pts',(-0.0371242974264225,-0.134248668971966,
0.102789777784449));
#40054=CARTESIAN_POINT('Ctrl Pts',(0.0928396337021713,-0.10383510521762,
0.110742281899551));
#40055=CARTESIAN_POINT('Ctrl Pts',(0.137550169005636,0.0219289054269618,
0.118694786014654));
#40056=CARTESIAN_POINT('Ctrl Pts',(0.0559501922162531,0.127555870431356,
0.126647290129757));
#40057=CARTESIAN_POINT('Ctrl Pts',(-0.0770281035821754,0.116049974518826,
0.13459979424486));
#40058=CARTESIAN_POINT('Ctrl Pts',(-0.13927251071013,-0.00202308703008076,
0.142552298359963));
#40059=CARTESIAN_POINT('Ctrl Pts',(-0.0736248085349355,-0.118238371369349,
0.150504802475065));
#40060=CARTESIAN_POINT('Ctrl Pts',(0.0596315829014974,-0.125876921640408,
0.158457306590168));
#40061=CARTESIAN_POINT('Ctrl Pts',(0.138129079193178,-0.0179243554725553,
0.166409810705271));
#40062=CARTESIAN_POINT('Ctrl Pts',(0.0897844651888838,0.106487909275724,
0.174362314820374));
#40063=CARTESIAN_POINT('Ctrl Pts',(-0.0410080379701501,0.133113732800722,
0.182314818935477));
#40064=CARTESIAN_POINT('Ctrl Pts',(-0.134143401206605,0.0375029724551737,
0.190267323050579));
#40065=CARTESIAN_POINT('Ctrl Pts',(-0.104096649768354,-0.0925462723956308,
0.198219827165683));
#40066=CARTESIAN_POINT('Ctrl Pts',(0.0215406810767683,-0.137611496939632,
0.206172331280785));
#40067=CARTESIAN_POINT('Ctrl Pts',(0.127397488829925,-0.056309900280862,
0.214124835395888));
#40068=CARTESIAN_POINT('Ctrl Pts',(0.116266864218555,0.0767003345124148,
0.222077339510991));
#40069=CARTESIAN_POINT('Ctrl Pts',(-0.0016300870944122,0.139277664563073,
0.230029843626094));
#40070=CARTESIAN_POINT('Ctrl Pts',(-0.1180301509465,0.0739581536911037,
0.237982347741196));
#40071=CARTESIAN_POINT('Ctrl Pts',(-0.126044685167542,-0.0592761534753867,
0.245934851856299));
#40072=CARTESIAN_POINT('Ctrl Pts',(-0.0183140487741412,-0.138077951344142,
0.253887355971402));
#40073=CARTESIAN_POINT('Ctrl Pts',(0.106234136865658,-0.0900845891054932,
0.261839860086505));
#40074=CARTESIAN_POINT('Ctrl Pts',(0.133228916899009,0.040632262203075,
0.269792364201608));
#40075=CARTESIAN_POINT('Ctrl Pts',(0.0378813411502606,0.134037043471229,
0.27774486831671));
#40076=CARTESIAN_POINT('Ctrl Pts',(-0.092252170148986,0.104357376993109,
0.285697372431813));
#40077=CARTESIAN_POINT('Ctrl Pts',(-0.137671731315388,-0.021152291274371,
0.293649876546916));
#40078=CARTESIAN_POINT('Ctrl Pts',(-0.0566691588697243,-0.127238089669758,
0.301602380662019));
#40079=CARTESIAN_POINT('Ctrl Pts',(0.0763719541489209,-0.116482829853556,
0.309554884777122));
#40080=CARTESIAN_POINT('Ctrl Pts',(0.139281709756163,0.00123707506708643,
0.317507388892225));
#40081=CARTESIAN_POINT('Ctrl Pts',(0.0742909098282569,0.117820990265484,
0.325459893007327));
#40082=CARTESIAN_POINT('Ctrl Pts',(-0.0589202520252667,0.1262114453589,
0.33341239712243));
#40083=CARTESIAN_POINT('Ctrl Pts',(-0.13802572406761,0.0187035960922139,
0.341364901237533));
#40084=CARTESIAN_POINT('Ctrl Pts',(-0.0903839958430062,-0.105979518461414,
0.349317405352636));
#40085=CARTESIAN_POINT('Ctrl Pts',(0.0402561631274929,-0.133343040355529,
0.357269909467738));
#40086=CARTESIAN_POINT('Ctrl Pts',(0.133929618074243,-0.0382594079720193,
0.365222413582842));
#40087=CARTESIAN_POINT('Ctrl Pts',(0.104617274119081,0.0919573329132998,
0.373174917697944));
#40088=CARTESIAN_POINT('Ctrl Pts',(-0.020763734615072,0.137730870367254,
0.381127421813047));
#40089=CARTESIAN_POINT('Ctrl Pts',(-0.127077674436729,0.0570279646339328,
0.38907992592815));
#40090=CARTESIAN_POINT('Ctrl Pts',(-0.116697873675526,-0.0760429626350431,
0.397032430043252));
#40091=CARTESIAN_POINT('Ctrl Pts',(0.000844063931402275,-0.139284651766041,
0.404984934158356));
#40092=CARTESIAN_POINT('Ctrl Pts',(0.117610871049501,-0.0746230633995127,
0.412937438273457));
#40093=CARTESIAN_POINT('Ctrl Pts',(0.126377239427685,0.0585638604483229,
0.420889942388562));
#40094=CARTESIAN_POINT('Ctrl Pts',(0.0190929207373193,0.137972437690235,
0.428842446503664));
#40095=CARTESIAN_POINT('Ctrl Pts',(-0.105723916050958,0.0906826070998613,
0.436794950618767));
#40096=CARTESIAN_POINT('Ctrl Pts',(-0.133456368516637,-0.0398795994144927,
0.44474745473387));
#40097=CARTESIAN_POINT('Ctrl Pts',(-0.038636663810782,-0.133821400192823,
0.452699958848972));
#40098=CARTESIAN_POINT('Ctrl Pts',(0.0916608011058181,-0.104875817685159,
0.460652462964076));
#40099=CARTESIAN_POINT('Ctrl Pts',(0.137790741908166,0.0203740232160909,
0.468604967079177));
#40100=CARTESIAN_POINT('Ctrl Pts',(0.0573828398023632,0.126918127906013,
0.476557471194281));
#40101=CARTESIAN_POINT('Ctrl Pts',(-0.0757067578384881,0.11690841395886,
0.484509975309383));
#40102=CARTESIAN_POINT('Ctrl Pts',(-0.139299045817393,-0.000444250914572553,
0.492462479424487));
#40103=CARTESIAN_POINT('Ctrl Pts',(-0.0749307309976486,-0.117412744486246,
0.500414983539588));
#40104=CARTESIAN_POINT('Ctrl Pts',(0.0581614397283287,-0.126517333775439,
0.508367487654693));
#40105=CARTESIAN_POINT('Ctrl Pts',(0.138005962114904,-0.01953005209576,
0.516319991769794));
#40106=CARTESIAN_POINT('Ctrl Pts',(0.0908022345067483,0.105567300931769,
0.524272495884898));
#40107=CARTESIAN_POINT('Ctrl Pts',(0.00421962447768953,0.124065836989857,
0.529574165294966));
#40108=CARTESIAN_POINT('Ctrl Pts',(-0.0334019664626881,0.11293918390632,
0.532225));
#40109=CARTESIAN_POINT('Ctrl Pts',(-0.0551480035117362,0.114734422509853,
-0.0109985226280624));
#40110=CARTESIAN_POINT('Ctrl Pts',(-0.0933676130497917,0.096363866272985,
-0.0083476879230281));
#40111=CARTESIAN_POINT('Ctrl Pts',(-0.149336390912421,0.0187402827500406,
-0.00304601851295955));
#40112=CARTESIAN_POINT('Ctrl Pts',(-0.0964304703874203,-0.115748046141832,
0.00490648560214325));
#40113=CARTESIAN_POINT('Ctrl Pts',(0.0451545083405425,-0.143574006615959,
0.0128589897172461));
#40114=CARTESIAN_POINT('Ctrl Pts',(0.145208826475777,-0.0397447786538297,
0.0208114938323489));
#40115=CARTESIAN_POINT('Ctrl Pts',(0.1119542696856,0.100678841159424,0.0287639979474517));
#40116=CARTESIAN_POINT('Ctrl Pts',(-0.0241245317345429,0.148599348152253,
0.0367165020625545));
#40117=CARTESIAN_POINT('Ctrl Pts',(-0.138040564718016,0.060089886543023,
0.0446690061776573));
#40118=CARTESIAN_POINT('Ctrl Pts',(-0.125200782766784,-0.0836134506306251,
0.0526215102927601));
#40119=CARTESIAN_POINT('Ctrl Pts',(0.00261186316306541,-0.150528227713698,
0.0605740144078629));
#40120=CARTESIAN_POINT('Ctrl Pts',(0.128024681770397,-0.0792188305486153,
0.0685265185229658));
#40121=CARTESIAN_POINT('Ctrl Pts',(0.135874855228935,0.0648382304092657,
0.0764790226380685));
#40122=CARTESIAN_POINT('Ctrl Pts',(0.0189525584669602,0.149354117763329,
0.0844315267531714));
#40123=CARTESIAN_POINT('Ctrl Pts',(-0.115373420421943,0.096720659768857,
0.0923840308682741));
#40124=CARTESIAN_POINT('Ctrl Pts',(-0.143753616608078,-0.0447304030485916,
0.100336534983377));
#40125=CARTESIAN_POINT('Ctrl Pts',(-0.0401267082350556,-0.145105969519263,
0.10828903909848));
#40126=CARTESIAN_POINT('Ctrl Pts',(0.100347997200478,-0.112232722514991,
0.116241543213583));
#40127=CARTESIAN_POINT('Ctrl Pts',(0.148674476878943,0.0237023957618521,
0.124194047328685));
#40128=CARTESIAN_POINT('Ctrl Pts',(0.0604751387741805,0.137871893915615,
0.132146551443788));
#40129=CARTESIAN_POINT('Ctrl Pts',(-0.0832577167141655,0.125435463861147,
0.140099055558891));
#40130=CARTESIAN_POINT('Ctrl Pts',(-0.150536112191887,-0.00218670328107987,
0.148051559673994));
#40131=CARTESIAN_POINT('Ctrl Pts',(-0.0795791817151125,-0.127800846319831,
0.156004063789097));
#40132=CARTESIAN_POINT('Ctrl Pts',(0.0644542602705204,-0.136057160898527,
0.163956567904199));
#40133=CARTESIAN_POINT('Ctrl Pts',(0.149300206166772,-0.0193739796362248,
0.171909072019302));
#40134=CARTESIAN_POINT('Ctrl Pts',(0.0970457433117808,0.115100070904688,
0.179861576134405));
#40135=CARTESIAN_POINT('Ctrl Pts',(-0.0443245445434091,0.143879245897109,
0.187814080249508));
#40136=CARTESIAN_POINT('Ctrl Pts',(-0.144992188270862,0.0405360084359473,
0.195766584364611));
#40137=CARTESIAN_POINT('Ctrl Pts',(-0.11251541936329,-0.100030910430598,
0.203719088479714));
#40138=CARTESIAN_POINT('Ctrl Pts',(0.023282773942454,-0.148740764681937,
0.211671592594816));
#40139=CARTESIAN_POINT('Ctrl Pts',(0.13770070327361,-0.0608639380662604,
0.219624096709919));
#40140=CARTESIAN_POINT('Ctrl Pts',(0.125669894417509,0.0829034394687354,
0.227576600825022));
#40141=CARTESIAN_POINT('Ctrl Pts',(-0.00176191965288545,0.150541682860363,
0.235529104940125));
#40142=CARTESIAN_POINT('Ctrl Pts',(-0.127575786164206,0.0799394860104231,
0.243481609055227));
#40143=CARTESIAN_POINT('Ctrl Pts',(-0.136238492225245,-0.0640700856498972,
0.25143411317033));
#40144=CARTESIAN_POINT('Ctrl Pts',(-0.0197951892077968,-0.149244943376008,
0.259386617285433));
#40145=CARTESIAN_POINT('Ctrl Pts',(0.114825774765427,-0.0973701396147685,
0.267339121400536));
#40146=CARTESIAN_POINT('Ctrl Pts',(0.144003745457388,0.0439183780806738,
0.275291625515639));
#40147=CARTESIAN_POINT('Ctrl Pts',(0.0409449775285778,0.144877228901612,
0.283244129630741));
#40148=CARTESIAN_POINT('Ctrl Pts',(-0.0997130227974173,0.112797232784741,
0.291196633745845));
#40149=CARTESIAN_POINT('Ctrl Pts',(-0.148805870485663,-0.0228629732899794,
0.299149137860947));
#40150=CARTESIAN_POINT('Ctrl Pts',(-0.0612522515314454,-0.137528412778265,
0.30710164197605));
#40151=CARTESIAN_POINT('Ctrl Pts',(0.0825485014914671,-0.125903326175825,
0.315054146091153));
#40152=CARTESIAN_POINT('Ctrl Pts',(0.150546055206619,0.00133712295512629,
0.323006650206255));
#40153=CARTESIAN_POINT('Ctrl Pts',(0.0802991536500716,0.12734970970746,
0.330959154321359));
#40154=CARTESIAN_POINT('Ctrl Pts',(-0.0636854008305359,0.136418739071857,
0.338911658436461));
#40155=CARTESIAN_POINT('Ctrl Pts',(-0.149188492242044,0.0202162409895048,
0.346864162551565));
#40156=CARTESIAN_POINT('Ctrl Pts',(-0.0976937607371238,-0.114550564212591,
0.354816666666667));
#40157=CARTESIAN_POINT('Ctrl Pts',(0.0435118621620017,-0.144127098596976,
0.36276917078177));
#40158=CARTESIAN_POINT('Ctrl Pts',(0.144761115524102,-0.041353620334011,
0.370721674896872));
#40159=CARTESIAN_POINT('Ctrl Pts',(0.113078148973544,0.0993943407332879,
0.378674179011976));
#40160=CARTESIAN_POINT('Ctrl Pts',(-0.0224429922861266,0.148869792381672,
0.386626683127078));
#40161=CARTESIAN_POINT('Ctrl Pts',(-0.137355024035624,0.0616400755499871,
0.394579187242181));
#40162=CARTESIAN_POINT('Ctrl Pts',(-0.126135761569897,-0.0821929029373033,
0.402531691357283));
#40163=CARTESIAN_POINT('Ctrl Pts',(0.000912327221120078,-0.150549235150219,
0.410484195472387));
#40164=CARTESIAN_POINT('Ctrl Pts',(0.127122597194663,-0.0806581699915775,
0.418436699587489));
#40165=CARTESIAN_POINT('Ctrl Pts',(0.136597941661171,0.0633001862455649,
0.426389203702593));
#40166=CARTESIAN_POINT('Ctrl Pts',(0.0206370520896696,0.149130896352934,
0.434341707817695));
#40167=CARTESIAN_POINT('Ctrl Pts',(-0.114274290072485,0.0980165220446819,
0.442294211932798));
#40168=CARTESIAN_POINT('Ctrl Pts',(-0.144249592121994,-0.0431048440285699,
0.450246716047901));
#40169=CARTESIAN_POINT('Ctrl Pts',(-0.0417613865685641,-0.144644145570336,
0.458199220163003));
#40170=CARTESIAN_POINT('Ctrl Pts',(0.0990738270496334,-0.113357602133906,
0.466151724278107));
#40171=CARTESIAN_POINT('Ctrl Pts',(0.148934506006449,0.0220217631535408,
0.474104228393209));
#40172=CARTESIAN_POINT('Ctrl Pts',(0.0620236510875902,0.137182574251203,
0.482056732508312));
#40173=CARTESIAN_POINT('Ctrl Pts',(-0.0818295077294796,0.126363329203676,
0.490009236623415));
#40174=CARTESIAN_POINT('Ctrl Pts',(-0.150564793313981,-0.000480179506898605,
0.497961740738518));
#40175=CARTESIAN_POINT('Ctrl Pts',(-0.0809907200679325,-0.126908447234973,
0.50591424485362));
#40176=CARTESIAN_POINT('Ctrl Pts',(0.0628652199313619,-0.136749366076106,
0.513866748968723));
#40177=CARTESIAN_POINT('Ctrl Pts',(0.149167132050327,-0.0211095362495466,
0.521819253083827));
#40178=CARTESIAN_POINT('Ctrl Pts',(0.0981458242641405,0.114105008776176,
0.529771757198928));
#40179=CARTESIAN_POINT('Ctrl Pts',(0.00456088470396912,0.134099605593792,
0.535073426608997));
#40180=CARTESIAN_POINT('Ctrl Pts',(-0.0361033354336669,0.122073089461044,
0.537724261314032));
#40181=CARTESIAN_POINT('Ctrl Pts',(-0.0592743564846287,0.123319225136769,
-0.00549926131403118));
#40182=CARTESIAN_POINT('Ctrl Pts',(-0.100353681504617,0.103574124138266,
-0.00284842660899691));
#40183=CARTESIAN_POINT('Ctrl Pts',(-0.160510225346362,0.0201424916518021,
0.00245324280107164));
#40184=CARTESIAN_POINT('Ctrl Pts',(-0.103645711789151,-0.124408691385358,
0.0104057469161744));
#40185=CARTESIAN_POINT('Ctrl Pts',(0.0485331155042784,-0.154316680716642,
0.0183582510312773));
#40186=CARTESIAN_POINT('Ctrl Pts',(0.156073823115068,-0.0427186122490994,
0.02631075514638));
#40187=CARTESIAN_POINT('Ctrl Pts',(0.120331052236703,0.108211959478697,
0.0342632592614829));
#40188=CARTESIAN_POINT('Ctrl Pts',(-0.0259296076557639,0.159718034649898,
0.0422157633765857));
#40189=CARTESIAN_POINT('Ctrl Pts',(-0.148369208700255,0.0645860072761131,
0.0501682674916885));
#40190=CARTESIAN_POINT('Ctrl Pts',(-0.134568712506405,-0.0898696809311483,
0.0581207716067913));
#40191=CARTESIAN_POINT('Ctrl Pts',(0.00280729125912282,-0.161791239253156,
0.0660732757218941));
#40192=CARTESIAN_POINT('Ctrl Pts',(0.137603904817239,-0.0851462410825952,
0.074025779836997));
#40193=CARTESIAN_POINT('Ctrl Pts',(0.146041453783967,0.0696896376728019,
0.0819782839520996));
#40194=CARTESIAN_POINT('Ctrl Pts',(0.0203706505282163,0.160529278577907,
0.0899307880672026));
#40195=CARTESIAN_POINT('Ctrl Pts',(-0.124006034950765,0.103957614083849,
0.0978832921823053));
#40196=CARTESIAN_POINT('Ctrl Pts',(-0.154509729712493,-0.0480772772751253,
0.105835796297408));
#40197=CARTESIAN_POINT('Ctrl Pts',(-0.0431291190436888,-0.155963270066561,
0.113788300412511));
#40198=CARTESIAN_POINT('Ctrl Pts',(0.107856360698785,-0.120630339812362,
0.121740804527614));
#40199=CARTESIAN_POINT('Ctrl Pts',(0.159798784752249,0.0254758860967424,
0.129693308642717));
#40200=CARTESIAN_POINT('Ctrl Pts',(0.065000085332108,0.148187917399874,
0.137645812757819));
#40201=CARTESIAN_POINT('Ctrl Pts',(-0.0894873298461556,0.134820953203468,
0.145598316872922));
#40202=CARTESIAN_POINT('Ctrl Pts',(-0.161799713673645,-0.00235031953207901,
0.153550820988025));
#40203=CARTESIAN_POINT('Ctrl Pts',(-0.0855335548952896,-0.137363321270313,
0.161503325103128));
#40204=CARTESIAN_POINT('Ctrl Pts',(0.0692769376395434,-0.146237400156646,
0.169455829218231));
#40205=CARTESIAN_POINT('Ctrl Pts',(0.160471333140366,-0.0208236037998943,
0.177408333333334));
#40206=CARTESIAN_POINT('Ctrl Pts',(0.104307021434678,0.123712232533651,
0.185360837448436));
#40207=CARTESIAN_POINT('Ctrl Pts',(-0.0476410511166683,0.154644758993495,
0.193313341563539));
#40208=CARTESIAN_POINT('Ctrl Pts',(-0.155840975335119,0.043569044416721,
0.201265845678642));
#40209=CARTESIAN_POINT('Ctrl Pts',(-0.120934188958227,-0.107515548465566,
0.209218349793745));
#40210=CARTESIAN_POINT('Ctrl Pts',(0.0250248668081396,-0.159870032424242,
0.217170853908847));
#40211=CARTESIAN_POINT('Ctrl Pts',(0.148003917717295,-0.0654179758516589,
0.22512335802395));
#40212=CARTESIAN_POINT('Ctrl Pts',(0.135072924616463,0.0891065444250562,
0.233075862139053));
#40213=CARTESIAN_POINT('Ctrl Pts',(-0.0018937522113587,0.161805701157652,
0.241028366254156));
#40214=CARTESIAN_POINT('Ctrl Pts',(-0.137121421381912,0.0859208183297427,
0.248980870369259));
#40215=CARTESIAN_POINT('Ctrl Pts',(-0.146432299282947,-0.0688640178244077,
0.256933374484361));
#40216=CARTESIAN_POINT('Ctrl Pts',(-0.0212763296414524,-0.160411935407873,
0.264885878599465));
#40217=CARTESIAN_POINT('Ctrl Pts',(0.123417412665197,-0.104655690124044,
0.272838382714567));
#40218=CARTESIAN_POINT('Ctrl Pts',(0.154778574015767,0.0472044939582724,
0.28079088682967));
#40219=CARTESIAN_POINT('Ctrl Pts',(0.0440086139068953,0.155717414331996,
0.288743390944773));
#40220=CARTESIAN_POINT('Ctrl Pts',(-0.107173875445849,0.121237088576372,
0.296695895059875));
#40221=CARTESIAN_POINT('Ctrl Pts',(-0.159940009655938,-0.0245736553055878,
0.304648399174979));
#40222=CARTESIAN_POINT('Ctrl Pts',(-0.0658353441931666,-0.147818735886772,
0.312600903290081));
#40223=CARTESIAN_POINT('Ctrl Pts',(0.0887250488340134,-0.135323822498093,
0.320553407405184));
#40224=CARTESIAN_POINT('Ctrl Pts',(0.161810400657075,0.00143717084316612,
0.328505911520287));
#40225=CARTESIAN_POINT('Ctrl Pts',(0.0863073974718863,0.136878429149436,
0.33645841563539));
#40226=CARTESIAN_POINT('Ctrl Pts',(-0.0684505496358049,0.146626032784815,
0.344410919750492));
#40227=CARTESIAN_POINT('Ctrl Pts',(-0.160351260416479,0.0217288858867957,
0.352363423865596));
#40228=CARTESIAN_POINT('Ctrl Pts',(-0.105003525631241,-0.123121609963769,
0.360315927980698));
#40229=CARTESIAN_POINT('Ctrl Pts',(0.0467675611965104,-0.154911156838423,
0.368268432095801));
#40230=CARTESIAN_POINT('Ctrl Pts',(0.155592612973961,-0.0444478326960028,
0.376220936210903));
#40231=CARTESIAN_POINT('Ctrl Pts',(0.121539023828006,0.106831348553276,
0.384173440326007));
#40232=CARTESIAN_POINT('Ctrl Pts',(-0.0241222499571812,0.160008714396091,
0.392125944441109));
#40233=CARTESIAN_POINT('Ctrl Pts',(-0.147632373634519,0.0662521864660413,
0.400078448556213));
#40234=CARTESIAN_POINT('Ctrl Pts',(-0.135573649464267,-0.0883428432395635,
0.408030952671315));
#40235=CARTESIAN_POINT('Ctrl Pts',(0.00098059051083778,-0.161813818534397,
0.415983456786418));
#40236=CARTESIAN_POINT('Ctrl Pts',(0.136634323339825,-0.0866932765836425,
0.423935960901521));
#40237=CARTESIAN_POINT('Ctrl Pts',(0.146818643894656,0.068036512042807,
0.431888465016623));
#40238=CARTESIAN_POINT('Ctrl Pts',(0.0221811834420201,0.160289355015634,
0.439840969131727));
#40239=CARTESIAN_POINT('Ctrl Pts',(-0.122824664094011,0.105350436989503,
0.447793473246828));
#40240=CARTESIAN_POINT('Ctrl Pts',(-0.155042815727352,-0.0463300886426471,
0.455745977361933));
#40241=CARTESIAN_POINT('Ctrl Pts',(-0.0448861093263465,-0.155466890947849,
0.463698481477034));
#40242=CARTESIAN_POINT('Ctrl Pts',(0.106486852993449,-0.121839386582653,
0.471650985592139));
#40243=CARTESIAN_POINT('Ctrl Pts',(0.160078270104732,0.0236695030909907,
0.47960348970724));
#40244=CARTESIAN_POINT('Ctrl Pts',(0.0666644623728171,0.147447020596393,
0.487555993822343));
#40245=CARTESIAN_POINT('Ctrl Pts',(-0.087952257620471,0.135818244448492,
0.495508497937446));
#40246=CARTESIAN_POINT('Ctrl Pts',(-0.161830540810569,-0.000516108099224624,
0.503461002052549));
#40247=CARTESIAN_POINT('Ctrl Pts',(-0.0870507091382164,-0.136404149983702,
0.511413506167652));
#40248=CARTESIAN_POINT('Ctrl Pts',(0.0675690001343951,-0.146981398376774,
0.519366010282755));
#40249=CARTESIAN_POINT('Ctrl Pts',(0.16032830198575,-0.0226890204033332,
0.527318514397857));
#40250=CARTESIAN_POINT('Ctrl Pts',(0.105489414021532,0.122642716620584,
0.53527101851296));
#40251=CARTESIAN_POINT('Ctrl Pts',(0.00490214493024879,0.144133374197726,
0.540572687923028));
#40252=CARTESIAN_POINT('Ctrl Pts',(-0.0388047044046456,0.131206995015769,
0.543223522628063));
#40253=CARTESIAN_POINT('Ctrl Pts',(-0.0634007094575211,0.131904027763685,
0.));
#40254=CARTESIAN_POINT('Ctrl Pts',(-0.107339749959441,0.110784382003547,
0.00265083470503427));
#40255=CARTESIAN_POINT('Ctrl Pts',(-0.171684059780304,0.0215447005535634,
0.00795250411510281));
#40256=CARTESIAN_POINT('Ctrl Pts',(-0.110860953190881,-0.133069336628884,
0.0159050082302056));
#40257=CARTESIAN_POINT('Ctrl Pts',(0.0519117226680141,-0.165059354817326,
0.0238575123453085));
#40258=CARTESIAN_POINT('Ctrl Pts',(0.166938819754359,-0.045692445844369,
0.0318100164604112));
#40259=CARTESIAN_POINT('Ctrl Pts',(0.128707834787806,0.11574507779797,0.0397625205755141));
#40260=CARTESIAN_POINT('Ctrl Pts',(-0.0277346835769849,0.170836721147544,
0.0477150246906169));
#40261=CARTESIAN_POINT('Ctrl Pts',(-0.158697852682494,0.0690821280092034,
0.0556675288057197));
#40262=CARTESIAN_POINT('Ctrl Pts',(-0.143936642246025,-0.0961259112316717,
0.0636200329208225));
#40263=CARTESIAN_POINT('Ctrl Pts',(0.00300271935518024,-0.173054250792614,
0.0715725370359253));
#40264=CARTESIAN_POINT('Ctrl Pts',(0.14718312786408,-0.0910736516165751,
0.0795250411510281));
#40265=CARTESIAN_POINT('Ctrl Pts',(0.156208052339,0.0745410449363381,0.0874775452661308));
#40266=CARTESIAN_POINT('Ctrl Pts',(0.0217887425894723,0.171704439392484,
0.0954300493812338));
#40267=CARTESIAN_POINT('Ctrl Pts',(-0.132638649479586,0.11119456839884,
0.103382553496337));
#40268=CARTESIAN_POINT('Ctrl Pts',(-0.165265842816907,-0.0514241515016591,
0.111335057611439));
#40269=CARTESIAN_POINT('Ctrl Pts',(-0.0461315298523219,-0.166820570613858,
0.119287561726542));
#40270=CARTESIAN_POINT('Ctrl Pts',(0.115364724197092,-0.129027957109734,
0.127240065841645));
#40271=CARTESIAN_POINT('Ctrl Pts',(0.170923092625556,0.0272493764316328,
0.135192569956748));
#40272=CARTESIAN_POINT('Ctrl Pts',(0.0695250318900354,0.158503940884133,
0.143145074071851));
#40273=CARTESIAN_POINT('Ctrl Pts',(-0.0957169429781459,0.144206442545789,
0.151097578186953));
#40274=CARTESIAN_POINT('Ctrl Pts',(-0.173063315155402,-0.00251393578307793,
0.159050082302056));
#40275=CARTESIAN_POINT('Ctrl Pts',(-0.0914879280754666,-0.146925796220795,
0.167002586417159));
#40276=CARTESIAN_POINT('Ctrl Pts',(0.0740996150085664,-0.156417639414764,
0.174955090532262));
#40277=CARTESIAN_POINT('Ctrl Pts',(0.171642460113959,-0.0222732279635641,
0.182907594647365));
#40278=CARTESIAN_POINT('Ctrl Pts',(0.111568299557575,0.132324394162615,
0.190860098762467));
#40279=CARTESIAN_POINT('Ctrl Pts',(-0.0509575576899273,0.165410272089882,
0.19881260287757));
#40280=CARTESIAN_POINT('Ctrl Pts',(-0.166689762399376,0.0466020803974948,
0.206765106992673));
#40281=CARTESIAN_POINT('Ctrl Pts',(-0.129352958553163,-0.115000186500534,
0.214717611107776));
#40282=CARTESIAN_POINT('Ctrl Pts',(0.0267669596738252,-0.170999300166548,
0.222670115222879));
#40283=CARTESIAN_POINT('Ctrl Pts',(0.15830713216098,-0.0699720136370574,
0.230622619337982));
#40284=CARTESIAN_POINT('Ctrl Pts',(0.144475954815417,0.0953096493813769,
0.238575123453084));
#40285=CARTESIAN_POINT('Ctrl Pts',(-0.00202558476983171,0.173069719454941,
0.246527627568187));
#40286=CARTESIAN_POINT('Ctrl Pts',(-0.146667056599619,0.091902150649062,
0.25448013168329));
#40287=CARTESIAN_POINT('Ctrl Pts',(-0.156626106340649,-0.073657949998918,
0.262432635798393));
#40288=CARTESIAN_POINT('Ctrl Pts',(-0.0227574700751082,-0.171578927439738,
0.270385139913495));
#40289=CARTESIAN_POINT('Ctrl Pts',(0.132009050564966,-0.111941240633319,
0.278337644028599));
#40290=CARTESIAN_POINT('Ctrl Pts',(0.165553402574146,0.0504906098358712,
0.286290148143701));
#40291=CARTESIAN_POINT('Ctrl Pts',(0.0470722502852127,0.16655759976238,
0.294242652258804));
#40292=CARTESIAN_POINT('Ctrl Pts',(-0.11463472809428,0.129676944368004,
0.302195156373907));
#40293=CARTESIAN_POINT('Ctrl Pts',(-0.171074148826212,-0.0262843373211962,
0.31014766048901));
#40294=CARTESIAN_POINT('Ctrl Pts',(-0.0704184368548879,-0.158109058995279,
0.318100164604112));
#40295=CARTESIAN_POINT('Ctrl Pts',(0.0949015961765597,-0.144744318820362,
0.326052668719215));
#40296=CARTESIAN_POINT('Ctrl Pts',(0.173074746107531,0.00153721873120606,
0.334005172834318));
#40297=CARTESIAN_POINT('Ctrl Pts',(0.0923156412937011,0.146407148591411,
0.341957676949421));
#40298=CARTESIAN_POINT('Ctrl Pts',(-0.0732156984410742,0.156833326497772,
0.349910181064524));
#40299=CARTESIAN_POINT('Ctrl Pts',(-0.171514028590913,0.0232415307840867,
0.357862685179626));
#40300=CARTESIAN_POINT('Ctrl Pts',(-0.112313290525359,-0.131692655714946,
0.365815189294729));
#40301=CARTESIAN_POINT('Ctrl Pts',(0.0500232602310192,-0.165695215079871,
0.373767693409832));
#40302=CARTESIAN_POINT('Ctrl Pts',(0.16642411042382,-0.0475420450579947,
0.381720197524935));
#40303=CARTESIAN_POINT('Ctrl Pts',(0.129999898682469,0.114268356373264,
0.389672701640038));
#40304=CARTESIAN_POINT('Ctrl Pts',(-0.0258015076282358,0.171147636410509,
0.39762520575514));
#40305=CARTESIAN_POINT('Ctrl Pts',(-0.157909723233413,0.0708642973820958,
0.405577709870244));
#40306=CARTESIAN_POINT('Ctrl Pts',(-0.145011537358637,-0.0944927835418238,
0.413530213985346));
#40307=CARTESIAN_POINT('Ctrl Pts',(0.00104885380055552,-0.173078401918574,
0.421482718100449));
#40308=CARTESIAN_POINT('Ctrl Pts',(0.146146049484986,-0.0927283831757074,
0.429435222215551));
#40309=CARTESIAN_POINT('Ctrl Pts',(0.157039346128141,0.0727728378400491,
0.437387726330655));
#40310=CARTESIAN_POINT('Ctrl Pts',(0.0237253147943705,0.171447813678334,
0.445340230445757));
#40311=CARTESIAN_POINT('Ctrl Pts',(-0.131375038115538,0.112684351934323,
0.45329273456086));
#40312=CARTESIAN_POINT('Ctrl Pts',(-0.16583603933271,-0.0495553332567244,
0.461245238675963));
#40313=CARTESIAN_POINT('Ctrl Pts',(-0.0480108320841284,-0.166289636325362,
0.469197742791066));
#40314=CARTESIAN_POINT('Ctrl Pts',(0.113899878937264,-0.130321171031401,
0.477150246906169));
#40315=CARTESIAN_POINT('Ctrl Pts',(0.171222034203015,0.0253172430284407,
0.485102751021271));
#40316=CARTESIAN_POINT('Ctrl Pts',(0.071305273658044,0.157711466941583,
0.493055255136374));
#40317=CARTESIAN_POINT('Ctrl Pts',(-0.0940750075114624,0.145273159693308,
0.501007759251477));
#40318=CARTESIAN_POINT('Ctrl Pts',(-0.173096288307157,-0.000552036691550711,
0.50896026336658));
#40319=CARTESIAN_POINT('Ctrl Pts',(-0.0931106982085004,-0.14589985273243,
0.516912767481683));
#40320=CARTESIAN_POINT('Ctrl Pts',(0.0722727803374284,-0.157213430677441,
0.524865271596785));
#40321=CARTESIAN_POINT('Ctrl Pts',(0.171489471921174,-0.0242685045571198,
0.532817775711888));
#40322=CARTESIAN_POINT('Ctrl Pts',(0.112833003778924,0.131180424464991,
0.540770279826991));
#40323=CARTESIAN_POINT('Ctrl Pts',(0.00524340515652838,0.154167142801661,
0.54607194923706));
#40324=CARTESIAN_POINT('Ctrl Pts',(-0.0415060733756244,0.140340900570494,
0.548722783942094));
#40325=CARTESIAN_POINT('Ctrl Pts',(-0.146267142220666,-0.000128791573925899,
0.458934495415709));
#40326=CARTESIAN_POINT('Ctrl Pts',(-0.146386413462202,-0.014310462982192,
0.459704743169127));
#40327=CARTESIAN_POINT('Ctrl Pts',(-0.144492166435918,-0.0284609503391585,
0.460474990922545));
#40328=CARTESIAN_POINT('Ctrl Pts',(-0.140455004588417,-0.04197110290299,
0.461245238675963));
#40329=CARTESIAN_POINT('Ctrl Pts',(-0.126560970249849,-0.0884667676129373,
0.463896073380997));
#40330=CARTESIAN_POINT('Ctrl Pts',(-0.0872859011669886,-0.12737820196915,
0.466546908086032));
#40331=CARTESIAN_POINT('Ctrl Pts',(-0.0406632481219932,-0.140839174931596,
0.469197742791066));
#40332=CARTESIAN_POINT('Ctrl Pts',(0.00595940492300207,-0.154300147894042,
0.4718485774961));
#40333=CARTESIAN_POINT('Ctrl Pts',(0.0599296419301325,-0.142310659462721,
0.474499412201135));
#40334=CARTESIAN_POINT('Ctrl Pts',(0.0964684529779897,-0.110376179570421,
0.477150246906169));
#40335=CARTESIAN_POINT('Ctrl Pts',(0.133007264025847,-0.0784416996781205,
0.479801081611203));
#40336=CARTESIAN_POINT('Ctrl Pts',(0.152114649114431,-0.0265622283248395,
0.482451916316237));
#40337=CARTESIAN_POINT('Ctrl Pts',(0.145015548234561,0.0214432113373248,
0.485102751021272));
#40338=CARTESIAN_POINT('Ctrl Pts',(0.137916447354691,0.0694486509994885,
0.487753585726306));
#40339=CARTESIAN_POINT('Ctrl Pts',(0.104610860506367,0.113580058970536,
0.49040442043134));
#40340=CARTESIAN_POINT('Ctrl Pts',(0.0603946868872881,0.133572711748014,
0.493055255136374));
#40341=CARTESIAN_POINT('Ctrl Pts',(0.0161785132682088,0.153565364525491,
0.495706089841409));
#40342=CARTESIAN_POINT('Ctrl Pts',(-0.0389482471216264,0.1494192621094,
0.498356924546443));
#40343=CARTESIAN_POINT('Ctrl Pts',(-0.0796818407824932,0.123042011503878,
0.501007759251477));
#40344=CARTESIAN_POINT('Ctrl Pts',(-0.0932156861533014,0.114278099486334,
0.501888506167652));
#40345=CARTESIAN_POINT('Ctrl Pts',(-0.105160643384876,0.103060050144818,
0.502769253083826));
#40346=CARTESIAN_POINT('Ctrl Pts',(-0.115072616245005,0.0902061753896192,
0.50365));
#40347=CARTESIAN_POINT('Ctrl Pts',(-0.0686153921261811,-0.0959615133978097,
-2.38524477946811E-18));
#40348=CARTESIAN_POINT('Ctrl Pts',(-0.0712073975642253,-0.0945517549303093,
-2.83889532725695E-18));
#40349=CARTESIAN_POINT('Ctrl Pts',(-0.0737377474651001,-0.0930410231931718,
5.14426139154652E-18));
#40350=CARTESIAN_POINT('Ctrl Pts',(-0.0761998018605363,-0.091430646244207,
6.50521303491303E-18));
#40351=CARTESIAN_POINT('Ctrl Pts',(-0.0821844297375259,-0.0875162295688071,
8.61254391956714E-18));
#40352=CARTESIAN_POINT('Ctrl Pts',(-0.0877662752922461,-0.0830147043174395,
8.93950144287772E-18));
#40353=CARTESIAN_POINT('Ctrl Pts',(-0.0929202787198591,-0.0780195924546499,
9.54097911787244E-18));
#40354=CARTESIAN_POINT('Ctrl Pts',(-0.0954786058604465,-0.0755401353824292,
9.83953861283751E-18));
#40355=CARTESIAN_POINT('Ctrl Pts',(-0.0979275180792717,-0.0729421130511386,
1.49939491249404E-17));
#40356=CARTESIAN_POINT('Ctrl Pts',(-0.100258897735172,-0.0702429236064683,
1.47451495458029E-17));
#40357=CARTESIAN_POINT('Ctrl Pts',(-0.104668940139426,-0.0651371314726185,
1.42745197659725E-17));
#40358=CARTESIAN_POINT('Ctrl Pts',(-0.108665118623842,-0.0596642636850333,
-1.289688799178E-17));
#40359=CARTESIAN_POINT('Ctrl Pts',(-0.112224391688578,-0.0538945629536488,
-2.42861286636753E-17));
#40360=CARTESIAN_POINT('Ctrl Pts',(-0.114007263482302,-0.0510044681210456,
-2.99911014422584E-17));
#40361=CARTESIAN_POINT('Ctrl Pts',(-0.115680198610802,-0.0480392113919056,
-9.85233076388881E-18));
#40362=CARTESIAN_POINT('Ctrl Pts',(-0.117233217251657,-0.0450208645520303,
-8.67361737988404E-18));
#40363=CARTESIAN_POINT('Ctrl Pts',(-0.121574823694362,-0.0365827983617143,
-5.37841570781424E-18));
#40364=CARTESIAN_POINT('Ctrl Pts',(-0.124997594823754,-0.027708690332575,
-9.37762199309504E-19));
#40365=CARTESIAN_POINT('Ctrl Pts',(-0.127437485841812,-0.018577962661637,
9.54097911787244E-18));
#40366=CARTESIAN_POINT('Ctrl Pts',(-0.12867484687016,-0.0139474252741679,
1.48551452162951E-17));
#40367=CARTESIAN_POINT('Ctrl Pts',(-0.129658851279119,-0.00925026145395888,
3.85592351303264E-18));
#40368=CARTESIAN_POINT('Ctrl Pts',(-0.13037677319566,-0.00450727571206391,
1.12757025938492E-17));
#40369=CARTESIAN_POINT('Ctrl Pts',(-0.130820878643177,-0.00157327166937493,
1.5865567080829E-17));
#40370=CARTESIAN_POINT('Ctrl Pts',(-0.131161668086746,0.00136911314303839,
-1.28026844144678E-17));
#40371=CARTESIAN_POINT('Ctrl Pts',(-0.131397381290232,0.00431340779322604,
-1.38777878078145E-17));
#40372=CARTESIAN_POINT('Ctrl Pts',(-0.131719489313798,0.0083368605168951,
-1.53469436465178E-17));
#40373=CARTESIAN_POINT('Ctrl Pts',(-0.131845540542961,0.0123645321806217,
2.00482317967995E-17));
#40374=CARTESIAN_POINT('Ctrl Pts',(-0.131770346471732,0.0163834363085182,
1.56125112837913E-17));
#40375=CARTESIAN_POINT('Ctrl Pts',(-0.131648667841181,0.0228868047604438,
8.25177748690449E-18));
#40376=CARTESIAN_POINT('Ctrl Pts',(-0.131000732502959,0.0293672129596454,
8.03096099599679E-18));
#40377=CARTESIAN_POINT('Ctrl Pts',(-0.129864039936534,0.0357832484813204,
1.04083408558608E-17));
#40378=CARTESIAN_POINT('Ctrl Pts',(-0.129251059617937,0.0392432020469336,
1.16903823743602E-17));
#40379=CARTESIAN_POINT('Ctrl Pts',(-0.128495732458156,0.0426844698916631,
9.6775998731851E-18));
#40380=CARTESIAN_POINT('Ctrl Pts',(-0.127602533865954,0.0461005734698996,
1.21430643318376E-17));
#40381=CARTESIAN_POINT('Ctrl Pts',(-0.126801717254801,0.0491633553806105,
1.43535300781251E-17));
#40382=CARTESIAN_POINT('Ctrl Pts',(-0.125892295195939,0.0521970927094408,
-2.04303423409802E-17));
#40383=CARTESIAN_POINT('Ctrl Pts',(-0.12487995022281,0.0551944839930744,
-1.90819582357449E-17));
#40384=CARTESIAN_POINT('Ctrl Pts',(-0.122213990144214,0.063087964688102,
-1.55310558352899E-17));
#40385=CARTESIAN_POINT('Ctrl Pts',(-0.118834573434494,0.0707355529753685,
-2.09602125306395E-19));
#40386=CARTESIAN_POINT('Ctrl Pts',(-0.114813287039476,0.0780547614149283,
-3.46944695195361E-18));
#40387=CARTESIAN_POINT('Ctrl Pts',(-0.112113271799503,0.0829691028445349,
-5.65820692756715E-18));
#40388=CARTESIAN_POINT('Ctrl Pts',(-0.109123295952561,0.0877354841888059,
1.59792597750096E-17));
#40389=CARTESIAN_POINT('Ctrl Pts',(-0.105858764968584,0.0923275350572008,
1.73472347597681E-17));
#40390=CARTESIAN_POINT('Ctrl Pts',(-0.104035851863276,0.0948917348608856,
1.81111115738308E-17));
#40391=CARTESIAN_POINT('Ctrl Pts',(-0.102127627911009,0.0974005222622627,
-1.86461934882118E-17));
#40392=CARTESIAN_POINT('Ctrl Pts',(-0.100145200306236,0.0998394990060757,
-1.56125112837913E-17));
#40393=CARTESIAN_POINT('Ctrl Pts',(-0.0936292563097381,0.10785605196023,
-5.64125013933619E-18));
#40394=CARTESIAN_POINT('Ctrl Pts',(-0.0862946795456802,0.115149852779714,
-9.28670353986392E-18));
#40395=CARTESIAN_POINT('Ctrl Pts',(-0.0782486257709069,0.121568627915854,
-1.38777878078145E-17));
#40396=CARTESIAN_POINT('Ctrl Pts',(-0.0735390572914751,0.125325707088318,
-1.65650710848099E-17));
#40397=CARTESIAN_POINT('Ctrl Pts',(-0.0685847970970084,0.128782722422648,
6.71820819248872E-19));
#40398=CARTESIAN_POINT('Ctrl Pts',(-0.0634007094575211,0.131904027763685,
0.));
#40399=CARTESIAN_POINT('Origin',(0.,0.,0.));
#40400=CARTESIAN_POINT('Origin',(-0.0577350269189626,-0.1,-0.3));
#40401=CARTESIAN_POINT('',(-0.0577350269189626,-0.1,-0.3));
#40402=CARTESIAN_POINT('',(0.0577350269189626,-0.1,-0.3));
#40403=CARTESIAN_POINT('',(-0.0288675134594813,-0.1,-0.3));
#40404=CARTESIAN_POINT('',(-0.0577350269189626,-0.1,-0.1));
#40405=CARTESIAN_POINT('',(-0.0577350269189626,-0.1,-0.3));
#40406=CARTESIAN_POINT('',(0.0577350269189626,-0.1,-0.1));
#40407=CARTESIAN_POINT('',(-0.0577350269189626,-0.1,-0.1));
#40408=CARTESIAN_POINT('',(0.0577350269189626,-0.1,-0.3));
#40409=CARTESIAN_POINT('Origin',(-0.115470053837925,1.41410031829988E-17,
-0.3));
#40410=CARTESIAN_POINT('',(-0.115470053837925,1.41410031829988E-17,-0.3));
#40411=CARTESIAN_POINT('',(-0.101036297108185,-0.025,-0.3));
#40412=CARTESIAN_POINT('',(-0.115470053837925,1.38777878078145E-17,-0.1));
#40413=CARTESIAN_POINT('',(-0.115470053837925,1.41410031829988E-17,-0.3));
#40414=CARTESIAN_POINT('',(-0.115470053837925,1.41410031829988E-17,-0.1));
#40415=CARTESIAN_POINT('Origin',(-0.0577350269189626,0.1,-0.3));
#40416=CARTESIAN_POINT('',(-0.0577350269189626,0.1,-0.3));
#40417=CARTESIAN_POINT('',(-0.0721687836487032,0.075,-0.3));
#40418=CARTESIAN_POINT('',(-0.0577350269189626,0.1,-0.1));
#40419=CARTESIAN_POINT('',(-0.0577350269189626,0.1,-0.3));
#40420=CARTESIAN_POINT('',(-0.0577350269189626,0.1,-0.1));
#40421=CARTESIAN_POINT('Origin',(0.0577350269189626,0.1,-0.3));
#40422=CARTESIAN_POINT('',(0.0577350269189626,0.1,-0.3));
#40423=CARTESIAN_POINT('',(0.0288675134594813,0.1,-0.3));
#40424=CARTESIAN_POINT('',(0.0577350269189626,0.1,-0.1));
#40425=CARTESIAN_POINT('',(0.0577350269189626,0.1,-0.3));
#40426=CARTESIAN_POINT('',(0.0577350269189626,0.1,-0.1));
#40427=CARTESIAN_POINT('Origin',(0.115470053837925,0.,-0.3));
#40428=CARTESIAN_POINT('',(0.115470053837925,0.,-0.3));
#40429=CARTESIAN_POINT('',(0.101036297108185,0.025,-0.3));
#40430=CARTESIAN_POINT('',(0.115470053837925,0.,-0.1));
#40431=CARTESIAN_POINT('',(0.115470053837925,0.,-0.3));
#40432=CARTESIAN_POINT('',(0.115470053837925,0.,-0.1));
#40433=CARTESIAN_POINT('Origin',(0.0577350269189626,-0.1,-0.3));
#40434=CARTESIAN_POINT('',(0.0721687836487032,-0.075,-0.3));
#40435=CARTESIAN_POINT('',(0.0577350269189626,-0.1,-0.1));
#40436=CARTESIAN_POINT('Origin',(0.,0.,-0.1));
#40437=CARTESIAN_POINT('Origin',(0.,0.,0.));
#40438=CARTESIAN_POINT('',(-0.3,-3.67394039744206E-17,0.));
#40439=CARTESIAN_POINT('Origin',(0.,0.,0.));
#40440=CARTESIAN_POINT('Origin',(0.,0.,-0.3));
#40441=CARTESIAN_POINT('',(-0.3,-3.67394039744206E-17,-0.3));
#40442=CARTESIAN_POINT('',(-0.3,-3.67394039744206E-17,-0.3));
#40443=CARTESIAN_POINT('Origin',(0.,0.,-0.3));
#40444=CARTESIAN_POINT('Origin',(0.,0.,-0.3));
#40445=CARTESIAN_POINT('Origin',(0.,0.,0.6));
#40446=CARTESIAN_POINT('',(0.,0.,0.));
#40447=CARTESIAN_POINT('Origin',(0.,0.,0.));
#40448=CARTESIAN_POINT('',(-0.146500586129689,0.000104807665585484,0.0160655045842905));
#40449=CARTESIAN_POINT('',(-0.146471000393815,0.000161627070721384,0.00893449541570859));
#40450=CARTESIAN_POINT('',(-0.14635,-1.79227059055215E-17,0.));
#40451=CARTESIAN_POINT('',(0.0634007094575212,0.131904027763685,0.));
#40452=CARTESIAN_POINT('Ctrl Pts',(-0.146500586129689,0.000104807665585484,
0.0160655045842905));
#40453=CARTESIAN_POINT('Ctrl Pts',(-0.14654494062996,0.00598698351314685,
0.0157446908947048));
#40454=CARTESIAN_POINT('Ctrl Pts',(-0.146221105349753,0.0118639507829193,
0.0154238772051191));
#40455=CARTESIAN_POINT('Ctrl Pts',(-0.145512600887712,0.0176938044004412,
0.0151030635155334));
#40456=CARTESIAN_POINT('Ctrl Pts',(-0.139696831446137,0.0655482447521769,
0.0124696595607311));
#40457=CARTESIAN_POINT('Ctrl Pts',(-0.107962161373412,0.110228180545907,
0.00983625560592885));
#40458=CARTESIAN_POINT('Ctrl Pts',(-0.06469522132477,0.13152107817143,0.0072028516511266));
#40459=CARTESIAN_POINT('Ctrl Pts',(-0.0252475006917791,0.150934428781716,
0.00480190110075107));
#40460=CARTESIAN_POINT('Ctrl Pts',(0.0237864150713563,0.150907312609249,
0.00240095055037554));
#40461=CARTESIAN_POINT('Ctrl Pts',(0.0635538308725811,0.132076982143462,
1.66967134562768E-17));
#40462=CARTESIAN_POINT('',(-0.063400709457524,0.131904027763684,0.));
#40463=CARTESIAN_POINT('Origin',(0.,0.,0.));
#40464=CARTESIAN_POINT('Ctrl Pts',(-0.0634007094575239,0.131904027763684,
1.49186218934005E-16));
#40465=CARTESIAN_POINT('Ctrl Pts',(-0.107082934395073,0.110907822426531,
0.00263534106650592));
#40466=CARTESIAN_POINT('Ctrl Pts',(-0.139152358317953,0.0667027373135744,
0.00527068213301169));
#40467=CARTESIAN_POINT('Ctrl Pts',(-0.145347393378452,0.0189333151714045,
0.00790602319951745));
#40468=CARTESIAN_POINT('Ctrl Pts',(-0.146153287982764,0.0127191260377668,
0.00824884727158116));
#40469=CARTESIAN_POINT('Ctrl Pts',(-0.14652131876894,0.00644461879462582,
0.00859167134364488));
#40470=CARTESIAN_POINT('Ctrl Pts',(-0.146471000393815,0.000161627070721384,
0.00893449541570859));
#40471=CARTESIAN_POINT('Origin',(0.,0.,0.));
#40472=CARTESIAN_POINT('',(-0.146124286466753,3.81045546672121E-5,0.0660655045842905));
#40473=CARTESIAN_POINT('',(-0.146121893894205,3.63833482308178E-5,0.0589344954157087));
#40474=CARTESIAN_POINT('',(-0.14635,-1.79227059055215E-17,0.));
#40475=CARTESIAN_POINT('Ctrl Pts',(-0.146124286466753,3.81045546672121E-5,
0.0660655045842905));
#40476=CARTESIAN_POINT('Ctrl Pts',(-0.146175624225919,0.0219480700681356,
0.0648784479568517));
#40477=CARTESIAN_POINT('Ctrl Pts',(-0.141554683648142,0.0438374299905643,
0.0636913913294129));
#40478=CARTESIAN_POINT('Ctrl Pts',(-0.132150173022132,0.0634306246655632,
0.062504334701974));
#40479=CARTESIAN_POINT('Ctrl Pts',(-0.111286909296501,0.106896787232447,
0.0598709307471717));
#40480=CARTESIAN_POINT('Ctrl Pts',(-0.0668815981213141,0.139062512957816,
0.0572375267923695));
#40481=CARTESIAN_POINT('Ctrl Pts',(-0.0190775358903001,0.145337701034954,
0.0546041228375673));
#40482=CARTESIAN_POINT('Ctrl Pts',(0.028726526340714,0.151612889112092,
0.051970718882765));
#40483=CARTESIAN_POINT('Ctrl Pts',(0.0799293396275551,0.131997539540999,
0.0493373149279628));
#40484=CARTESIAN_POINT('Ctrl Pts',(0.111303508306999,0.0953874982726326,
0.0467039109731605));
#40485=CARTESIAN_POINT('Ctrl Pts',(0.142677676986443,0.0587774570042668,
0.0440705070183582));
#40486=CARTESIAN_POINT('Ctrl Pts',(0.154223201058489,0.00517272403862895,
0.041437103063556));
#40487=CARTESIAN_POINT('Ctrl Pts',(0.14070340769012,-0.0411058697401277,
0.0388036991087537));
#40488=CARTESIAN_POINT('Ctrl Pts',(0.12718361432175,-0.0873844635188848,
0.0361702951539514));
#40489=CARTESIAN_POINT('Ctrl Pts',(0.0885985035129631,-0.12633691811076,
0.0335368911991492));
#40490=CARTESIAN_POINT('Ctrl Pts',(0.0424500313328507,-0.140301337584722,
0.030903487244347));
#40491=CARTESIAN_POINT('Ctrl Pts',(-0.00369844084726173,-0.154265757058684,
0.0282700832895447));
#40492=CARTESIAN_POINT('Ctrl Pts',(-0.0574102743986997,-0.143242141414731,
0.0256366793347424));
#40493=CARTESIAN_POINT('Ctrl Pts',(-0.0943177567692062,-0.112215861137884,
0.0230032753799401));
#40494=CARTESIAN_POINT('Ctrl Pts',(-0.126728995572139,-0.0849693486522956,
0.0206906851147236));
#40495=CARTESIAN_POINT('Ctrl Pts',(-0.146180856053097,-0.0422969446440751,
0.0183780948495071));
#40496=CARTESIAN_POINT('Ctrl Pts',(-0.146500586129689,0.000104807665585484,
0.0160655045842905));
#40497=CARTESIAN_POINT('Ctrl Pts',(-0.146471000393815,0.000161627070721384,
0.00893449541570859));
#40498=CARTESIAN_POINT('Ctrl Pts',(-0.146134513724681,-0.0418536993801969,
0.0112270124101507));
#40499=CARTESIAN_POINT('Ctrl Pts',(-0.127090283331881,-0.0842484349621326,
0.0135195294045928));
#40500=CARTESIAN_POINT('Ctrl Pts',(-0.0951738980203006,-0.111522448354846,
0.0158120463990349));
#40501=CARTESIAN_POINT('Ctrl Pts',(-0.0584847214035319,-0.142875030567541,
0.0184473874655407));
#40502=CARTESIAN_POINT('Ctrl Pts',(-0.00478572197187679,-0.154246435821546,
0.0210827285320465));
#40503=CARTESIAN_POINT('Ctrl Pts',(0.0414949714453012,-0.140576153089947,
0.0237180695985523));
#40504=CARTESIAN_POINT('Ctrl Pts',(0.0877756648624791,-0.126905870358348,
0.0263534106650582));
#40505=CARTESIAN_POINT('Ctrl Pts',(0.12663805226518,-0.0881938996411451,
0.028988751731564));
#40506=CARTESIAN_POINT('Ctrl Pts',(0.140447863117085,-0.0419714582064656,
0.0316240927980698));
#40507=CARTESIAN_POINT('Ctrl Pts',(0.154257673968991,0.00425098322821388,
0.0342594338645756));
#40508=CARTESIAN_POINT('Ctrl Pts',(0.143014908270101,0.0579838953803693,
0.0368947749310814));
#40509=CARTESIAN_POINT('Ctrl Pts',(0.111816739036639,0.0947918176848183,
0.0395301159975872));
#40510=CARTESIAN_POINT('Ctrl Pts',(0.0806185698031766,0.131599739989267,
0.042165457064093));
#40511=CARTESIAN_POINT('Ctrl Pts',(0.0294649970351413,0.15148267244601,
0.0448007981305989));
#40512=CARTESIAN_POINT('Ctrl Pts',(-0.0184028717348104,0.145423626667293,
0.0474361391971047));
#40513=CARTESIAN_POINT('Ctrl Pts',(-0.0662707405047621,0.139364580888577,
0.0500714802636105));
#40514=CARTESIAN_POINT('Ctrl Pts',(-0.11085290527663,0.107363556874401,
0.0527068213301163));
#40515=CARTESIAN_POINT('Ctrl Pts',(-0.131901071754926,0.0639489919997987,
0.0553421623966221));
#40516=CARTESIAN_POINT('Ctrl Pts',(-0.141464922191872,0.0442223138744639,
0.0565396067363176));
#40517=CARTESIAN_POINT('Ctrl Pts',(-0.146169931163403,0.0221391901971212,
0.0577370510760131));
#40518=CARTESIAN_POINT('Ctrl Pts',(-0.146121893894205,3.63833482308178E-5,
0.0589344954157087));
#40519=CARTESIAN_POINT('Origin',(0.,0.,0.));
#40520=CARTESIAN_POINT('',(-0.146368002745976,-0.000129372869328834,0.116065504584291));
#40521=CARTESIAN_POINT('',(-0.146366557616609,-0.000129983413451606,0.108934495415709));
#40522=CARTESIAN_POINT('',(-0.14635,-1.79227059055215E-17,0.));
#40523=CARTESIAN_POINT('Ctrl Pts',(-0.146368002745976,-0.000129372869328834,
0.116065504584291));
#40524=CARTESIAN_POINT('Ctrl Pts',(-0.146025111950034,0.0376095209348488,
0.114012205018999));
#40525=CARTESIAN_POINT('Ctrl Pts',(-0.131097704503774,0.0755892522017571,
0.111958905453707));
#40526=CARTESIAN_POINT('Ctrl Pts',(-0.104818007194008,0.1024708903805,0.109905605888415));
#40527=CARTESIAN_POINT('Ctrl Pts',(-0.0711136904949951,0.136947210099294,
0.107272201933612));
#40528=CARTESIAN_POINT('Ctrl Pts',(-0.0187363862257596,0.153168661700715,
0.10463879797881));
#40529=CARTESIAN_POINT('Ctrl Pts',(0.0285541005041433,0.143776766284718,
0.102005394024008));
#40530=CARTESIAN_POINT('Ctrl Pts',(0.0758445872340461,0.134384870868722,
0.0993719900692057));
#40531=CARTESIAN_POINT('Ctrl Pts',(0.118048256424616,0.0993796284353078,
0.0967385861144034));
#40532=CARTESIAN_POINT('Ctrl Pts',(0.136020336225278,0.0546403479960236,
0.0941051821596012));
#40533=CARTESIAN_POINT('Ctrl Pts',(0.153992416025939,0.00990106755673973,
0.0914717782047989));
#40534=CARTESIAN_POINT('Ctrl Pts',(0.147732906436694,-0.0445722508884142,
0.0888383742499967));
#40535=CARTESIAN_POINT('Ctrl Pts',(0.120081310876684,-0.0840688974447852,
0.0862049702951944));
#40536=CARTESIAN_POINT('Ctrl Pts',(0.092429715316675,-0.123565544001157,
0.0835715663403921));
#40537=CARTESIAN_POINT('Ctrl Pts',(0.0433860337859016,-0.148085518668745,
0.0809381623855898));
#40538=CARTESIAN_POINT('Ctrl Pts',(-0.00480217723865872,-0.146506046566169,
0.0783047584307875));
#40539=CARTESIAN_POINT('Ctrl Pts',(-0.0529903882632186,-0.144926574463593,
0.0756713544759853));
#40540=CARTESIAN_POINT('Ctrl Pts',(-0.100323128781565,-0.117247655590855,
0.0730379505211831));
#40541=CARTESIAN_POINT('Ctrl Pts',(-0.125328890902702,-0.0760248964502869,
0.0704045465663809));
#40542=CARTESIAN_POINT('Ctrl Pts',(-0.139062832915904,-0.053384075469981,
0.0689581992390174));
#40543=CARTESIAN_POINT('Ctrl Pts',(-0.146061734917782,-0.0266576901787336,
0.067511851911654));
#40544=CARTESIAN_POINT('Ctrl Pts',(-0.146124286466753,3.81045546672121E-5,
0.0660655045842905));
#40545=CARTESIAN_POINT('Ctrl Pts',(-0.146121893894205,3.63833482308178E-5,
0.0589344954157087));
#40546=CARTESIAN_POINT('Ctrl Pts',(-0.146064210518155,-0.026504769812526,
0.060372392142519));
#40547=CARTESIAN_POINT('Ctrl Pts',(-0.139152958627323,-0.0530743047642348,
0.0618102888693293));
#40548=CARTESIAN_POINT('Ctrl Pts',(-0.125571320368441,-0.0756261679111494,
0.0632481855961396));
#40549=CARTESIAN_POINT('Ctrl Pts',(-0.100679234318938,-0.116958657212465,
0.0658835266626455));
#40550=CARTESIAN_POINT('Ctrl Pts',(-0.0533808940352117,-0.144795530080065,
0.0685188677291512));
#40551=CARTESIAN_POINT('Ctrl Pts',(-0.00516183231960515,-0.146494306755382,
0.071154208795657));
#40552=CARTESIAN_POINT('Ctrl Pts',(0.0430572293960016,-0.148193083430699,
0.0737895498621628));
#40553=CARTESIAN_POINT('Ctrl Pts',(0.0921970125434883,-0.123753763913733,
0.0764248909286687));
#40554=CARTESIAN_POINT('Ctrl Pts',(0.119936668638416,-0.0842765346784538,
0.0790602319951745));
#40555=CARTESIAN_POINT('Ctrl Pts',(0.147676324733344,-0.0447993054431753,
0.0816955730616803));
#40556=CARTESIAN_POINT('Ctrl Pts',(0.154015853775713,0.00971583351041531,
0.0843309141281861));
#40557=CARTESIAN_POINT('Ctrl Pts',(0.136075382627054,0.0545053485317346,
0.0869662551946919));
#40558=CARTESIAN_POINT('Ctrl Pts',(0.118134911478395,0.0992948635530542,
0.0896015962611977));
#40559=CARTESIAN_POINT('Ctrl Pts',(0.0759144401387073,0.134358754642102,
0.0922369373277035));
#40560=CARTESIAN_POINT('Ctrl Pts',(0.0285922932904845,0.143769920707126,
0.0948722783942094));
#40561=CARTESIAN_POINT('Ctrl Pts',(-0.0187298535577381,0.15318108677215,
0.0975076194607152));
#40562=CARTESIAN_POINT('Ctrl Pts',(-0.0711536759144954,0.13693952781315,
0.100142960527221));
#40563=CARTESIAN_POINT('Ctrl Pts',(-0.104866248150923,0.102422641268563,
0.102778301593727));
#40564=CARTESIAN_POINT('Ctrl Pts',(-0.131117262559492,0.0755453303453163,
0.104830366201054));
#40565=CARTESIAN_POINT('Ctrl Pts',(-0.146023101823344,0.0375871567885092,
0.106882430808381));
#40566=CARTESIAN_POINT('Ctrl Pts',(-0.146366557616609,-0.000129983413451606,
0.108934495415709));
#40567=CARTESIAN_POINT('Origin',(0.,0.,0.));
#40568=CARTESIAN_POINT('',(-0.14651736545536,8.65668654492988E-5,0.166065504584291));
#40569=CARTESIAN_POINT('',(-0.146524127737672,8.31850724179233E-5,0.158934495415709));
#40570=CARTESIAN_POINT('',(-0.14635,-1.79227059055215E-17,0.));
#40571=CARTESIAN_POINT('Ctrl Pts',(-0.14651736545536,8.65668654492988E-5,
0.166065504584291));
#40572=CARTESIAN_POINT('Ctrl Pts',(-0.146554285531508,0.00533178393548585,
0.165779366035948));
#40573=CARTESIAN_POINT('Ctrl Pts',(-0.146296777197391,0.0105733383781062,
0.165493227487605));
#40574=CARTESIAN_POINT('Ctrl Pts',(-0.145732753046151,0.0157816995937671,
0.165207088939262));
#40575=CARTESIAN_POINT('Ctrl Pts',(-0.140541899038255,0.0637155382981208,
0.16257368498446));
#40576=CARTESIAN_POINT('Ctrl Pts',(-0.109389226009343,0.108837918334108,
0.159940281029658));
#40577=CARTESIAN_POINT('Ctrl Pts',(-0.0664064572564633,0.130680066597967,
0.157306877074855));
#40578=CARTESIAN_POINT('Ctrl Pts',(-0.0234236885035836,0.152522214861825,
0.154673473120053));
#40579=CARTESIAN_POINT('Ctrl Pts',(0.031389175973264,0.151084131353554,
0.152040069165251));
#40580=CARTESIAN_POINT('Ctrl Pts',(0.073167488832194,0.12701817148098,0.149406665210449));
#40581=CARTESIAN_POINT('Ctrl Pts',(0.114945801691124,0.102952211608407,
0.146773261255646));
#40582=CARTESIAN_POINT('Ctrl Pts',(0.143689562932137,0.0562583753715299,
0.144139857300844));
#40583=CARTESIAN_POINT('Ctrl Pts',(0.146359798857064,0.00811829104130666,
0.141506453346042));
#40584=CARTESIAN_POINT('Ctrl Pts',(0.149030034781992,-0.0400217932889162,
0.13887304939124));
#40585=CARTESIAN_POINT('Ctrl Pts',(0.125626745390835,-0.0896081257124856,
0.136239645436437));
#40586=CARTESIAN_POINT('Ctrl Pts',(0.0867663172267087,-0.118146957909964,
0.133606241481635));
#40587=CARTESIAN_POINT('Ctrl Pts',(0.0479058890625822,-0.146685790107443,
0.130972837526833));
#40588=CARTESIAN_POINT('Ctrl Pts',(-0.00641167787451363,-0.154177122078832,
0.128339433572031));
#40589=CARTESIAN_POINT('Ctrl Pts',(-0.0515464175662268,-0.13722267989126,
0.125706029617228));
#40590=CARTESIAN_POINT('Ctrl Pts',(-0.0966811572579399,-0.120268237703689,
0.123072625662426));
#40591=CARTESIAN_POINT('Ctrl Pts',(-0.13263306970427,-0.0788680213571585,
0.120439221707624));
#40592=CARTESIAN_POINT('Ctrl Pts',(-0.143093361363041,-0.0318023192658095,
0.117805817752821));
#40593=CARTESIAN_POINT('Ctrl Pts',(-0.145397626569199,-0.0214343617297895,
0.117225713363311));
#40594=CARTESIAN_POINT('Ctrl Pts',(-0.146464877288401,-0.0107914790330514,
0.116645608973801));
#40595=CARTESIAN_POINT('Ctrl Pts',(-0.146368002745976,-0.000129372869328834,
0.116065504584291));
#40596=CARTESIAN_POINT('Ctrl Pts',(-0.146366557616609,-0.000129983413451606,
0.108934495415709));
#40597=CARTESIAN_POINT('Ctrl Pts',(-0.146464181092139,-0.0108506595114597,
0.109517771874887));
#40598=CARTESIAN_POINT('Ctrl Pts',(-0.145385284604313,-0.0215518621108894,
0.110101048334066));
#40599=CARTESIAN_POINT('Ctrl Pts',(-0.143055987718722,-0.0319735935649507,
0.110684324793244));
#40600=CARTESIAN_POINT('Ctrl Pts',(-0.132531832933994,-0.0790607277237021,
0.11331966585975));
#40601=CARTESIAN_POINT('Ctrl Pts',(-0.0964822012484396,-0.12044278191103,
0.115955006926256));
#40602=CARTESIAN_POINT('Ctrl Pts',(-0.0512822836387571,-0.13732242834474,
0.118590347992762));
#40603=CARTESIAN_POINT('Ctrl Pts',(-0.00608236602907434,-0.154202074778449,
0.121225689059267));
#40604=CARTESIAN_POINT('Ctrl Pts',(0.0482678375047366,-0.14657931345854,
0.123861030125773));
#40605=CARTESIAN_POINT('Ctrl Pts',(0.0870803134198012,-0.117916681520738,
0.126496371192279));
#40606=CARTESIAN_POINT('Ctrl Pts',(0.125892789334866,-0.089254049582936,
0.129131712258785));
#40607=CARTESIAN_POINT('Ctrl Pts',(0.149167537631184,-0.0395515470272406,
0.131767053325291));
#40608=CARTESIAN_POINT('Ctrl Pts',(0.146332238452734,0.00861396207485353,
0.134402394391797));
#40609=CARTESIAN_POINT('Ctrl Pts',(0.143496939274284,0.0567794711769477,
0.137037735458302));
#40610=CARTESIAN_POINT('Ctrl Pts',(0.114551592621066,0.103407986825441,
0.139673076524808));
#40611=CARTESIAN_POINT('Ctrl Pts',(0.0726443273415577,0.127318991170589,
0.142308417591314));
#40612=CARTESIAN_POINT('Ctrl Pts',(0.0307370620620493,0.151229995515737,
0.14494375865782));
#40613=CARTESIAN_POINT('Ctrl Pts',(-0.0241321218437492,0.152423488557541,
0.147579099724326));
#40614=CARTESIAN_POINT('Ctrl Pts',(-0.067039462170215,0.130357334843671,
0.150214440790831));
#40615=CARTESIAN_POINT('Ctrl Pts',(-0.109946802496681,0.108291181129802,
0.152849781857337));
#40616=CARTESIAN_POINT('Ctrl Pts',(-0.140892299243814,0.0629653806602592,
0.155485122923843));
#40617=CARTESIAN_POINT('Ctrl Pts',(-0.145819277598255,0.0149687147614827,
0.158120463990349));
#40618=CARTESIAN_POINT('Ctrl Pts',(-0.1463265762883,0.0100268124462353,
0.158391807798802));
#40619=CARTESIAN_POINT('Ctrl Pts',(-0.146558040382541,0.0050565950257616,
0.158663151607255));
#40620=CARTESIAN_POINT('Ctrl Pts',(-0.146524127737672,8.31850724179233E-5,
0.158934495415709));
#40621=CARTESIAN_POINT('Origin',(0.,0.,0.));
#40622=CARTESIAN_POINT('',(-0.146129957599089,4.76874783713124E-5,0.21606550458429));
#40623=CARTESIAN_POINT('',(-0.146134590291164,5.53529746073057E-5,0.208934495415709));
#40624=CARTESIAN_POINT('',(-0.14635,-1.79227059055215E-17,0.));
#40625=CARTESIAN_POINT('Ctrl Pts',(-0.146129957599089,4.76874783713124E-5,
0.21606550458429));
#40626=CARTESIAN_POINT('Ctrl Pts',(-0.146192738333019,0.0213155226117273,
0.214913123098095));
#40627=CARTESIAN_POINT('Ctrl Pts',(-0.14184845306411,0.0425589323614883,
0.213760741611899));
#40628=CARTESIAN_POINT('Ctrl Pts',(-0.132968065125987,0.0616975770053832,
0.212608360125703));
#40629=CARTESIAN_POINT('Ctrl Pts',(-0.11267474299563,0.105432905191852,
0.2099749561709));
#40630=CARTESIAN_POINT('Ctrl Pts',(-0.0686935897650435,0.13817700942041,
0.207341552216098));
#40631=CARTESIAN_POINT('Ctrl Pts',(-0.0209756858809845,0.145076248759314,
0.204708148261296));
#40632=CARTESIAN_POINT('Ctrl Pts',(0.0267422180030747,0.151975488098219,
0.202074744306494));
#40633=CARTESIAN_POINT('Ctrl Pts',(0.0781968725406062,0.13302986254747,
0.199441340351692));
#40634=CARTESIAN_POINT('Ctrl Pts',(0.110047008199114,0.0968336374273772,
0.196807936396889));
#40635=CARTESIAN_POINT('Ctrl Pts',(0.141897143857622,0.0606374123072843,
0.194174532442087));
#40636=CARTESIAN_POINT('Ctrl Pts',(0.154142760637107,0.00719058761784734,
0.191541128487285));
#40637=CARTESIAN_POINT('Ctrl Pts',(0.141228904479148,-0.0392618630629832,
0.188907724532483));
#40638=CARTESIAN_POINT('Ctrl Pts',(0.128315048321188,-0.0857143137438141,
0.18627432057768));
#40639=CARTESIAN_POINT('Ctrl Pts',(0.0902417192257834,-0.125172390416039,
0.183640916622878));
#40640=CARTESIAN_POINT('Ctrl Pts',(0.0442800434850501,-0.139736806546778,
0.181007512668076));
#40641=CARTESIAN_POINT('Ctrl Pts',(-0.00168163225568323,-0.154301222677517,
0.178374108713273));
#40642=CARTESIAN_POINT('Ctrl Pts',(-0.0555316546417454,-0.143971978266771,
0.175740704758471));
#40643=CARTESIAN_POINT('Ctrl Pts',(-0.0928421483413364,-0.113434707375038,
0.173107300803669));
#40644=CARTESIAN_POINT('Ctrl Pts',(-0.126098584749153,-0.0862155337115625,
0.17076003539721));
#40645=CARTESIAN_POINT('Ctrl Pts',(-0.146214500923306,-0.0429412483281845,
0.16841276999075));
#40646=CARTESIAN_POINT('Ctrl Pts',(-0.14651736545536,8.65668654492988E-5,
0.166065504584291));
#40647=CARTESIAN_POINT('Ctrl Pts',(-0.146524127737672,8.31850724179233E-5,
0.158934495415709));
#40648=CARTESIAN_POINT('Ctrl Pts',(-0.146228674526712,-0.043246078859919,
0.161298492673761));
#40649=CARTESIAN_POINT('Ctrl Pts',(-0.125790555024919,-0.0868176629158599,
0.163662489931814));
#40650=CARTESIAN_POINT('Ctrl Pts',(-0.0921252733308782,-0.11401867430555,
0.166026487189866));
#40651=CARTESIAN_POINT('Ctrl Pts',(-0.0545958307473115,-0.144341866145796,
0.168661828256372));
#40652=CARTESIAN_POINT('Ctrl Pts',(-0.000628485618429035,-0.154320718498276,
0.171297169322878));
#40653=CARTESIAN_POINT('Ctrl Pts',(0.0452626498105411,-0.139422439628514,
0.173932510389384));
#40654=CARTESIAN_POINT('Ctrl Pts',(0.0911537852395115,-0.124524160758753,
0.17656785145589));
#40655=CARTESIAN_POINT('Ctrl Pts',(0.128968710968569,-0.0847487506667484,
0.179203192522395));
#40656=CARTESIAN_POINT('Ctrl Pts',(0.141530385150016,-0.0381637812674535,
0.181838533588901));
#40657=CARTESIAN_POINT('Ctrl Pts',(0.154092059331463,0.00842118813184087,
0.184473874655407));
#40658=CARTESIAN_POINT('Ctrl Pts',(0.141400481965299,0.0618157168384256,
0.187109215721913));
#40659=CARTESIAN_POINT('Ctrl Pts',(0.109220671810841,0.0977658885483793,
0.189744556788419));
#40660=CARTESIAN_POINT('Ctrl Pts',(0.0770408616563825,0.133716060258333,
0.192379897854925));
#40661=CARTESIAN_POINT('Ctrl Pts',(0.025372818713629,0.152221874971656,
0.19501523892143));
#40662=CARTESIAN_POINT('Ctrl Pts',(-0.022313779030084,0.144877256285936,
0.197650579987936));
#40663=CARTESIAN_POINT('Ctrl Pts',(-0.0700003767737975,0.137532637600217,
0.200285921054442));
#40664=CARTESIAN_POINT('Ctrl Pts',(-0.113705529318471,0.104337585515455,
0.202921262120948));
#40665=CARTESIAN_POINT('Ctrl Pts',(-0.133576619842631,0.0603706116554267,
0.205556603187454));
#40666=CARTESIAN_POINT('Ctrl Pts',(-0.142066653397378,0.041585478402751,
0.206682567263539));
#40667=CARTESIAN_POINT('Ctrl Pts',(-0.146205843323087,0.0208339599326467,
0.207808531339624));
#40668=CARTESIAN_POINT('Ctrl Pts',(-0.146134590291164,5.53529746073057E-5,
0.208934495415709));
#40669=CARTESIAN_POINT('Origin',(0.,0.,0.));
#40670=CARTESIAN_POINT('',(-0.146348968946192,-0.000130334789587572,0.266065504584291));
#40671=CARTESIAN_POINT('',(-0.146327394052832,-0.000130859996972892,0.258934495415708));
#40672=CARTESIAN_POINT('',(-0.14635,-1.79227059055215E-17,0.));
#40673=CARTESIAN_POINT('Ctrl Pts',(-0.146348968946192,-0.000130334789587572,
0.266065504584291));
#40674=CARTESIAN_POINT('Ctrl Pts',(-0.146013620606683,0.0369836123692833,
0.264046880160242));
#40675=CARTESIAN_POINT('Ctrl Pts',(-0.131636768783893,0.074328824870482,
0.262028255736193));
#40676=CARTESIAN_POINT('Ctrl Pts',(-0.106148536005423,0.10109196632601,
0.260009631312144));
#40677=CARTESIAN_POINT('Ctrl Pts',(-0.072897767709896,0.136005921449249,
0.257376227357342));
#40678=CARTESIAN_POINT('Ctrl Pts',(-0.020736980756812,0.152910669462462,
0.254742823402539));
#40679=CARTESIAN_POINT('Ctrl Pts',(0.0266722339182632,0.144137744153214,
0.252109419447737));
#40680=CARTESIAN_POINT('Ctrl Pts',(0.0740814485933381,0.135364818843967,
0.249476015492935));
#40681=CARTESIAN_POINT('Ctrl Pts',(0.116739090990404,0.100914220212258,
0.246842611538132));
#40682=CARTESIAN_POINT('Ctrl Pts',(0.135294462171964,0.056413702744499,
0.24420920758333));
#40683=CARTESIAN_POINT('Ctrl Pts',(0.153849833353525,0.0119131852767396,
0.241575803628528));
#40684=CARTESIAN_POINT('Ctrl Pts',(0.148302933319579,-0.0426372510270706,
0.238942399673726));
#40685=CARTESIAN_POINT('Ctrl Pts',(0.121169990969772,-0.082492003492008,
0.236308995718923));
#40686=CARTESIAN_POINT('Ctrl Pts',(0.094037048619966,-0.122346755956945,
0.233675591764121));
#40687=CARTESIAN_POINT('Ctrl Pts',(0.0453180639542996,-0.14750582458301,
0.231042187809319));
#40688=CARTESIAN_POINT('Ctrl Pts',(-0.00288666981273841,-0.146556352606171,
0.228408783854516));
#40689=CARTESIAN_POINT('Ctrl Pts',(-0.0510914035797761,-0.145606880629331,
0.225775379899714));
#40690=CARTESIAN_POINT('Ctrl Pts',(-0.0987818864481854,-0.118548868049589,
0.223141975944912));
#40691=CARTESIAN_POINT('Ctrl Pts',(-0.124324382367327,-0.0776565856875276,
0.22050857199011));
#40692=CARTESIAN_POINT('Ctrl Pts',(-0.138689444093445,-0.0546588268893121,
0.219027549521503));
#40693=CARTESIAN_POINT('Ctrl Pts',(-0.146049272792313,-0.0272853980218952,
0.217546527052897));
#40694=CARTESIAN_POINT('Ctrl Pts',(-0.146129957599089,4.76874783713124E-5,
0.21606550458429));
#40695=CARTESIAN_POINT('Ctrl Pts',(-0.146134590291164,5.53529746073057E-5,
0.208934495415709));
#40696=CARTESIAN_POINT('Ctrl Pts',(-0.146039074200404,-0.0277987783441389,
0.210443872406129));
#40697=CARTESIAN_POINT('Ctrl Pts',(-0.138377421661147,-0.055701587485614,
0.21195324939655));
#40698=CARTESIAN_POINT('Ctrl Pts',(-0.123487844473835,-0.0789814939515912,
0.213462626386971));
#40699=CARTESIAN_POINT('Ctrl Pts',(-0.0974909500772326,-0.119627730063286,
0.216097967453477));
#40700=CARTESIAN_POINT('Ctrl Pts',(-0.0494601327803805,-0.146181306651382,
0.218733308519983));
#40701=CARTESIAN_POINT('Ctrl Pts',(-0.00121289818784218,-0.14658053417448,
0.221368649586488));
#40702=CARTESIAN_POINT('Ctrl Pts',(0.047034336404696,-0.146979761697578,
0.224003990652994));
#40703=CARTESIAN_POINT('Ctrl Pts',(0.0954979882929203,-0.121224640155678,
0.2266393317195));
#40704=CARTESIAN_POINT('Ctrl Pts',(0.122163941197393,-0.0810141690783142,
0.229274672786006));
#40705=CARTESIAN_POINT('Ctrl Pts',(0.148829894101866,-0.0408036980009502,
0.231910013852512));
#40706=CARTESIAN_POINT('Ctrl Pts',(0.153698148022588,0.0138621226118777,
0.234545354919018));
#40707=CARTESIAN_POINT('Ctrl Pts',(0.134557348601142,0.0581519050223658,
0.237180695985524));
#40708=CARTESIAN_POINT('Ctrl Pts',(0.115416549179696,0.102441687432854,
0.239816037052029));
#40709=CARTESIAN_POINT('Ctrl Pts',(0.0722666964160822,0.136355431641002,
0.242451378118535));
#40710=CARTESIAN_POINT('Ctrl Pts',(0.0247081678934101,0.144488167542617,
0.245086719185041));
#40711=CARTESIAN_POINT('Ctrl Pts',(-0.0228503606292616,0.152620903444231,
0.247722060251547));
#40712=CARTESIAN_POINT('Ctrl Pts',(-0.0748175649109913,0.134972631039312,
0.250357401318053));
#40713=CARTESIAN_POINT('Ctrl Pts',(-0.107587875971466,0.0995598968678148,
0.252992742384558));
#40714=CARTESIAN_POINT('Ctrl Pts',(-0.132216325719399,0.072945540282363,
0.254973326728275));
#40715=CARTESIAN_POINT('Ctrl Pts',(-0.146001912399175,0.0362973920726889,
0.256953911071992));
#40716=CARTESIAN_POINT('Ctrl Pts',(-0.146327394052832,-0.000130859996972892,
0.258934495415708));
#40717=CARTESIAN_POINT('Origin',(0.,0.,0.));
#40718=CARTESIAN_POINT('',(-0.146531331768327,7.78185235384022E-5,0.316065504584291));
#40719=CARTESIAN_POINT('',(-0.146550416329645,6.385150607816E-5,0.308934495415709));
#40720=CARTESIAN_POINT('',(-0.14635,-1.79227059055215E-17,0.));
#40721=CARTESIAN_POINT('Ctrl Pts',(-0.146531331768327,7.78185235384022E-5,
0.316065504584291));
#40722=CARTESIAN_POINT('Ctrl Pts',(-0.14656115307709,0.00468624689283061,
0.315814041177191));
#40723=CARTESIAN_POINT('Ctrl Pts',(-0.14636239679671,0.00929207042467623,
0.315562577770091));
#40724=CARTESIAN_POINT('Ctrl Pts',(-0.145926597573945,0.0138753548512781,
0.315311114362991));
#40725=CARTESIAN_POINT('Ctrl Pts',(-0.14136277093227,0.0618729520929492,
0.312677710408189));
#40726=CARTESIAN_POINT('Ctrl Pts',(-0.110802592512226,0.10739869970775,
0.310044306453387));
#40727=CARTESIAN_POINT('Ctrl Pts',(-0.0681090134487845,0.12980084606346,
0.307410902498584));
#40728=CARTESIAN_POINT('Ctrl Pts',(-0.0254154343853437,0.152202992419171,
0.304777498543782));
#40729=CARTESIAN_POINT('Ctrl Pts',(0.0294115453214934,0.151481537515791,
0.30214409458898));
#40730=CARTESIAN_POINT('Ctrl Pts',(0.0715008751789212,0.127963753463258,
0.299510690634177));
#40731=CARTESIAN_POINT('Ctrl Pts',(0.113590205036349,0.104445969410725,
0.296877286679375));
#40732=CARTESIAN_POINT('Ctrl Pts',(0.142941885044368,0.0581318562090376,
0.294243882724573));
#40733=CARTESIAN_POINT('Ctrl Pts',(0.146241172727074,0.0100307901566561,
0.291610478769771));
#40734=CARTESIAN_POINT('Ctrl Pts',(0.149540460409781,-0.038070275895725,
0.288977074814969));
#40735=CARTESIAN_POINT('Ctrl Pts',(0.126787355767176,-0.0879582947988004,
0.286343670860166));
#40736=CARTESIAN_POINT('Ctrl Pts',(0.0883033030491544,-0.117002666731855,
0.283710266905364));
#40737=CARTESIAN_POINT('Ctrl Pts',(0.0498192503311324,-0.14604703866491,
0.281076862950562));
#40738=CARTESIAN_POINT('Ctrl Pts',(-0.00439575046230666,-0.154247763627944,
0.27844345899576));
#40739=CARTESIAN_POINT('Ctrl Pts',(-0.0497482595792165,-0.137884763554925,
0.275810055040957));
#40740=CARTESIAN_POINT('Ctrl Pts',(-0.0951007686961262,-0.121521763481905,
0.273176651086155));
#40741=CARTESIAN_POINT('Ctrl Pts',(-0.131590786136507,-0.0805950383728307,
0.270543247131353));
#40742=CARTESIAN_POINT('Ctrl Pts',(-0.142665420037712,-0.0336700947016615,
0.26790984317655));
#40743=CARTESIAN_POINT('Ctrl Pts',(-0.145250841169412,-0.0227152638644948,
0.267295063645797));
#40744=CARTESIAN_POINT('Ctrl Pts',(-0.146451100522698,-0.0114335245988962,
0.266680284115044));
#40745=CARTESIAN_POINT('Ctrl Pts',(-0.146348968946192,-0.000130334789587572,
0.266065504584291));
#40746=CARTESIAN_POINT('Ctrl Pts',(-0.146327394052832,-0.000130859996972892,
0.258934495415708));
#40747=CARTESIAN_POINT('Ctrl Pts',(-0.146434994267663,-0.0121735902233998,
0.259589252138497));
#40748=CARTESIAN_POINT('Ctrl Pts',(-0.145071563913279,-0.0241922883978194,
0.260244008861286));
#40749=CARTESIAN_POINT('Ctrl Pts',(-0.142142543798705,-0.0358164956803284,
0.260898765584076));
#40750=CARTESIAN_POINT('Ctrl Pts',(-0.130353482726251,-0.0826029581188991,
0.263534106650581));
#40751=CARTESIAN_POINT('Ctrl Pts',(-0.0932019427421253,-0.122998687057965,
0.266169447717088));
#40752=CARTESIAN_POINT('Ctrl Pts',(-0.0475636294365445,-0.138654337383406,
0.268804788783593));
#40753=CARTESIAN_POINT('Ctrl Pts',(-0.00192531613096394,-0.154309987708848,
0.271440129850099));
#40754=CARTESIAN_POINT('Ctrl Pts',(0.0521997704960722,-0.145225559420664,
0.274075470916605));
#40755=CARTESIAN_POINT('Ctrl Pts',(0.090225865564854,-0.115527560795972,
0.27671081198311));
#40756=CARTESIAN_POINT('Ctrl Pts',(0.128251960633635,-0.0858295621712801,
0.279346153049616));
#40757=CARTESIAN_POINT('Ctrl Pts',(0.150179064144164,-0.0355179932100797,
0.281981494116122));
#40758=CARTESIAN_POINT('Ctrl Pts',(0.14604701445983,0.0125536324530514,
0.284616835182628));
#40759=CARTESIAN_POINT('Ctrl Pts',(0.141914964775496,0.0606252581161832,
0.287252176249134));
#40760=CARTESIAN_POINT('Ctrl Pts',(0.1117237618963,0.106456940481245,0.28988751731564));
#40761=CARTESIAN_POINT('Ctrl Pts',(0.0691874497467596,0.129230108403338,
0.292522858382145));
#40762=CARTESIAN_POINT('Ctrl Pts',(0.02665113759722,0.152003276325431,0.295158199448651));
#40763=CARTESIAN_POINT('Ctrl Pts',(-0.0282302838226635,0.151717929804555,
0.297793540515157));
#40764=CARTESIAN_POINT('Ctrl Pts',(-0.0705274923191129,0.128503684568086,
0.300428881581663));
#40765=CARTESIAN_POINT('Ctrl Pts',(-0.112824700815562,0.105289439331617,
0.303064222648169));
#40766=CARTESIAN_POINT('Ctrl Pts',(-0.142537696388578,0.0591462953795561,
0.305699563714675));
#40767=CARTESIAN_POINT('Ctrl Pts',(-0.146169655872548,0.0110343020847702,
0.30833490478118));
#40768=CARTESIAN_POINT('Ctrl Pts',(-0.146445102685266,0.00738550168790281,
0.308534768326023));
#40769=CARTESIAN_POINT('Ctrl Pts',(-0.146570540139926,0.00372537713102106,
0.308734631870866));
#40770=CARTESIAN_POINT('Ctrl Pts',(-0.146550416329645,6.385150607816E-5,
0.308934495415709));
#40771=CARTESIAN_POINT('Origin',(0.,0.,0.));
#40772=CARTESIAN_POINT('',(-0.146136883584905,5.71367125724795E-5,0.366065504584291));
#40773=CARTESIAN_POINT('',(-0.14615227160514,7.39083677616704E-5,0.358934495415709));
#40774=CARTESIAN_POINT('',(-0.14635,-1.79227059055215E-17,0.));
#40775=CARTESIAN_POINT('Ctrl Pts',(-0.146136883584905,5.71367125724795E-5,
0.366065504584291));
#40776=CARTESIAN_POINT('Ctrl Pts',(-0.14621004407594,0.0206825763459024,
0.364947798239338));
#40777=CARTESIAN_POINT('Ctrl Pts',(-0.142132997319362,0.0412803999606639,
0.363830091894385));
#40778=CARTESIAN_POINT('Ctrl Pts',(-0.133763205647759,0.0599541672162359,
0.362712385549432));
#40779=CARTESIAN_POINT('Ctrl Pts',(-0.114043318945497,0.10395102986619,
0.360078981594629));
#40780=CARTESIAN_POINT('Ctrl Pts',(-0.070493949429046,0.137267251375705,
0.357445577639827));
#40781=CARTESIAN_POINT('Ctrl Pts',(-0.0228703083824292,0.144789662428813,
0.354812173685025));
#40782=CARTESIAN_POINT('Ctrl Pts',(0.0247533326641879,0.15231207348192,
0.352178769730223));
#40783=CARTESIAN_POINT('Ctrl Pts',(0.0764512452409704,0.13404067407862,
0.34954536577542));
#40784=CARTESIAN_POINT('Ctrl Pts',(0.108771811167509,0.0982638817017563,
0.346911961820618));
#40785=CARTESIAN_POINT('Ctrl Pts',(0.141092377094047,0.0624870893248929,
0.344278557865816));
#40786=CARTESIAN_POINT('Ctrl Pts',(0.154035596370341,0.00920490397446603,
0.341645153911014));
#40787=CARTESIAN_POINT('Ctrl Pts',(0.141730062949927,-0.0374123857561472,
0.339011749956212));
#40788=CARTESIAN_POINT('Ctrl Pts',(0.129424529529512,-0.0840296754867619,
0.336378346001409));
#40789=CARTESIAN_POINT('Ctrl Pts',(0.0918702434123863,-0.123982069597563,
0.333744942046607));
#40790=CARTESIAN_POINT('Ctrl Pts',(0.0461028784809079,-0.139146045389481,
0.331111538091804));
#40791=CARTESIAN_POINT('Ctrl Pts',(0.000335513549430837,-0.154310021181399,
0.328478134137002));
#40792=CARTESIAN_POINT('Ctrl Pts',(-0.0536449301963988,-0.144685578654437,
0.3258447301822));
#40793=CARTESIAN_POINT('Ctrl Pts',(-0.0913514146376612,-0.114638633956686,
0.323211326227398));
#40794=CARTESIAN_POINT('Ctrl Pts',(-0.125457311698448,-0.0874608681681781,
0.320829385679696));
#40795=CARTESIAN_POINT('Ctrl Pts',(-0.146248854944573,-0.043574665631504,
0.318447445131993));
#40796=CARTESIAN_POINT('Ctrl Pts',(-0.146531331768327,7.78185235384022E-5,
0.316065504584291));
#40797=CARTESIAN_POINT('Ctrl Pts',(-0.146550416329645,6.385150607816E-5,
0.308934495415709));
#40798=CARTESIAN_POINT('Ctrl Pts',(-0.146305193582165,-0.0445544072241828,
0.311369972937372));
#40799=CARTESIAN_POINT('Ctrl Pts',(-0.1244453858937,-0.0893807124057277,
0.313805450459035));
#40800=CARTESIAN_POINT('Ctrl Pts',(-0.0890196886128741,-0.116459517256704,
0.316240927980698));
#40801=CARTESIAN_POINT('Ctrl Pts',(-0.0506868384743053,-0.145760500665881,
0.318876269047204));
#40802=CARTESIAN_POINT('Ctrl Pts',(0.00352978519775653,-0.154281624846726,
0.321511610113709));
#40803=CARTESIAN_POINT('Ctrl Pts',(0.0490028377607838,-0.138152256629371,
0.324146951180215));
#40804=CARTESIAN_POINT('Ctrl Pts',(0.0944758903238113,-0.122022888412016,
0.326782292246721));
#40805=CARTESIAN_POINT('Ctrl Pts',(0.131205371777804,-0.0812430277964604,
0.329417633313227));
#40806=CARTESIAN_POINT('Ctrl Pts',(0.142507292286359,-0.034336507766627,
0.332052974379733));
#40807=CARTESIAN_POINT('Ctrl Pts',(0.153809212794913,0.0125700122632054,
0.334688315446239));
#40808=CARTESIAN_POINT('Ctrl Pts',(0.139683572358031,0.0656031917073164,
0.337323656512744));
#40809=CARTESIAN_POINT('Ctrl Pts',(0.106546798111412,0.1006732533129,0.33995899757925));
#40810=CARTESIAN_POINT('Ctrl Pts',(0.0734100238647925,0.135743314918485,
0.342594338645756));
#40811=CARTESIAN_POINT('Ctrl Pts',(0.0212621158084357,0.152850258685541,
0.345229679712262));
#40812=CARTESIAN_POINT('Ctrl Pts',(-0.026209274243358,0.144223431050692,
0.347865020778768));
#40813=CARTESIAN_POINT('Ctrl Pts',(-0.0736806642951504,0.135596603415843,
0.350500361845274));
#40814=CARTESIAN_POINT('Ctrl Pts',(-0.11647553634238,0.10123600437909,0.353135702911779));
#40815=CARTESIAN_POINT('Ctrl Pts',(-0.135154759147093,0.056749583260925,
0.355771043978285));
#40816=CARTESIAN_POINT('Ctrl Pts',(-0.142628910530197,0.0389491506944377,
0.356825527790759));
#40817=CARTESIAN_POINT('Ctrl Pts',(-0.146242014510603,0.0195275186049996,
0.357880011603234));
#40818=CARTESIAN_POINT('Ctrl Pts',(-0.14615227160514,7.39083677616704E-5,
0.358934495415709));
#40819=CARTESIAN_POINT('Origin',(0.,0.,0.));
#40820=CARTESIAN_POINT('',(-0.146330070388523,-0.000130413829425732,0.416065504584291));
#40821=CARTESIAN_POINT('',(-0.146289342453438,-0.000128032530387096,0.408934495415709));
#40822=CARTESIAN_POINT('',(-0.14635,-1.79227059055215E-17,0.));
#40823=CARTESIAN_POINT('Ctrl Pts',(-0.146330070388523,-0.000130413829425732,
0.416065504584291));
#40824=CARTESIAN_POINT('Ctrl Pts',(-0.146004163689088,0.0363580550473478,
0.414081555301485));
#40825=CARTESIAN_POINT('Ctrl Pts',(-0.13216535679172,0.0730671490760677,
0.412097606018678));
#40826=CARTESIAN_POINT('Ctrl Pts',(-0.107460925463154,0.0996957714768259,
0.410113656735872));
#40827=CARTESIAN_POINT('Ctrl Pts',(-0.0746693880354573,0.135041392531165,
0.40748025278107));
#40828=CARTESIAN_POINT('Ctrl Pts',(-0.0227340340094623,0.152626534075836,
0.404846848826268));
#40829=CARTESIAN_POINT('Ctrl Pts',(0.0247858083562081,0.144474084374625,
0.402213444871466));
#40830=CARTESIAN_POINT('Ctrl Pts',(0.0723056507218785,0.136321634673413,
0.399580040916663));
#40831=CARTESIAN_POINT('Ctrl Pts',(0.115409981427224,0.102431593726319,
0.396946636961861));
#40832=CARTESIAN_POINT('Ctrl Pts',(0.134545471232452,0.0581774313853258,
0.394313233007059));
#40833=CARTESIAN_POINT('Ctrl Pts',(0.15368096103768,0.0139232690443328,
0.391679829052256));
#40834=CARTESIAN_POINT('Ctrl Pts',(0.14884760994279,-0.0406950146905586,
0.389046425097455));
#40835=CARTESIAN_POINT('Ctrl Pts',(0.122237961103967,-0.0809010396527884,
0.386413021142652));
#40836=CARTESIAN_POINT('Ctrl Pts',(0.0956283122651433,-0.121107064615018,
0.38377961718785));
#40837=CARTESIAN_POINT('Ctrl Pts',(0.0472423656823864,-0.146900830804586,
0.381146213233048));
#40838=CARTESIAN_POINT('Ctrl Pts',(-0.000970660813290544,-0.146581564902762,
0.378512809278245));
#40839=CARTESIAN_POINT('Ctrl Pts',(-0.0491836873089679,-0.146262299000937,
0.375879405323443));
#40840=CARTESIAN_POINT('Ctrl Pts',(-0.0972237937175652,-0.11983000100772,
0.373246001368641));
#40841=CARTESIAN_POINT('Ctrl Pts',(-0.123298644977828,-0.0792751001159155,
0.370612597413839));
#40842=CARTESIAN_POINT('Ctrl Pts',(-0.138306441127099,-0.0559330806595814,
0.369096899803989));
#40843=CARTESIAN_POINT('Ctrl Pts',(-0.146037672211633,-0.0279125797478292,
0.36758120219414));
#40844=CARTESIAN_POINT('Ctrl Pts',(-0.146136883584905,5.71367125724795E-5,
0.366065504584291));
#40845=CARTESIAN_POINT('Ctrl Pts',(-0.14615227160514,7.39083677616704E-5,
0.358934495415709));
#40846=CARTESIAN_POINT('Ctrl Pts',(-0.146017731158506,-0.0290904851457483,
0.36051535266974));
#40847=CARTESIAN_POINT('Ctrl Pts',(-0.137560931614845,-0.0583267505026361,
0.362096209923772));
#40848=CARTESIAN_POINT('Ctrl Pts',(-0.121314920725415,-0.0822800955868649,
0.363677067177803));
#40849=CARTESIAN_POINT('Ctrl Pts',(-0.0942322859368278,-0.122211110116912,
0.366312408244309));
#40850=CARTESIAN_POINT('Ctrl Pts',(-0.0455034427974572,-0.147460895977431,
0.368947749310814));
#40851=CARTESIAN_POINT('Ctrl Pts',(0.00273703201223555,-0.146559997189415,
0.37158309037732));
#40852=CARTESIAN_POINT('Ctrl Pts',(0.050977506821928,-0.145659098401399,
0.374218431443826));
#40853=CARTESIAN_POINT('Ctrl Pts',(0.0987296133019425,-0.11860751496485,
0.376853772510332));
#40854=CARTESIAN_POINT('Ctrl Pts',(0.124302447370845,-0.0776931509080149,
0.379489113576838));
#40855=CARTESIAN_POINT('Ctrl Pts',(0.149875281439748,-0.0367787868511801,
0.382124454643343));
#40856=CARTESIAN_POINT('Ctrl Pts',(0.153268843097537,0.0179983578259404,
0.384759795709849));
#40857=CARTESIAN_POINT('Ctrl Pts',(0.132941641804014,0.0617563275693305,
0.387395136776355));
#40858=CARTESIAN_POINT('Ctrl Pts',(0.112614440510491,0.10551429731272,0.39003047784286));
#40859=CARTESIAN_POINT('Ctrl Pts',(0.0685664762656556,0.13825309212238,
0.392665818909367));
#40860=CARTESIAN_POINT('Ctrl Pts',(0.0208060845723004,0.145101450596359,
0.395301159975872));
#40861=CARTESIAN_POINT('Ctrl Pts',(-0.0269543071210555,0.151949809070337,
0.397936501042378));
#40862=CARTESIAN_POINT('Ctrl Pts',(-0.0784271262629304,0.132907731208634,
0.400571842108884));
#40863=CARTESIAN_POINT('Ctrl Pts',(-0.110231373247062,0.0966248853684404,
0.40320718317539));
#40864=CARTESIAN_POINT('Ctrl Pts',(-0.133271130208243,0.0703407243117375,
0.405116287255496));
#40865=CARTESIAN_POINT('Ctrl Pts',(-0.145989017153952,0.0350087805988431,
0.407025391335602));
#40866=CARTESIAN_POINT('Ctrl Pts',(-0.146289342453438,-0.000128032530387096,
0.408934495415709));
#40867=CARTESIAN_POINT('Origin',(0.,0.,0.));
#40868=CARTESIAN_POINT('',(-0.146544022497492,6.84377374728824E-5,0.466065504584291));
#40869=CARTESIAN_POINT('',(-0.146570300119817,4.22437972465385E-5,0.458934495415709));
#40870=CARTESIAN_POINT('',(-0.14635,-1.79227059055215E-17,0.));
#40871=CARTESIAN_POINT('Ctrl Pts',(-0.146544022497492,6.84377374728824E-5,
0.466065504584291));
#40872=CARTESIAN_POINT('Ctrl Pts',(-0.146567170791634,0.00404048499144927,
0.465848716318434));
#40873=CARTESIAN_POINT('Ctrl Pts',(-0.146419528859516,0.00801078566506452,
0.465631928052577));
#40874=CARTESIAN_POINT('Ctrl Pts',(-0.146095506097533,0.0119666390378655,
0.46541513978672));
#40875=CARTESIAN_POINT('Ctrl Pts',(-0.142159486684863,0.0600197930006592,
0.462781735831918));
#40876=CARTESIAN_POINT('Ctrl Pts',(-0.112197024986195,0.105941128890497,
0.460148331877115));
#40877=CARTESIAN_POINT('Ctrl Pts',(-0.0697999311245908,0.128899445176305,
0.457514927922313));
#40878=CARTESIAN_POINT('Ctrl Pts',(-0.0274028372629858,0.151857761462114,
0.454881523967511));
#40879=CARTESIAN_POINT('Ctrl Pts',(0.0274288887615551,0.151853058143892,
0.452248120012709));
#40880=CARTESIAN_POINT('Ctrl Pts',(0.0698220433938502,0.12888746877825,
0.449614716057906));
#40881=CARTESIAN_POINT('Ctrl Pts',(0.112215198026145,0.105921879412608,
0.446981312103104));
#40882=CARTESIAN_POINT('Ctrl Pts',(0.142169781266193,0.0599954039995453,
0.444347908148302));
#40883=CARTESIAN_POINT('Ctrl Pts',(0.146097556879977,0.0119415755015296,
0.441714504193499));
#40884=CARTESIAN_POINT('Ctrl Pts',(0.150025332493762,-0.036112252996486,
0.439081100238697));
#40885=CARTESIAN_POINT('Ctrl Pts',(0.127926300481281,-0.0862934345794555,
0.436447696283895));
#40886=CARTESIAN_POINT('Ctrl Pts',(0.0898251994650805,-0.11583838264071,
0.433814292329093));
#40887=CARTESIAN_POINT('Ctrl Pts',(0.0517240984488793,-0.145383330701964,
0.431180888374291));
#40888=CARTESIAN_POINT('Ctrl Pts',(-0.00237907157104229,-0.154292045241502,
0.428547484419488));
#40889=CARTESIAN_POINT('Ctrl Pts',(-0.0479416004074503,-0.138523284332019,
0.425914080464686));
#40890=CARTESIAN_POINT('Ctrl Pts',(-0.0935041292438574,-0.122754523422536,
0.423280676509884));
#40891=CARTESIAN_POINT('Ctrl Pts',(-0.130526016896751,-0.0823082870640309,
0.420647272555081));
#40892=CARTESIAN_POINT('Ctrl Pts',(-0.142213100308499,-0.0355321186027758,
0.418013868600279));
#40893=CARTESIAN_POINT('Ctrl Pts',(-0.145095389184054,-0.0239960984301615,
0.417364413928283));
#40894=CARTESIAN_POINT('Ctrl Pts',(-0.146436757404375,-0.0120750773303437,
0.416714959256287));
#40895=CARTESIAN_POINT('Ctrl Pts',(-0.146330070388523,-0.000130413829425732,
0.416065504584291));
#40896=CARTESIAN_POINT('Ctrl Pts',(-0.146289342453438,-0.000128032530387096,
0.408934495415709));
#40897=CARTESIAN_POINT('Ctrl Pts',(-0.146403588367378,-0.0134943301275472,
0.409660732402108));
#40898=CARTESIAN_POINT('Ctrl Pts',(-0.144720893191604,-0.0268323904448261,
0.410386969388508));
#40899=CARTESIAN_POINT('Ctrl Pts',(-0.141125892037436,-0.0396334040556115,
0.411113206374907));
#40900=CARTESIAN_POINT('Ctrl Pts',(-0.128080489017291,-0.0860852338207874,
0.413748547441413));
#40901=CARTESIAN_POINT('Ctrl Pts',(-0.0898540081506159,-0.125465279532456,
0.416383888507919));
#40902=CARTESIAN_POINT('Ctrl Pts',(-0.0438104358868217,-0.139885559754408,
0.419019229574425));
#40903=CARTESIAN_POINT('Ctrl Pts',(0.00223313637697255,-0.15430583997636,
0.42165457064093));
#40904=CARTESIAN_POINT('Ctrl Pts',(0.0560938000378854,-0.143766354708596,
0.424289911707436));
#40905=CARTESIAN_POINT('Ctrl Pts',(0.0933059016336915,-0.11305455692152,
0.426925252773942));
#40906=CARTESIAN_POINT('Ctrl Pts',(0.130518003229497,-0.082342759134444,
0.429560593840448));
#40907=CARTESIAN_POINT('Ctrl Pts',(0.151081542760197,-0.0314586488280562,
0.432195934906954));
#40908=CARTESIAN_POINT('Ctrl Pts',(0.145655743526821,0.0164841893354265,
0.434831275973459));
#40909=CARTESIAN_POINT('Ctrl Pts',(0.140229944293446,0.06442702749891,0.437466617039965));
#40910=CARTESIAN_POINT('Ctrl Pts',(0.108814806295994,0.109428593519488,
0.440101958106471));
#40911=CARTESIAN_POINT('Ctrl Pts',(0.0656803334199076,0.131047388078691,
0.442737299172977));
#40912=CARTESIAN_POINT('Ctrl Pts',(0.022545860543821,0.152666182637894,
0.445372640239483));
#40913=CARTESIAN_POINT('Ctrl Pts',(-0.032307947210901,0.150902205735721,
0.448007981305989));
#40914=CARTESIAN_POINT('Ctrl Pts',(-0.0739643108743681,0.126556725768634,
0.450643322372494));
#40915=CARTESIAN_POINT('Ctrl Pts',(-0.115620674537836,0.102211245801546,
0.453278663439));
#40916=CARTESIAN_POINT('Ctrl Pts',(-0.144079594110048,0.0552842627695439,
0.455914004505506));
#40917=CARTESIAN_POINT('Ctrl Pts',(-0.14641389757273,0.0070918768996262,
0.458549345572012));
#40918=CARTESIAN_POINT('Ctrl Pts',(-0.146527615505388,0.00474413652285832,
0.458677728853244));
#40919=CARTESIAN_POINT('Ctrl Pts',(-0.146579333222338,0.00239339303023303,
0.458806112134477));
#40920=CARTESIAN_POINT('Ctrl Pts',(-0.146570300119817,4.22437972465385E-5,
0.458934495415709));
#40921=CARTESIAN_POINT('Origin',(0.,0.,0.));
#40922=CARTESIAN_POINT('',(-0.146145057762853,6.62388175271394E-5,0.516065504584291));
#40923=CARTESIAN_POINT('',(-0.146174937959923,9.05479403153491E-5,0.508934495415709));
#40924=CARTESIAN_POINT('',(-0.14635,-1.79227059055215E-17,0.));
#40925=CARTESIAN_POINT('Ctrl Pts',(-0.146145057762853,6.62388175271395E-5,
0.516065504584291));
#40926=CARTESIAN_POINT('Ctrl Pts',(-0.146227515408595,0.0200490060336265,
0.514982473380581));
#40927=CARTESIAN_POINT('Ctrl Pts',(-0.142408399519226,0.0400016020167204,
0.513899442176871));
#40928=CARTESIAN_POINT('Ctrl Pts',(-0.134535488644935,0.0582005124275171,
0.512816410973161));
#40929=CARTESIAN_POINT('Ctrl Pts',(-0.115392407114926,0.102451391335448,
0.510183007018359));
#40930=CARTESIAN_POINT('Ctrl Pts',(-0.0722822630505052,0.136334037036404,
0.507549603063556));
#40931=CARTESIAN_POINT('Ctrl Pts',(-0.0247610227936349,0.144478334368756,
0.504916199108754));
#40932=CARTESIAN_POINT('Ctrl Pts',(0.0227602174632348,0.152622631701108,
0.502282795153951));
#40933=CARTESIAN_POINT('Ctrl Pts',(0.0746925539125539,0.135028580664858,
0.49964939119915));
#40934=CARTESIAN_POINT('Ctrl Pts',(0.107478027152826,0.0996773345906346,
0.497015987244347));
#40935=CARTESIAN_POINT('Ctrl Pts',(0.140263500393099,0.06432608851641,0.494382583289545));
#40936=CARTESIAN_POINT('Ctrl Pts',(0.153902110424324,0.0112176474042102,
0.491749179334742));
#40937=CARTESIAN_POINT('Ctrl Pts',(0.142207002516364,-0.0355565153954619,
0.48911577537994));
#40938=CARTESIAN_POINT('Ctrl Pts',(0.130511894608405,-0.0823306781951331,
0.486482371425138));
#40939=CARTESIAN_POINT('Ctrl Pts',(0.0934830687612624,-0.122770562682277,
0.483848967470336));
#40940=CARTESIAN_POINT('Ctrl Pts',(0.0479178353914133,-0.138531506897017,
0.481215563515534));
#40941=CARTESIAN_POINT('Ctrl Pts',(0.00235260202156486,-0.154292451111757,
0.478582159560731));
#40942=CARTESIAN_POINT('Ctrl Pts',(-0.0517490388709899,-0.145374455054093,
0.475948755605929));
#40943=CARTESIAN_POINT('Ctrl Pts',(-0.0898450707539318,-0.115822971007387,
0.473315351651126));
#40944=CARTESIAN_POINT('Ctrl Pts',(-0.124804943950367,-0.0887042375336795,
0.470898735962181));
#40945=CARTESIAN_POINT('Ctrl Pts',(-0.146285980252562,-0.044209381789552,
0.468482120273236));
#40946=CARTESIAN_POINT('Ctrl Pts',(-0.146544022497492,6.84377374728824E-5,
0.466065504584291));
#40947=CARTESIAN_POINT('Ctrl Pts',(-0.146570300119817,4.22437972465385E-5,
0.458934495415709));
#40948=CARTESIAN_POINT('Ctrl Pts',(-0.14639390949893,-0.0458689668946884,
0.461441453200982));
#40949=CARTESIAN_POINT('Ctrl Pts',(-0.123052682342738,-0.0919348900534666,
0.463948410986256));
#40950=CARTESIAN_POINT('Ctrl Pts',(-0.0858494648887911,-0.118815796503266,
0.466455368771529));
#40951=CARTESIAN_POINT('Ctrl Pts',(-0.0467410413890165,-0.147073295328412,
0.469090709838035));
#40952=CARTESIAN_POINT('Ctrl Pts',(0.00768549296368549,-0.154130504270872,
0.471726050904541));
#40953=CARTESIAN_POINT('Ctrl Pts',(0.0527074437553312,-0.136781758627296,
0.474361391971047));
#40954=CARTESIAN_POINT('Ctrl Pts',(0.0977293945469769,-0.11943301298372,
0.476996733037553));
#40955=CARTESIAN_POINT('Ctrl Pts',(0.133346761777566,-0.0776783127541087,
0.479632074104058));
#40956=CARTESIAN_POINT('Ctrl Pts',(0.143380722078222,-0.0304843018080604,
0.482267415170564));
#40957=CARTESIAN_POINT('Ctrl Pts',(0.153414682378878,0.0167097091379873,
0.48490275623707));
#40958=CARTESIAN_POINT('Ctrl Pts',(0.137865235749601,0.0693430308004717,
0.487538097303576));
#40959=CARTESIAN_POINT('Ctrl Pts',(0.103795558670285,0.103507517218417,
0.490173438370082));
#40960=CARTESIAN_POINT('Ctrl Pts',(0.0697258815909678,0.137672003636362,
0.492808779436588));
#40961=CARTESIAN_POINT('Ctrl Pts',(0.0171359740616113,0.153367654809767,
0.495444120503093));
#40962=CARTESIAN_POINT('Ctrl Pts',(-0.0300857383810333,0.143464882345699,
0.498079461569599));
#40963=CARTESIAN_POINT('Ctrl Pts',(-0.0773074508236773,0.133562109881631,
0.500714802636104));
#40964=CARTESIAN_POINT('Ctrl Pts',(-0.11916096817961,0.09806091378009,0.503350143702611));
#40965=CARTESIAN_POINT('Ctrl Pts',(-0.136634759914189,0.0530873478673518,
0.505985484769117));
#40966=CARTESIAN_POINT('Ctrl Pts',(-0.143152625668081,0.0363118437555022,
0.506968488317981));
#40967=CARTESIAN_POINT('Ctrl Pts',(-0.146278417362408,0.0182184011065993,
0.507951491866845));
#40968=CARTESIAN_POINT('Ctrl Pts',(-0.146174937959923,9.05479403153491E-5,
0.508934495415709));
#40969=CARTESIAN_POINT('Origin',(0.,0.,0.));
#40970=CARTESIAN_POINT('',(-0.146311419053965,-0.000129619860865307,0.566065504584291));
#40971=CARTESIAN_POINT('',(-0.146253314944083,-0.00012165943743628,0.558934495415709));
#40972=CARTESIAN_POINT('',(-0.14635,-1.79227059055215E-17,0.));
#40973=CARTESIAN_POINT('Ctrl Pts',(-0.146311419053965,-0.000129619860865307,
0.566065504584291));
#40974=CARTESIAN_POINT('Ctrl Pts',(-0.145996667082224,0.0357327735863427,
0.564116230442728));
#40975=CARTESIAN_POINT('Ctrl Pts',(-0.132683527872108,0.0718042758553121,
0.562166956301165));
#40976=CARTESIAN_POINT('Ctrl Pts',(-0.10875495194318,0.0982825405633859,
0.560217682159602));
#40977=CARTESIAN_POINT('Ctrl Pts',(-0.0764282488179375,0.134053787671104,
0.557584278204799));
#40978=CARTESIAN_POINT('Ctrl Pts',(-0.0247272024587828,0.152316317789357,
0.554950874249997));
#40979=CARTESIAN_POINT('Ctrl Pts',(0.022895147382597,0.144785736790908,
0.552317470295194));
#40980=CARTESIAN_POINT('Ctrl Pts',(0.0705174972239762,0.13725515579246,
0.549684066340392));
#40981=CARTESIAN_POINT('Ctrl Pts',(0.11406115054758,0.103931463677311,0.54705066238559));
#40982=CARTESIAN_POINT('Ctrl Pts',(0.133773489094236,0.0599312186369601,
0.544417258430788));
#40983=CARTESIAN_POINT('Ctrl Pts',(0.153485827640893,0.0159309735966095,
0.541783854475986));
#40984=CARTESIAN_POINT('Ctrl Pts',(0.149366851410602,-0.038745824368944,
0.539150450521183));
#40985=CARTESIAN_POINT('Ctrl Pts',(0.123285043153097,-0.0792962514025479,
0.536517046566381));
#40986=CARTESIAN_POINT('Ctrl Pts',(0.097203234895591,-0.119846678436152,
0.533883642611579));
#40987=CARTESIAN_POINT('Ctrl Pts',(0.0491585946108714,-0.146270734537808,
0.531250238656777));
#40988=CARTESIAN_POINT('Ctrl Pts',(0.000945514053129371,-0.146581729267096,
0.528616834701974));
#40989=CARTESIAN_POINT('Ctrl Pts',(-0.0472675665046126,-0.146892723996384,
0.525983430747172));
#40990=CARTESIAN_POINT('Ctrl Pts',(-0.0956490873353763,-0.121090657353305,
0.523350026792369));
#40991=CARTESIAN_POINT('Ctrl Pts',(-0.122251838252959,-0.0808800679743115,
0.520716622837567));
#40992=CARTESIAN_POINT('Ctrl Pts',(-0.137913765110592,-0.057206752695483,
0.519166250086475));
#40993=CARTESIAN_POINT('Ctrl Pts',(-0.146027018608819,-0.0285393430688772,
0.517615877335383));
#40994=CARTESIAN_POINT('Ctrl Pts',(-0.146145057762853,6.62388175271395E-5,
0.516065504584291));
#40995=CARTESIAN_POINT('Ctrl Pts',(-0.146174937959923,9.05479403153491E-5,
0.508934495415709));
#40996=CARTESIAN_POINT('Ctrl Pts',(-0.146000998710948,-0.0303806868131737,
0.510586832933351));
#40997=CARTESIAN_POINT('Ctrl Pts',(-0.136702921110135,-0.060949146702594,
0.512239170450992));
#40998=CARTESIAN_POINT('Ctrl Pts',(-0.119053907816366,-0.0855189520167866,
0.513891507968634));
#40999=CARTESIAN_POINT('Ctrl Pts',(-0.0909051978707368,-0.124705750264253,
0.51652684903514));
#41000=CARTESIAN_POINT('Ctrl Pts',(-0.041513711866252,-0.148633411035251,
0.519162190101645));
#41001=CARTESIAN_POINT('Ctrl Pts',(0.00668497479873183,-0.146433040097983,
0.521797531168151));
#41002=CARTESIAN_POINT('Ctrl Pts',(0.0548836614637157,-0.144232669160716,
0.524432872234657));
#41003=CARTESIAN_POINT('Ctrl Pts',(0.101889548789197,-0.115904266515181,
0.527068213301163));
#41004=CARTESIAN_POINT('Ctrl Pts',(0.126350695083001,-0.0743157182057725,
0.529703554367669));
#41005=CARTESIAN_POINT('Ctrl Pts',(0.150811841376805,-0.0327271698963649,
0.532338895434175));
#41006=CARTESIAN_POINT('Ctrl Pts',(0.152728246638932,0.0221215240769157,
0.53497423650068));
#41007=CARTESIAN_POINT('Ctrl Pts',(0.131229403455446,0.0653159076268943,
0.537609577567186));
#41008=CARTESIAN_POINT('Ctrl Pts',(0.10973056027196,0.108510291176874,0.540244918633692));
#41009=CARTESIAN_POINT('Ctrl Pts',(0.0648164686428582,0.140050364303552,
0.542880259700198));
#41010=CARTESIAN_POINT('Ctrl Pts',(0.0168888935424139,0.145609372621787,
0.545515600766704));
#41011=CARTESIAN_POINT('Ctrl Pts',(-0.0310386815580289,0.151168380940021,
0.54815094183321));
#41012=CARTESIAN_POINT('Ctrl Pts',(-0.0819797401298146,0.130746324449814,
0.550786282899715));
#41013=CARTESIAN_POINT('Ctrl Pts',(-0.112794829345876,0.093619712631646,
0.553421623966221));
#41014=CARTESIAN_POINT('Ctrl Pts',(-0.134282196795419,0.0677313192961588,
0.555259247782717));
#41015=CARTESIAN_POINT('Ctrl Pts',(-0.145983763479016,0.0337207109540846,
0.557096871599213));
#41016=CARTESIAN_POINT('Ctrl Pts',(-0.146253314944083,-0.00012165943743628,
0.558934495415709));
#41017=CARTESIAN_POINT('Origin',(0.,0.,0.));
#41018=CARTESIAN_POINT('',(-0.146555285157174,5.84873774584615E-5,0.616065504584291));
#41019=CARTESIAN_POINT('',(-0.146582406651585,1.90495679610238E-5,0.608934495415709));
#41020=CARTESIAN_POINT('',(-0.14635,-1.79227059055215E-17,0.));
#41021=CARTESIAN_POINT('Ctrl Pts',(-0.146555285157174,5.84873774584615E-5,
0.616065504584291));
#41022=CARTESIAN_POINT('Ctrl Pts',(-0.146572323774182,0.00339452825839206,
0.615883391459677));
#41023=CARTESIAN_POINT('Ctrl Pts',(-0.146468182740347,0.00672948697362643,
0.615701278335063));
#41024=CARTESIAN_POINT('Ctrl Pts',(-0.146239449746585,0.0100558783590757,
0.615519165210449));
#41025=CARTESIAN_POINT('Ctrl Pts',(-0.142931910151921,0.0581563776955572,
0.612885761255647));
#41026=CARTESIAN_POINT('Ctrl Pts',(-0.113572285175357,0.10446545479915,
0.610252357300844));
#41027=CARTESIAN_POINT('Ctrl Pts',(-0.0714789213525946,0.127976017886268,
0.607618953346042));
#41028=CARTESIAN_POINT('Ctrl Pts',(-0.0293855575298321,0.151486580973386,
0.60498554939124));
#41029=CARTESIAN_POINT('Ctrl Pts',(0.0254415451391293,0.15219863004403,
0.602352145436437));
#41030=CARTESIAN_POINT('Ctrl Pts',(0.068131280382423,0.129789159736893,
0.599718741481635));
#41031=CARTESIAN_POINT('Ctrl Pts',(0.110821015625717,0.107379689429756,
0.597085337526833));
#41032=CARTESIAN_POINT('Ctrl Pts',(0.141373383443343,0.0618486997448399,
0.594451933572031));
#41033=CARTESIAN_POINT('Ctrl Pts',(0.145928975807906,0.0138503202638931,
0.591818529617228));
#41034=CARTESIAN_POINT('Ctrl Pts',(0.150484568172469,-0.0341480592170517,
0.589185125662426));
#41035=CARTESIAN_POINT('Ctrl Pts',(0.129043385083969,-0.0846138284940251,
0.586551721707624));
#41036=CARTESIAN_POINT('Ctrl Pts',(0.0913317465051492,-0.114654304027699,
0.583918317752822));
#41037=CARTESIAN_POINT('Ctrl Pts',(0.0536201079263286,-0.144694779561374,
0.58128491379802));
#41038=CARTESIAN_POINT('Ctrl Pts',(-0.000361986142813277,-0.154309961351749,
0.578651509843217));
#41039=CARTESIAN_POINT('Ctrl Pts',(-0.0461267489505717,-0.139138134179699,
0.576018105888415));
#41040=CARTESIAN_POINT('Ctrl Pts',(-0.0918915117583307,-0.123966307007649,
0.573384701933613));
#41041=CARTESIAN_POINT('Ctrl Pts',(-0.129438943304707,-0.0840074708731724,
0.57075129797881));
#41042=CARTESIAN_POINT('Ctrl Pts',(-0.141736479132229,-0.0373880707573429,
0.568117894024008));
#41043=CARTESIAN_POINT('Ctrl Pts',(-0.14493124569041,-0.0252768557512302,
0.567433764210769));
#41044=CARTESIAN_POINT('Ctrl Pts',(-0.146421886434131,-0.0127161165512012,
0.56674963439753));
#41045=CARTESIAN_POINT('Ctrl Pts',(-0.146311419053965,-0.000129619860865307,
0.566065504584291));
#41046=CARTESIAN_POINT('Ctrl Pts',(-0.146253314944083,-0.00012165943743628,
0.558934495415709));
#41047=CARTESIAN_POINT('Ctrl Pts',(-0.146370327932007,-0.0148127199255511,
0.559732212665719));
#41048=CARTESIAN_POINT('Ctrl Pts',(-0.144333034185812,-0.0294720768038573,
0.560529929915728));
#41049=CARTESIAN_POINT('Ctrl Pts',(-0.140006765979157,-0.0434215338335114,
0.561327647165738));
#41050=CARTESIAN_POINT('Ctrl Pts',(-0.125714493536039,-0.089505001334368,
0.563962988232244));
#41051=CARTESIAN_POINT('Ctrl Pts',(-0.0864408287894652,-0.127840769189951,
0.56659832929875));
#41052=CARTESIAN_POINT('Ctrl Pts',(-0.0400254307145004,-0.141015208458223,
0.569233670365256));
#41053=CARTESIAN_POINT('Ctrl Pts',(0.00638996736046498,-0.154189647726494,
0.571869011431762));
#41054=CARTESIAN_POINT('Ctrl Pts',(0.0599470987638218,-0.142202758407454,
0.574504352498268));
#41055=CARTESIAN_POINT('Ctrl Pts',(0.0963181864448715,-0.110499461900809,
0.577139693564773));
#41056=CARTESIAN_POINT('Ctrl Pts',(0.132689274125921,-0.0787961653941636,
0.579775034631279));
#41057=CARTESIAN_POINT('Ctrl Pts',(0.151874318084663,-0.0273764616999143,
0.582410375697785));
#41058=CARTESIAN_POINT('Ctrl Pts',(0.145158709082207,0.0204027767224063,
0.585045716764291));
#41059=CARTESIAN_POINT('Ctrl Pts',(0.138443100079752,0.0681820151447277,
0.587681057830797));
#41060=CARTESIAN_POINT('Ctrl Pts',(0.1058268381161,0.112320788295119,0.590316398897302));
#41061=CARTESIAN_POINT('Ctrl Pts',(0.0621255253059884,0.132769511657806,
0.592951739963808));
#41062=CARTESIAN_POINT('Ctrl Pts',(0.0184242124958778,0.153218235020492,
0.595587081030314));
#41063=CARTESIAN_POINT('Ctrl Pts',(-0.0363621511606923,0.149976908595474,
0.59822242209682));
#41064=CARTESIAN_POINT('Ctrl Pts',(-0.0773474224829438,0.124517871631514,
0.600857763163326));
#41065=CARTESIAN_POINT('Ctrl Pts',(-0.118332693805197,0.0990588346675542,
0.603493104229832));
#41066=CARTESIAN_POINT('Ctrl Pts',(-0.145516872793131,0.0513820871646532,
0.606128445296338));
#41067=CARTESIAN_POINT('Ctrl Pts',(-0.146551825250685,0.00314430216262847,
0.608763786362843));
#41068=CARTESIAN_POINT('Ctrl Pts',(-0.146574172232136,0.00210273848614761,
0.608820689380465));
#41069=CARTESIAN_POINT('Ctrl Pts',(-0.146584327751734,0.00106091323912811,
0.608877592398087));
#41070=CARTESIAN_POINT('Ctrl Pts',(-0.146582406651585,1.90495679610238E-5,
0.608934495415709));
#41071=CARTESIAN_POINT('Origin',(0.,0.,0.));
#41072=CARTESIAN_POINT('',(-0.146154441698478,7.49371236435786E-5,0.666065504584291));
#41073=CARTESIAN_POINT('',(-0.14620212788816,0.000104817362006062,0.658934495415709));
#41074=CARTESIAN_POINT('',(-0.14635,-1.79227059055215E-17,0.));
#41075=CARTESIAN_POINT('Ctrl Pts',(-0.146154441698478,7.49371236435786E-5,
0.666065504584291));
#41076=CARTESIAN_POINT('Ctrl Pts',(-0.146245091243546,0.019414808211501,
0.665017148521823));
#41077=CARTESIAN_POINT('Ctrl Pts',(-0.142674700046404,0.0387225584902945,
0.663968792459356));
#41078=CARTESIAN_POINT('Ctrl Pts',(-0.135284782149148,0.0564369123056677,
0.662920436396889));
#41079=CARTESIAN_POINT('Ctrl Pts',(-0.116721776970831,0.100934245858918,
0.660287032442087));
#41080=CARTESIAN_POINT('Ctrl Pts',(-0.074058225042023,0.13537752586737,
0.657653628487285));
#41081=CARTESIAN_POINT('Ctrl Pts',(-0.0266475060286977,0.144142317777245,
0.655020224532483));
#41082=CARTESIAN_POINT('Ctrl Pts',(0.020763212984627,0.15290710968712,0.652386820577681));
#41083=CARTESIAN_POINT('Ctrl Pts',(0.0729210990824686,0.13599341349842,
0.649753416622878));
#41084=CARTESIAN_POINT('Ctrl Pts',(0.106165877238123,0.101073754565802,
0.647120012668076));
#41085=CARTESIAN_POINT('Ctrl Pts',(0.139410655393777,0.0661540956331838,
0.644486608713273));
#41086=CARTESIAN_POINT('Ctrl Pts',(0.153742325607243,0.0132284739566488,
0.641853204758471));
#41087=CARTESIAN_POINT('Ctrl Pts',(0.142659641677727,-0.0336945691193152,
0.639219800803669));
#41088=CARTESIAN_POINT('Ctrl Pts',(0.13157695774821,-0.0806176121952798,
0.636586396848867));
#41089=CARTESIAN_POINT('Ctrl Pts',(0.09507991967571,-0.121538076670673,
0.633952992894065));
#41090=CARTESIAN_POINT('Ctrl Pts',(0.049724604077795,-0.137893296070049,
0.631319588939263));
#41091=CARTESIAN_POINT('Ctrl Pts',(0.00436928847988189,-0.154248515469425,
0.62868618498446));
#41092=CARTESIAN_POINT('Ctrl Pts',(-0.0498443046434454,-0.146038489792785,
0.626052781029658));
#41093=CARTESIAN_POINT('Ctrl Pts',(-0.0883233740987275,-0.116987516169781,
0.623419377074855));
#41094=CARTESIAN_POINT('Ctrl Pts',(-0.1241414224228,-0.0899455634453427,
0.620968086244667));
#41095=CARTESIAN_POINT('Ctrl Pts',(-0.146325940865162,-0.0448455053352938,
0.618516795414479));
#41096=CARTESIAN_POINT('Ctrl Pts',(-0.146555285157174,5.84873774584615E-5,
0.616065504584291));
#41097=CARTESIAN_POINT('Ctrl Pts',(-0.146582406651585,1.90495679610238E-5,
0.608934495415709));
#41098=CARTESIAN_POINT('Ctrl Pts',(-0.146495356123754,-0.0471907653725723,
0.611512933464593));
#41099=CARTESIAN_POINT('Ctrl Pts',(-0.121611930441545,-0.0944794748712001,
0.614091371513477));
#41100=CARTESIAN_POINT('Ctrl Pts',(-0.0826169041730041,-0.121085801253764,
0.616669809562361));
#41101=CARTESIAN_POINT('Ctrl Pts',(-0.042761304710591,-0.148279297166989,
0.619305150628866));
#41102=CARTESIAN_POINT('Ctrl Pts',(0.0118356201414113,-0.153867466492291,
0.621940491695373));
#41103=CARTESIAN_POINT('Ctrl Pts',(0.0563737778341691,-0.135311940689286,
0.624575832761878));
#41104=CARTESIAN_POINT('Ctrl Pts',(0.100911935526926,-0.116756414886282,
0.627211173828384));
#41105=CARTESIAN_POINT('Ctrl Pts',(0.135391326060439,-0.0740571939549723,
0.62984651489489));
#41106=CARTESIAN_POINT('Ctrl Pts',(0.144150040296483,-0.0266099605959858,
0.632481855961396));
#41107=CARTESIAN_POINT('Ctrl Pts',(0.152908754532526,0.0208372727630014,
0.635117197027901));
#41108=CARTESIAN_POINT('Ctrl Pts',(0.135946792471101,0.0730325185496646,
0.637752538094407));
#41109=CARTESIAN_POINT('Ctrl Pts',(0.100968951224381,0.106266622271745,
0.640387879160913));
#41110=CARTESIAN_POINT('Ctrl Pts',(0.0659911099776614,0.139500725993825,
0.643023220227419));
#41111=CARTESIAN_POINT('Ctrl Pts',(0.0129973895456473,0.153773687651321,
0.645658561293925));
#41112=CARTESIAN_POINT('Ctrl Pts',(-0.0339403566699702,0.14260216095667,
0.648293902360431));
#41113=CARTESIAN_POINT('Ctrl Pts',(-0.0808781028855877,0.131430634262018,
0.650929243426936));
#41114=CARTESIAN_POINT('Ctrl Pts',(-0.121759874884809,0.0948146192152183,
0.653564584493442));
#41115=CARTESIAN_POINT('Ctrl Pts',(-0.138015547484023,0.0493865647021963,
0.656199925559948));
#41116=CARTESIAN_POINT('Ctrl Pts',(-0.143638130564433,0.0336737106740469,
0.657111448845201));
#41117=CARTESIAN_POINT('Ctrl Pts',(-0.146314545676077,0.0169066195134479,
0.658022972130455));
#41118=CARTESIAN_POINT('Ctrl Pts',(-0.14620212788816,0.000104817362006062,
0.658934495415709));
#41119=CARTESIAN_POINT('Origin',(0.,0.,0.));
#41120=CARTESIAN_POINT('',(-0.146293122286189,-0.000127967976324597,0.716065504584291));
#41121=CARTESIAN_POINT('',(-0.146220133725287,-0.000111981377959844,0.708934495415709));
#41122=CARTESIAN_POINT('',(-0.14635,-1.79227059055215E-17,0.));
#41123=CARTESIAN_POINT('Ctrl Pts',(-0.146293122286189,-0.000127967976324597,
0.716065504584291));
#41124=CARTESIAN_POINT('Ctrl Pts',(-0.145991055868361,0.035107698155652,
0.714150905583971));
#41125=CARTESIAN_POINT('Ctrl Pts',(-0.133191339997662,0.0705402609933279,
0.71223630658365));
#41126=CARTESIAN_POINT('Ctrl Pts',(-0.110030394316881,0.0968525150836482,
0.71032170758333));
#41127=CARTESIAN_POINT('Ctrl Pts',(-0.0781740494934874,0.133043275639576,
0.707688303628528));
#41128=CARTESIAN_POINT('Ctrl Pts',(-0.0267161455114648,0.151980073612578,
0.705054899673726));
#41129=CARTESIAN_POINT('Ctrl Pts',(0.0210005740720494,0.145072648144428,
0.702421495718924));
#41130=CARTESIAN_POINT('Ctrl Pts',(0.0687172936555642,0.138165222676278,
0.699788091764121));
#41131=CARTESIAN_POINT('Ctrl Pts',(0.112692828840571,0.105413573766977,
0.697154687809319));
#41132=CARTESIAN_POINT('Ctrl Pts',(0.132978647675338,0.0616747648126076,
0.694521283854517));
#41133=CARTESIAN_POINT('Ctrl Pts',(0.153264466510106,0.0179359558582386,
0.691887879899714));
#41134=CARTESIAN_POINT('Ctrl Pts',(0.149860568994636,-0.0367900131411976,
0.689254475944912));
#41135=CARTESIAN_POINT('Ctrl Pts',(0.124311058190535,-0.0776779129690893,
0.68662107199011));
#41136=CARTESIAN_POINT('Ctrl Pts',(0.0987615473864338,-0.11856581279698,
0.683987668035308));
#41137=CARTESIAN_POINT('Ctrl Pts',(0.0510664232937013,-0.145615643453328,
0.681354264080505));
#41138=CARTESIAN_POINT('Ctrl Pts',(0.00286152734998743,-0.146556845670501,
0.678720860125703));
#41139=CARTESIAN_POINT('Ctrl Pts',(-0.0453433685937279,-0.147498047887674,
0.6760874561709));
#41140=CARTESIAN_POINT('Ctrl Pts',(-0.094058036388424,-0.122330621665673,
0.673454052216099));
#41141=CARTESIAN_POINT('Ctrl Pts',(-0.121184141071859,-0.082471215005648,
0.670820648261296));
#41142=CARTESIAN_POINT('Ctrl Pts',(-0.137511364617388,-0.0584798070786627,
0.669235600368961));
#41143=CARTESIAN_POINT('Ctrl Pts',(-0.146017385334238,-0.0291657216594994,
0.667650552476626));
#41144=CARTESIAN_POINT('Ctrl Pts',(-0.146154441698478,7.49371236435786E-5,
0.666065504584291));
#41145=CARTESIAN_POINT('Ctrl Pts',(-0.14620212788816,0.000104817362006062,
0.658934495415709));
#41146=CARTESIAN_POINT('Ctrl Pts',(-0.145989530157664,-0.0316697360413935,
0.660658313196961));
#41147=CARTESIAN_POINT('Ctrl Pts',(-0.135802925380645,-0.0635684301444077,
0.662382130978214));
#41148=CARTESIAN_POINT('Ctrl Pts',(-0.116706447513916,-0.088695711446933,
0.664105948759466));
#41149=CARTESIAN_POINT('Ctrl Pts',(-0.0875121017453893,-0.127109839103795,
0.666741289825971));
#41150=CARTESIAN_POINT('Ctrl Pts',(-0.0374938370091297,-0.149698000438276,
0.669376630892477));
#41151=CARTESIAN_POINT('Ctrl Pts',(0.0106280634930049,-0.146199755084551,
0.672011971958983));
#41152=CARTESIAN_POINT('Ctrl Pts',(0.0587499639951401,-0.142701509730827,
0.674647313025488));
#41153=CARTESIAN_POINT('Ctrl Pts',(0.104975500263151,-0.113116857688896,
0.677282654091995));
#41154=CARTESIAN_POINT('Ctrl Pts',(0.128307197060476,-0.0708843233930653,
0.679917995158501));
#41155=CARTESIAN_POINT('Ctrl Pts',(0.1516388938578,-0.0286517890972343,
0.682553336225006));
#41156=CARTESIAN_POINT('Ctrl Pts',(0.152076751184439,0.0262286274524959,
0.685188677291512));
#41157=CARTESIAN_POINT('Ctrl Pts',(0.129421876845612,0.06882806051419,0.687824018358017));
#41158=CARTESIAN_POINT('Ctrl Pts',(0.106767002506784,0.111427493575885,
0.690459359424523));
#41159=CARTESIAN_POINT('Ctrl Pts',(0.0610193965024891,0.141745943149541,
0.69309470049103));
#41160=CARTESIAN_POINT('Ctrl Pts',(0.0129594391535466,0.146011564806377,
0.695730041557535));
#41161=CARTESIAN_POINT('Ctrl Pts',(-0.0351005181953946,0.150277186463213,
0.698365382624041));
#41162=CARTESIAN_POINT('Ctrl Pts',(-0.0854728268889839,0.128489980203229,
0.701000723690547));
#41163=CARTESIAN_POINT('Ctrl Pts',(-0.115276382892,0.0905465607729482,0.703636064757053));
#41164=CARTESIAN_POINT('Ctrl Pts',(-0.135250024617843,0.0651177741718751,
0.705402208309938));
#41165=CARTESIAN_POINT('Ctrl Pts',(-0.145985488943994,0.0324326426859288,
0.707168351862824));
#41166=CARTESIAN_POINT('Ctrl Pts',(-0.146220133725287,-0.000111981377959844,
0.708934495415709));
#41167=CARTESIAN_POINT('Origin',(0.,0.,0.));
#41168=CARTESIAN_POINT('',(-0.146564965442509,4.80374956639621E-5,0.766065504584291));
#41169=CARTESIAN_POINT('',(-0.14658533994215,-4.90005960534454E-6,0.758934495415709));
#41170=CARTESIAN_POINT('',(-0.14635,-1.79227059055215E-17,0.));
#41171=CARTESIAN_POINT('Ctrl Pts',(-0.146564965442509,4.80374956639621E-5,
0.766065504584291));
#41172=CARTESIAN_POINT('Ctrl Pts',(-0.146576599691724,0.00274840678048242,
0.76591806660092));
#41173=CARTESIAN_POINT('Ctrl Pts',(-0.146508366823243,0.00544817658194007,
0.765770628617549));
#41174=CARTESIAN_POINT('Ctrl Pts',(-0.146358404344074,0.00814339894155673,
0.765623190634177));
#41175=CARTESIAN_POINT('Ctrl Pts',(-0.14367991012782,0.0562830238780745,
0.762989786679375));
#41176=CARTESIAN_POINT('Ctrl Pts',(-0.11492813804623,0.102971929623608,
0.760356382724573));
#41177=CARTESIAN_POINT('Ctrl Pts',(-0.0731456970048765,0.127030722191848,
0.757722978769771));
#41178=CARTESIAN_POINT('Ctrl Pts',(-0.031363255963523,0.151089514760089,
0.755089574814969));
#41179=CARTESIAN_POINT('Ctrl Pts',(0.023449854037593,0.152518194151036,
0.752456170860167));
#41180=CARTESIAN_POINT('Ctrl Pts',(0.0664288749466077,0.130668672151013,
0.749822766905364));
#41181=CARTESIAN_POINT('Ctrl Pts',(0.109407895855622,0.108819150150991,
0.747189362950562));
#41182=CARTESIAN_POINT('Ctrl Pts',(0.140552827672535,0.0636914267599971,
0.744555958995759));
#41183=CARTESIAN_POINT('Ctrl Pts',(0.145735458379408,0.0157566983326864,
0.741922555040957));
#41184=CARTESIAN_POINT('Ctrl Pts',(0.150918089086281,-0.0321780300946251,
0.739289151086155));
#41185=CARTESIAN_POINT('Ctrl Pts',(0.130138418683114,-0.0829197635582554,
0.736655747131352));
#41186=CARTESIAN_POINT('Ctrl Pts',(0.0928226866975336,-0.113450633258391,
0.73402234317655));
#41187=CARTESIAN_POINT('Ctrl Pts',(0.0555069547119538,-0.143981502958525,
0.731388939221748));
#41188=CARTESIAN_POINT('Ctrl Pts',(0.00165516114396223,-0.154301508895166,
0.728755535266946));
#41189=CARTESIAN_POINT('Ctrl Pts',(-0.0443040153143291,-0.139729208016517,
0.726122131312144));
#41190=CARTESIAN_POINT('Ctrl Pts',(-0.0902631917726212,-0.125156907137867,
0.723488727357341));
#41191=CARTESIAN_POINT('Ctrl Pts',(-0.128329751121212,-0.0856922994439281,
0.720855323402539));
#41192=CARTESIAN_POINT('Ctrl Pts',(-0.141235637963126,-0.0392376340275311,
0.718221919447737));
#41193=CARTESIAN_POINT('Ctrl Pts',(-0.144758384781757,-0.0265575271266455,
0.717503114493255));
#41194=CARTESIAN_POINT('Ctrl Pts',(-0.146406528193996,-0.0133566238911661,
0.716784309538773));
#41195=CARTESIAN_POINT('Ctrl Pts',(-0.146293122286189,-0.000127967976324597,
0.716065504584291));
#41196=CARTESIAN_POINT('Ctrl Pts',(-0.146220133725287,-0.000111981377959844,
0.708934495415709));
#41197=CARTESIAN_POINT('Ctrl Pts',(-0.146335612821056,-0.016128633179466,
0.709803692929329));
#41198=CARTESIAN_POINT('Ctrl Pts',(-0.143907730109974,-0.0321112532361818,
0.71067289044295));
#41199=CARTESIAN_POINT('Ctrl Pts',(-0.138785978242991,-0.047178134378496,
0.71154208795657));
#41200=CARTESIAN_POINT('Ctrl Pts',(-0.123257214278523,-0.0928597774990785,
0.714177429023076));
#41201=CARTESIAN_POINT('Ctrl Pts',(-0.0829648830371437,-0.130123431139663,
0.716812770089582));
#41202=CARTESIAN_POINT('Ctrl Pts',(-0.0362113622873864,-0.142042463234138,
0.719448111156088));
#41203=CARTESIAN_POINT('Ctrl Pts',(0.0105421584623702,-0.153961495328613,
0.722083452222593));
#41204=CARTESIAN_POINT('Ctrl Pts',(0.063756868720506,-0.140535905876979,
0.724718793289099));
#41205=CARTESIAN_POINT('Ctrl Pts',(0.0992605327204626,-0.107864131039655,
0.727354134355605));
#41206=CARTESIAN_POINT('Ctrl Pts',(0.13476419672042,-0.075192356202331,
0.729989475422111));
#41207=CARTESIAN_POINT('Ctrl Pts',(0.152556814462199,-0.0232743959793195,
0.732624816488617));
#41208=CARTESIAN_POINT('Ctrl Pts',(0.144556272029555,0.024306549251931,
0.735260157555123));
#41209=CARTESIAN_POINT('Ctrl Pts',(0.136555729596912,0.0718874944831808,
0.737895498621628));
#41210=CARTESIAN_POINT('Ctrl Pts',(0.102762026989844,0.115131424722669,
0.740530839688134));
#41211=CARTESIAN_POINT('Ctrl Pts',(0.058525606626993,0.13439522866968,0.74316618075464));
#41212=CARTESIAN_POINT('Ctrl Pts',(0.0142891862641413,0.15365903261669,
0.745801521821146));
#41213=CARTESIAN_POINT('Ctrl Pts',(-0.0403899518544944,0.148942710271224,
0.748436862887652));
#41214=CARTESIAN_POINT('Ctrl Pts',(-0.0806743706113798,0.122388602614794,
0.751072203954158));
#41215=CARTESIAN_POINT('Ctrl Pts',(-0.120735958293688,0.0959813775627587,
0.753692967774675));
#41216=CARTESIAN_POINT('Ctrl Pts',(-0.146561633397375,0.047977288078364,
0.756313731595192));
#41217=CARTESIAN_POINT('Ctrl Pts',(-0.14658533994215,-4.90005960534454E-6,
0.758934495415709));
#41218=CARTESIAN_POINT('Origin',(0.,0.,0.));
#41219=CARTESIAN_POINT('',(-0.146164975321328,8.31911013993853E-5,0.816065504584291));
#41220=CARTESIAN_POINT('',(-0.146233275186053,0.000116309547457056,0.808934495415709));
#41221=CARTESIAN_POINT('',(-0.14635,-1.79227059055215E-17,0.));
#41222=CARTESIAN_POINT('Ctrl Pts',(-0.146164975321328,8.31911013993853E-5,
0.816065504584291));
#41223=CARTESIAN_POINT('Ctrl Pts',(-0.146262710135629,0.0187799830896948,
0.815051823663067));
#41224=CARTESIAN_POINT('Ctrl Pts',(-0.142931951335767,0.037443276248974,
0.814038142741842));
#41225=CARTESIAN_POINT('Ctrl Pts',(-0.136010977838838,0.054663650141277,
0.813024461820618));
#41226=CARTESIAN_POINT('Ctrl Pts',(-0.118031238261729,0.0993998188524282,
0.810391057865816));
#41227=CARTESIAN_POINT('Ctrl Pts',(-0.0758215305972079,0.13439788253602,
0.807757653911014));
#41228=CARTESIAN_POINT('Ctrl Pts',(-0.028529425342275,0.143781679589591,
0.805124249956212));
#41229=CARTESIAN_POINT('Ctrl Pts',(0.0187626799126572,0.153165476643161,
0.80249084600141));
#41230=CARTESIAN_POINT('Ctrl Pts',(0.0711371827580015,0.136935007066712,
0.799857442046606));
#41231=CARTESIAN_POINT('Ctrl Pts',(0.104835580177757,0.102452897995539,
0.797224038091804));
#41232=CARTESIAN_POINT('Ctrl Pts',(0.138533977597513,0.0679707889243652,
0.794590634137002));
#41233=CARTESIAN_POINT('Ctrl Pts',(0.15355626959168,0.0152370403584678,
0.791957230182201));
#41234=CARTESIAN_POINT('Ctrl Pts',(0.143087905965057,-0.0318268624597296,
0.789323826227399));
#41235=CARTESIAN_POINT('Ctrl Pts',(0.132619542338435,-0.0788907652779263,
0.786690422272596));
#41236=CARTESIAN_POINT('Ctrl Pts',(0.096660523091021,-0.120284822348423,
0.784057018317793));
#41237=CARTESIAN_POINT('Ctrl Pts',(0.0515228742830193,-0.137231523355512,
0.781423614362991));
#41238=CARTESIAN_POINT('Ctrl Pts',(0.00638522547501753,-0.1541782243626,
0.778790210408188));
#41239=CARTESIAN_POINT('Ctrl Pts',(-0.0479310528935715,-0.146677569306282,
0.776156806453387));
#41240=CARTESIAN_POINT('Ctrl Pts',(-0.0867865839024083,-0.118132069714372,
0.773523402498585));
#41241=CARTESIAN_POINT('Ctrl Pts',(-0.123466686745614,-0.0911847643100577,
0.771037436527154));
#41242=CARTESIAN_POINT('Ctrl Pts',(-0.146368799251201,-0.045483147880463,
0.768551470555722));
#41243=CARTESIAN_POINT('Ctrl Pts',(-0.146564965442509,4.80374956639621E-5,
0.766065504584291));
#41244=CARTESIAN_POINT('Ctrl Pts',(-0.14658533994215,-4.90005960534454E-6,
0.758934495415709));
#41245=CARTESIAN_POINT('Ctrl Pts',(-0.146609310208618,-0.0485208624767226,
0.761584413728203));
#41246=CARTESIAN_POINT('Ctrl Pts',(-0.120122621218798,-0.0970137112575841,
0.764234332040698));
#41247=CARTESIAN_POINT('Ctrl Pts',(-0.0793243537302287,-0.123267883191947,
0.766884250353192));
#41248=CARTESIAN_POINT('Ctrl Pts',(-0.0387505182093485,-0.149377630477176,
0.769519591419698));
#41249=CARTESIAN_POINT('Ctrl Pts',(0.0159771533787021,-0.153492702582488,
0.772154932486204));
#41250=CARTESIAN_POINT('Ctrl Pts',(0.0599991778729333,-0.13374387011901,
0.77479027355271));
#41251=CARTESIAN_POINT('Ctrl Pts',(0.104021202367166,-0.113995037655531,
0.777425614619216));
#41252=CARTESIAN_POINT('Ctrl Pts',(0.13733757976758,-0.0703823006232647,
0.780060955685721));
#41253=CARTESIAN_POINT('Ctrl Pts',(0.14481468818493,-0.022716297290398,
0.782696296752227));
#41254=CARTESIAN_POINT('Ctrl Pts',(0.152291796602279,0.0249497060424673,
0.785331637818733));
#41255=CARTESIAN_POINT('Ctrl Pts',(0.133929636036564,0.0766689756759309,
0.787966978885239));
#41256=CARTESIAN_POINT('Ctrl Pts',(0.0980690284933123,0.108948564888508,
0.790602319951745));
#41257=CARTESIAN_POINT('Ctrl Pts',(0.0622084209500598,0.141228154101085,
0.793237661018251));
#41258=CARTESIAN_POINT('Ctrl Pts',(0.00884936642926935,0.154068062892775,
0.795873002084756));
#41259=CARTESIAN_POINT('Ctrl Pts',(-0.0377703306973942,0.141635893595607,
0.798508343151262));
#41260=CARTESIAN_POINT('Ctrl Pts',(-0.084390027824057,0.129203724298439,
0.801143684217768));
#41261=CARTESIAN_POINT('Ctrl Pts',(-0.124270367556593,0.0914994769124139,
0.803779025284273));
#41262=CARTESIAN_POINT('Ctrl Pts',(-0.139296118286606,0.0456499204587224,
0.806414366350779));
#41263=CARTESIAN_POINT('Ctrl Pts',(-0.144085736300807,0.0310348862098803,
0.807254409372422));
#41264=CARTESIAN_POINT('Ctrl Pts',(-0.146349920545361,0.0155922205493257,
0.808094452394066));
#41265=CARTESIAN_POINT('Ctrl Pts',(-0.146233275186053,0.000116309547457056,
0.808934495415709));
#41266=CARTESIAN_POINT('Origin',(0.,0.,0.));
#41267=CARTESIAN_POINT('',(-0.146273246343463,-0.000123611542196964,0.866065504584292));
#41268=CARTESIAN_POINT('',(-0.146190615322833,-9.92620605964336E-5,0.858934495415709));
#41269=CARTESIAN_POINT('',(-0.14635,-1.79227059055215E-17,0.));
#41270=CARTESIAN_POINT('Ctrl Pts',(-0.146273246343463,-0.000123611542196964,
0.866065504584292));
#41271=CARTESIAN_POINT('Ctrl Pts',(-0.14598570205562,0.0344841852260994,
0.864185580725214));
#41272=CARTESIAN_POINT('Ctrl Pts',(-0.13368920007778,0.0692748383916789,
0.862305656866136));
#41273=CARTESIAN_POINT('Ctrl Pts',(-0.111287960012964,0.0954050911579531,
0.860425733007059));
#41274=CARTESIAN_POINT('Ctrl Pts',(-0.0799082241293448,0.13200844115132,
0.857792329052257));
#41275=CARTESIAN_POINT('Ctrl Pts',(-0.0287004609307042,0.151617916172533,
0.855158925097454));
#41276=CARTESIAN_POINT('Ctrl Pts',(0.0191028994225217,0.145335216041435,
0.852525521142652));
#41277=CARTESIAN_POINT('Ctrl Pts',(0.0669062597757476,0.139052515910338,
0.84989211718785));
#41278=CARTESIAN_POINT('Ctrl Pts',(0.111305217283559,0.10687764062693,0.847258713233048));
#41279=CARTESIAN_POINT('Ctrl Pts',(0.132160826244895,0.0634075368078452,
0.844625309278246));
#41280=CARTESIAN_POINT('Ctrl Pts',(0.15301643520623,0.0199374329887607,
0.841991905323443));
#41281=CARTESIAN_POINT('Ctrl Pts',(0.15032869562109,-0.0348278993660004,
0.839358501368641));
#41282=CARTESIAN_POINT('Ctrl Pts',(0.12531596597325,-0.076046177073106,
0.836725097413839));
#41283=CARTESIAN_POINT('Ctrl Pts',(0.10030323632541,-0.117264454780212,
0.834091693459036));
#41284=CARTESIAN_POINT('Ctrl Pts',(0.0529655166148703,-0.144935677839662,
0.831458289504234));
#41285=CARTESIAN_POINT('Ctrl Pts',(0.00477698054298851,-0.14650698356075,
0.828824885549432));
#41286=CARTESIAN_POINT('Ctrl Pts',(-0.0434115555288926,-0.148078289281839,
0.826191481594629));
#41287=CARTESIAN_POINT('Ctrl Pts',(-0.0924509079621152,-0.123549677664568,
0.823558077639828));
#41288=CARTESIAN_POINT('Ctrl Pts',(-0.120095698433879,-0.084048234986577,
0.820924673685025));
#41289=CARTESIAN_POINT('Ctrl Pts',(-0.137099129982578,-0.059752153692848,
0.819304950651447));
#41290=CARTESIAN_POINT('Ctrl Pts',(-0.146008808497438,-0.0297917172680741,
0.817685227617869));
#41291=CARTESIAN_POINT('Ctrl Pts',(-0.146164975321328,8.31911013993853E-5,
0.816065504584291));
#41292=CARTESIAN_POINT('Ctrl Pts',(-0.146233275186053,0.000116309547457056,
0.808934495415709));
#41293=CARTESIAN_POINT('Ctrl Pts',(-0.145983986542363,-0.0329580355137906,
0.810729793460572));
#41294=CARTESIAN_POINT('Ctrl Pts',(-0.134860471440613,-0.0661842257005933,
0.812525091505434));
#41295=CARTESIAN_POINT('Ctrl Pts',(-0.114274246165196,-0.0918080661847913,
0.814320389550297));
#41296=CARTESIAN_POINT('Ctrl Pts',(-0.0840554615862833,-0.129421630853252,
0.816955730616803));
#41297=CARTESIAN_POINT('Ctrl Pts',(-0.0334467307009701,-0.150653894668816,
0.819591071683309));
#41298=CARTESIAN_POINT('Ctrl Pts',(0.0145634383780638,-0.145860313412396,
0.822226412749814));
#41299=CARTESIAN_POINT('Ctrl Pts',(0.0625736074570984,-0.141066732155975,
0.82486175381632));
#41300=CARTESIAN_POINT('Ctrl Pts',(0.107985214729854,-0.110247305827569,
0.827497094882826));
#41301=CARTESIAN_POINT('Ctrl Pts',(0.130170526119325,-0.0674014545208048,
0.830132435949332));
#41302=CARTESIAN_POINT('Ctrl Pts',(0.152355837508797,-0.0245556032140414,
0.832767777015837));
#41303=CARTESIAN_POINT('Ctrl Pts',(0.151314853014986,0.0303166730710795,
0.835403118082343));
#41304=CARTESIAN_POINT('Ctrl Pts',(0.127520386856677,0.0722902292399131,
0.838038459148849));
#41305=CARTESIAN_POINT('Ctrl Pts',(0.103725920698368,0.114263785408748,
0.840673800215355));
#41306=CARTESIAN_POINT('Ctrl Pts',(0.0571779728755602,0.143338621461295,
0.843309141281861));
#41307=CARTESIAN_POINT('Ctrl Pts',(0.00902055110528975,0.146307747926884,
0.845944482348367));
#41308=CARTESIAN_POINT('Ctrl Pts',(-0.0391368706649794,0.149276874392473,
0.848579823414872));
#41309=CARTESIAN_POINT('Ctrl Pts',(-0.088903766382711,0.126140291271107,
0.851215164481378));
#41310=CARTESIAN_POINT('Ctrl Pts',(-0.117674187241089,0.087407636925452,
0.853850505547884));
#41311=CARTESIAN_POINT('Ctrl Pts',(-0.136175085157248,0.0625004974853221,
0.855545168837159));
#41312=CARTESIAN_POINT('Ctrl Pts',(-0.145993587468369,0.0311441202011877,
0.857239832126434));
#41313=CARTESIAN_POINT('Ctrl Pts',(-0.146190615322833,-9.92620605964336E-5,
0.858934495415709));
#41314=CARTESIAN_POINT('Origin',(0.,0.,-0.0924367114736152));
#41315=CARTESIAN_POINT('',(-0.117713232580125,-9.94762513365651E-5,0.882563288526385));
#41316=CARTESIAN_POINT('',(-0.11796233779121,-2.11776828218935E-5,0.892436711473616));
#41317=CARTESIAN_POINT('',(-0.117775,-1.30487598617993E-14,-0.0924367114736152));
#41318=CARTESIAN_POINT('',(-0.11766859746431,0.00500517689819253,0.932224999999999));
#41319=CARTESIAN_POINT('Ctrl Pts',(-0.117713232580125,-9.94762513365794E-5,
0.882563288526385));
#41320=CARTESIAN_POINT('Ctrl Pts',(-0.117805978893427,-0.0112620890991194,
0.88331676862211));
#41321=CARTESIAN_POINT('Ctrl Pts',(-0.111244449407799,-0.0613316426944826,
0.886703652672637));
#41322=CARTESIAN_POINT('Ctrl Pts',(-0.0402800891732956,-0.133026134299755,
0.892723940677965));
#41323=CARTESIAN_POINT('Ctrl Pts',(0.0894243408305711,-0.10638650575871,
0.900624152542373));
#41324=CARTESIAN_POINT('Ctrl Pts',(0.137929356340621,0.0167100404698593,
0.908524364406779));
#41325=CARTESIAN_POINT('Ctrl Pts',(0.0614290966487016,0.124766721395902,
0.916424576271187));
#41326=CARTESIAN_POINT('Ctrl Pts',(-0.0710668305166857,0.11939070761148,
0.924324788135593));
#41327=CARTESIAN_POINT('Ctrl Pts',(-0.116012267804409,0.0439444575637681,
0.929591596045198));
#41328=CARTESIAN_POINT('Ctrl Pts',(-0.11766859746431,0.00500517689817995,
0.932225));
#41329=CARTESIAN_POINT('',(-0.0334019664626758,0.112939183906323,0.932224999999999));
#41330=CARTESIAN_POINT('Origin',(0.,0.,0.932225));
#41331=CARTESIAN_POINT('Ctrl Pts',(-0.11796233779121,-2.11776828218909E-5,
0.892436711473617));
#41332=CARTESIAN_POINT('Ctrl Pts',(-0.117965690360961,-0.00128932424828905,
0.892522768983215));
#41333=CARTESIAN_POINT('Ctrl Pts',(-0.117371901374032,-0.0413888390951994,
0.89524416755932));
#41334=CARTESIAN_POINT('Ctrl Pts',(-0.0720261204166176,-0.118897020856024,
0.90060090720193));
#41335=CARTESIAN_POINT('Ctrl Pts',(0.0602520802431792,-0.125231345176025,
0.908506930401448));
#41336=CARTESIAN_POINT('Ctrl Pts',(0.137949690524835,-0.017881538827179,
0.916412953600965));
#41337=CARTESIAN_POINT('Ctrl Pts',(0.0900118016872842,0.105886249500893,
0.924318976800482));
#41338=CARTESIAN_POINT('Ctrl Pts',(0.00399973323748277,0.12400080376067,
0.929589658933494));
#41339=CARTESIAN_POINT('Ctrl Pts',(-0.0334019664626807,0.112939183906322,
0.932225));
#41340=CARTESIAN_POINT('Origin',(0.,0.,-0.0924367114736152));
#41341=CARTESIAN_POINT('',(-0.117626101595281,6.69479464755203E-5,0.832563288526385));
#41342=CARTESIAN_POINT('',(-0.117646735358023,-7.98810330651378E-5,0.842436711473617));
#41343=CARTESIAN_POINT('',(-0.117775,-1.30487598617993E-14,-0.0924367114736152));
#41344=CARTESIAN_POINT('Ctrl Pts',(-0.117626101595281,6.69479464755242E-5,
0.832563288526385));
#41345=CARTESIAN_POINT('Ctrl Pts',(-0.117500426517155,-0.023974851392196,
0.834183011559963));
#41346=CARTESIAN_POINT('Ctrl Pts',(-0.0986730411655657,-0.0872854052949152,
0.838436138548343));
#41347=CARTESIAN_POINT('Ctrl Pts',(0.00452896330992775,-0.13890521184416,
0.845322669491525));
#41348=CARTESIAN_POINT('Ctrl Pts',(0.118813895436517,-0.0721000537472655,
0.853222881355933));
#41349=CARTESIAN_POINT('Ctrl Pts',(0.125302761776928,0.0601169674638447,
0.861123093220339));
#41350=CARTESIAN_POINT('Ctrl Pts',(0.0181127265090936,0.137795052940508,
0.869023305084746));
#41351=CARTESIAN_POINT('Ctrl Pts',(-0.0937244491952465,0.0949681812626695,
0.876170036853428));
#41352=CARTESIAN_POINT('Ctrl Pts',(-0.11748183163376,0.0277511097711188,
0.880683364667308));
#41353=CARTESIAN_POINT('Ctrl Pts',(-0.117713232580125,-9.94762513365794E-5,
0.882563288526385));
#41354=CARTESIAN_POINT('Ctrl Pts',(-0.117646735358023,-7.9881033065143E-5,
0.842436711473617));
#41355=CARTESIAN_POINT('Ctrl Pts',(-0.117734748084911,-0.0140363608293074,
0.843377389250847));
#41356=CARTESIAN_POINT('Ctrl Pts',(-0.108999987861276,-0.0669858868324248,
0.846953408094583));
#41357=CARTESIAN_POINT('Ctrl Pts',(-0.0306982239304521,-0.135581215292453,
0.853164768004825));
#41358=CARTESIAN_POINT('Ctrl Pts',(0.0968538014257187,-0.0997179081430208,
0.861070791204343));
#41359=CARTESIAN_POINT('Ctrl Pts',(0.136419444538435,0.0267352712365894,
0.86897681440386));
#41360=CARTESIAN_POINT('Ctrl Pts',(0.0520445414416943,0.128903423908239,
0.876882837603378));
#41361=CARTESIAN_POINT('Ctrl Pts',(-0.0781668699995673,0.11412164151165,
0.884702803293296));
#41362=CARTESIAN_POINT('Ctrl Pts',(-0.117863024541527,0.0375451567622119,
0.889887427916709));
#41363=CARTESIAN_POINT('Ctrl Pts',(-0.11796233779121,-2.11776828218909E-5,
0.892436711473617));
#41364=CARTESIAN_POINT('Origin',(0.,0.,-0.0924367114736152));
#41365=CARTESIAN_POINT('',(-0.117947993201171,3.86581212928119E-5,0.782563288526384));
#41366=CARTESIAN_POINT('',(-0.117681065835582,9.35999791555828E-5,0.792436711473616));
#41367=CARTESIAN_POINT('',(-0.117775,-1.30487598617993E-14,-0.0924367114736152));
#41368=CARTESIAN_POINT('Ctrl Pts',(-0.117947993201171,3.86581212928078E-5,
0.782563288526385));
#41369=CARTESIAN_POINT('Ctrl Pts',(-0.117790128676528,-0.0366025127545069,
0.785049254497816));
#41370=CARTESIAN_POINT('Ctrl Pts',(-0.0798361540276521,-0.112340416450435,
0.790168624424051));
#41371=CARTESIAN_POINT('Ctrl Pts',(0.0488494678181175,-0.130110898691923,
0.797921398305084));
#41372=CARTESIAN_POINT('Ctrl Pts',(0.135663410254684,-0.0301754342953877,
0.805821610169492));
#41373=CARTESIAN_POINT('Ctrl Pts',(0.0993958918478579,0.0971368425207782,
0.813721822033898));
#41374=CARTESIAN_POINT('Ctrl Pts',(-0.0270490771841315,0.136321199631122,
0.821622033898304));
#41375=CARTESIAN_POINT('Ctrl Pts',(-0.10806095418056,0.0691504233541856,
0.827902522729134));
#41376=CARTESIAN_POINT('Ctrl Pts',(-0.11770475357857,0.0151131705390384,
0.831549607605161));
#41377=CARTESIAN_POINT('Ctrl Pts',(-0.117626101595281,6.69479464755242E-5,
0.832563288526385));
#41378=CARTESIAN_POINT('Ctrl Pts',(-0.117681065835582,9.35999791555758E-5,
0.792436711473616));
#41379=CARTESIAN_POINT('Ctrl Pts',(-0.117480451076367,-0.0265229424847173,
0.794232009518479));
#41380=CARTESIAN_POINT('Ctrl Pts',(-0.0953885925249484,-0.0925118216380055,
0.798662648629848));
#41381=CARTESIAN_POINT('Ctrl Pts',(0.0138111005924944,-0.138325195186183,
0.80572862880772));
#41382=CARTESIAN_POINT('Ctrl Pts',(0.123445922182148,-0.0639194978340518,
0.813634652007238));
#41383=CARTESIAN_POINT('Ctrl Pts',(0.120932728835538,0.0685557124046954,
0.821540675206756));
#41384=CARTESIAN_POINT('Ctrl Pts',(0.0085545008581314,0.138749538494654,
0.829446698406273));
#41385=CARTESIAN_POINT('Ctrl Pts',(-0.0972993756118875,0.0895381706496827,
0.83641204382856));
#41386=CARTESIAN_POINT('Ctrl Pts',(-0.117488177410916,0.0250631961509614,
0.840742048184341));
#41387=CARTESIAN_POINT('Ctrl Pts',(-0.117646735358023,-7.9881033065143E-5,
0.842436711473617));
#41388=CARTESIAN_POINT('Origin',(0.,0.,-0.0924367114736152));
#41389=CARTESIAN_POINT('',(-0.117729227722965,-0.000102982086865302,0.732563288526385));
#41390=CARTESIAN_POINT('',(-0.117964389557135,-3.94331754086097E-6,0.742436711473616));
#41391=CARTESIAN_POINT('',(-0.117775,-1.30487598617993E-14,-0.0924367114736152));
#41392=CARTESIAN_POINT('Ctrl Pts',(-0.117729227722965,-0.000102982086865302,
0.732563288526385));
#41393=CARTESIAN_POINT('Ctrl Pts',(-0.117820491001352,-0.0107487282458691,
0.733282093480867));
#41394=CARTESIAN_POINT('Ctrl Pts',(-0.111634982628329,-0.060291927513671,
0.73663430239015));
#41395=CARTESIAN_POINT('Ctrl Pts',(-0.0420051819866054,-0.132478981273086,
0.742619915254238));
#41396=CARTESIAN_POINT('Ctrl Pts',(0.0880063312515965,-0.107563941317063,
0.750520127118644));
#41397=CARTESIAN_POINT('Ctrl Pts',(0.1381735813042,0.0149391196739674,0.758420338983051));
#41398=CARTESIAN_POINT('Ctrl Pts',(0.0629820334107182,0.123888575547709,
0.766320550847457));
#41399=CARTESIAN_POINT('Ctrl Pts',(-0.069350334823955,0.120439391087123,
0.774220762711865));
#41400=CARTESIAN_POINT('Ctrl Pts',(-0.116921686943853,0.0431900873220952,
0.77963500860484));
#41401=CARTESIAN_POINT('Ctrl Pts',(-0.117957355850309,0.00221177730489086,
0.782415850543013));
#41402=CARTESIAN_POINT('Ctrl Pts',(-0.117947993201171,3.86581212928078E-5,
0.782563288526385));
#41403=CARTESIAN_POINT('Ctrl Pts',(-0.117964389557135,-3.94331754086175E-6,
0.742436711473616));
#41404=CARTESIAN_POINT('Ctrl Pts',(-0.117964495672005,-0.000218720446770248,
0.742451288719605));
#41405=CARTESIAN_POINT('Ctrl Pts',(-0.117867006535742,-0.039261788207105,
0.745101207032099));
#41406=CARTESIAN_POINT('Ctrl Pts',(-0.0752264694457675,-0.116899882557203,
0.750386466411098));
#41407=CARTESIAN_POINT('Ctrl Pts',(0.0568996293847587,-0.126834681679914,
0.758292489610617));
#41408=CARTESIAN_POINT('Ctrl Pts',(0.137333582544999,-0.0215427765762162,
0.766198512810132));
#41409=CARTESIAN_POINT('Ctrl Pts',(0.0930027975645983,0.103320297856606,
0.774104536009652));
#41410=CARTESIAN_POINT('Ctrl Pts',(-0.035819122070238,0.13431900488649,
0.782010559209168));
#41411=CARTESIAN_POINT('Ctrl Pts',(-0.110236635830862,0.0639621230870467,
0.788121284363823));
#41412=CARTESIAN_POINT('Ctrl Pts',(-0.117774936058969,0.0125478221742061,
0.791596668451973));
#41413=CARTESIAN_POINT('Ctrl Pts',(-0.117681065835582,9.35999791555758E-5,
0.792436711473616));
#41414=CARTESIAN_POINT('Origin',(0.,0.,-0.0924367114736152));
#41415=CARTESIAN_POINT('',(-0.117617624673989,6.03055670430245E-5,0.682563288526385));
#41416=CARTESIAN_POINT('',(-0.117670490259622,-9.01168895870441E-5,0.692436711473616));
#41417=CARTESIAN_POINT('',(-0.117775,-1.30487598617993E-14,-0.0924367114736152));
#41418=CARTESIAN_POINT('Ctrl Pts',(-0.117617624673989,6.03055670430289E-5,
0.682563288526385));
#41419=CARTESIAN_POINT('Ctrl Pts',(-0.117507328717046,-0.0234710821212703,
0.68414833641872));
#41420=CARTESIAN_POINT('Ctrl Pts',(-0.0992894616255371,-0.0862548596187289,
0.688366788265857));
#41421=CARTESIAN_POINT('Ctrl Pts',(0.00271304928865532,-0.138952348570324,
0.695218644067796));
#41422=CARTESIAN_POINT('Ctrl Pts',(0.117860843754417,-0.0736473850127282,
0.703118855932203));
#41423=CARTESIAN_POINT('Ctrl Pts',(0.126078691992566,0.0584746033489104,
0.711019067796611));
#41424=CARTESIAN_POINT('Ctrl Pts',(0.0199109026571207,0.137545162630623,
0.718919279661016));
#41425=CARTESIAN_POINT('Ctrl Pts',(-0.0930178497353151,0.0959867468400004,
0.726100686570943));
#41426=CARTESIAN_POINT('Ctrl Pts',(-0.117486140108619,0.0282528811088558,
0.730648689526065));
#41427=CARTESIAN_POINT('Ctrl Pts',(-0.117729227722965,-0.000102982086865302,
0.732563288526385));
#41428=CARTESIAN_POINT('Ctrl Pts',(-0.117670490259622,-9.01168895870632E-5,
0.692436711473616));
#41429=CARTESIAN_POINT('Ctrl Pts',(-0.117763421933718,-0.0129794996427261,
0.693305908987236));
#41430=CARTESIAN_POINT('Ctrl Pts',(-0.109885703418251,-0.0648380928819097,
0.696810447567362));
#41431=CARTESIAN_POINT('Ctrl Pts',(-0.0343406886760894,-0.134704570618338,
0.702950327213994));
#41432=CARTESIAN_POINT('Ctrl Pts',(0.0941327483034478,-0.102291886006113,
0.710856350413511));
#41433=CARTESIAN_POINT('Ctrl Pts',(0.137088516418336,0.0230508765206803,
0.718762373613029));
#41434=CARTESIAN_POINT('Ctrl Pts',(0.0555021824679276,0.127452391053421,
0.726668396812546));
#41435=CARTESIAN_POINT('Ctrl Pts',(-0.0762633445254468,0.116087019895361,
0.734559842766075));
#41436=CARTESIAN_POINT('Ctrl Pts',(-0.117945311741555,0.0386096693093802,
0.739815947653099));
#41437=CARTESIAN_POINT('Ctrl Pts',(-0.117964389557135,-3.94331754086175E-6,
0.742436711473616));
#41438=CARTESIAN_POINT('Origin',(0.,0.,-0.0924367114736152));
#41439=CARTESIAN_POINT('',(-0.117940203002297,4.70676520639361E-5,0.632563288526384));
#41440=CARTESIAN_POINT('',(-0.117656000082187,8.43516556759474E-5,0.642436711473616));
#41441=CARTESIAN_POINT('',(-0.117775,-1.30487598617993E-14,-0.0924367114736152));
#41442=CARTESIAN_POINT('Ctrl Pts',(-0.117940203002297,4.7067652063935E-5,
0.632563288526384));
#41443=CARTESIAN_POINT('Ctrl Pts',(-0.117755638437952,-0.0360893706242894,
0.635014579356573));
#41444=CARTESIAN_POINT('Ctrl Pts',(-0.0807233593759693,-0.111374211355997,
0.640099274141563));
#41445=CARTESIAN_POINT('Ctrl Pts',(0.0471445089225743,-0.130738330601145,
0.647817372881356));
#41446=CARTESIAN_POINT('Ctrl Pts',(0.135257361515437,-0.0319462355497722,
0.655717584745763));
#41447=CARTESIAN_POINT('Ctrl Pts',(0.100657174442164,0.0958292702846084,
0.66361779661017));
#41448=CARTESIAN_POINT('Ctrl Pts',(-0.0252648283287276,0.136663104967713,
0.671518008474576));
#41449=CARTESIAN_POINT('Ctrl Pts',(-0.107599838532302,0.0701921319068488,
0.677833172446648));
#41450=CARTESIAN_POINT('Ctrl Pts',(-0.11769057479473,0.0156240453509343,
0.681514932463917));
#41451=CARTESIAN_POINT('Ctrl Pts',(-0.117617624673989,6.03055670430289E-5,
0.682563288526385));
#41452=CARTESIAN_POINT('Ctrl Pts',(-0.117656000082187,8.43516556759457E-5,
0.642436711473616));
#41453=CARTESIAN_POINT('Ctrl Pts',(-0.117484912294625,-0.0254861849147704,
0.644160529254868));
#41454=CARTESIAN_POINT('Ctrl Pts',(-0.0967548225821553,-0.0904011202578769,
0.648519688102626));
#41455=CARTESIAN_POINT('Ctrl Pts',(0.0100790193068892,-0.138647097388359,
0.655514188016889));
#41456=CARTESIAN_POINT('Ctrl Pts',(0.121678866262096,-0.0672224497442505,
0.663420211216407));
#41457=CARTESIAN_POINT('Ctrl Pts',(0.122735961854403,0.0652724131012164,
0.671326234415924));
#41458=CARTESIAN_POINT('Ctrl Pts',(0.0122899564463577,0.138468628991968,
0.679232257615441));
#41459=CARTESIAN_POINT('Ctrl Pts',(-0.0959511456548746,0.0916518108144888,
0.686269083301339));
#41460=CARTESIAN_POINT('Ctrl Pts',(-0.117481660132417,0.0261001331898457,
0.69067056792073));
#41461=CARTESIAN_POINT('Ctrl Pts',(-0.117670490259622,-9.01168895870632E-5,
0.692436711473616));
#41462=CARTESIAN_POINT('Origin',(0.,0.,-0.0924367114736152));
#41463=CARTESIAN_POINT('',(-0.117743952026517,-0.000104311439111954,0.582563288526385));
#41464=CARTESIAN_POINT('',(-0.11796202899481,1.53301186523688E-5,0.592436711473616));
#41465=CARTESIAN_POINT('',(-0.117775,-1.30487598617993E-14,-0.0924367114736152));
#41466=CARTESIAN_POINT('Ctrl Pts',(-0.117743952026517,-0.000104311439111965,
0.582563288526385));
#41467=CARTESIAN_POINT('Ctrl Pts',(-0.117832850528047,-0.0102332806752188,
0.583247418339623));
#41468=CARTESIAN_POINT('Ctrl Pts',(-0.112015701243022,-0.0592509231652696,
0.586564952107665));
#41469=CARTESIAN_POINT('Ctrl Pts',(-0.0437333382095171,-0.131918576929031,
0.592515889830509));
#41470=CARTESIAN_POINT('Ctrl Pts',(0.0865927525795457,-0.108705156320324,
0.600416101694915));
#41471=CARTESIAN_POINT('Ctrl Pts',(0.138357057429181,0.0131316590523252,
0.608316313559322));
#41472=CARTESIAN_POINT('Ctrl Pts',(0.0645961051971127,0.123054699232873,
0.616216525423729));
#41473=CARTESIAN_POINT('Ctrl Pts',(-0.0677700447892944,0.121335637135943,
0.624116737288135));
#41474=CARTESIAN_POINT('Ctrl Pts',(-0.116658230525945,0.0442240676066805,
0.629565658322354));
#41475=CARTESIAN_POINT('Ctrl Pts',(-0.117953914810415,0.00273174284681649,
0.63238117540177));
#41476=CARTESIAN_POINT('Ctrl Pts',(-0.117940203002297,4.7067652063935E-5,
0.632563288526384));
#41477=CARTESIAN_POINT('Ctrl Pts',(-0.11796202899481,1.53301186523688E-5,
0.592436711473616));
#41478=CARTESIAN_POINT('Ctrl Pts',(-0.11789197517919,-0.0379767160352311,
0.5950151495225));
#41479=CARTESIAN_POINT('Ctrl Pts',(-0.077400231210687,-0.114927628746102,
0.600228928637889));
#41480=CARTESIAN_POINT('Ctrl Pts',(0.0534615168199478,-0.12832174587234,
0.608078048819785));
#41481=CARTESIAN_POINT('Ctrl Pts',(0.136703270562712,-0.0252352939724056,
0.615984072019302));
#41482=CARTESIAN_POINT('Ctrl Pts',(0.0957529101571512,0.100776904302778,
0.623890095218819));
#41483=CARTESIAN_POINT('Ctrl Pts',(-0.0321870028708045,0.135235354440354,
0.631796118418337));
#41484=CARTESIAN_POINT('Ctrl Pts',(-0.109365567925802,0.0661098894434327,
0.637978323836602));
#41485=CARTESIAN_POINT('Ctrl Pts',(-0.117746468172191,0.0136055832811398,
0.641525188188362));
#41486=CARTESIAN_POINT('Ctrl Pts',(-0.117656000082187,8.43516556759457E-5,
0.642436711473616));
#41487=CARTESIAN_POINT('Origin',(0.,0.,-0.0924367114736152));
#41488=CARTESIAN_POINT('',(-0.117610072962214,5.33056148506657E-5,0.532563288526385));
#41489=CARTESIAN_POINT('',(-0.117697192808605,-9.79052972080175E-5,0.542436711473616));
#41490=CARTESIAN_POINT('',(-0.117775,-1.30487598617993E-14,-0.0924367114736152));
#41491=CARTESIAN_POINT('Ctrl Pts',(-0.117610072962214,5.330561485066E-5,
0.532563288526385));
#41492=CARTESIAN_POINT('Ctrl Pts',(-0.117515081084069,-0.02296700464597,
0.534113661277477));
#41493=CARTESIAN_POINT('Ctrl Pts',(-0.0998958154709599,-0.0852230040130838,
0.538297437983371));
#41494=CARTESIAN_POINT('Ctrl Pts',(0.000896453507092177,-0.13897594101512,
0.545114618644068));
#41495=CARTESIAN_POINT('Ctrl Pts',(0.116888066275103,-0.0751817515916976,
0.553014830508475));
#41496=CARTESIAN_POINT('Ctrl Pts',(0.126832290918542,0.0568215257651788,
0.560915042372882));
#41497=CARTESIAN_POINT('Ctrl Pts',(0.0217071709283622,0.137273138451102,
0.568815254237287));
#41498=CARTESIAN_POINT('Ctrl Pts',(-0.0923030266130234,0.097000942567024,
0.576031336288457));
#41499=CARTESIAN_POINT('Ctrl Pts',(-0.117490655726745,0.0287559098676526,
0.580614014384821));
#41500=CARTESIAN_POINT('Ctrl Pts',(-0.117743952026517,-0.000104311439111965,
0.582563288526385));
#41501=CARTESIAN_POINT('Ctrl Pts',(-0.117697192808605,-9.79052972080122E-5,
0.542436711473616));
#41502=CARTESIAN_POINT('Ctrl Pts',(-0.11779135888071,-0.011920519912767,
0.543234428723626));
#41503=CARTESIAN_POINT('Ctrl Pts',(-0.110735559311442,-0.0626905594030618,
0.546667487040141));
#41504=CARTESIAN_POINT('Ctrl Pts',(-0.0379577228913647,-0.133730383672961,
0.552735886423163));
#41505=CARTESIAN_POINT('Ctrl Pts',(0.0913424031974019,-0.104791076063462,
0.56064190962268));
#41506=CARTESIAN_POINT('Ctrl Pts',(0.137659831668342,0.0193487722984857,
0.568547932822197));
#41507=CARTESIAN_POINT('Ctrl Pts',(0.0589161298691768,0.125910658348106,
0.576453956021715));
#41508=CARTESIAN_POINT('Ctrl Pts',(-0.0733516660922674,0.11808529682354,
0.584359979221232));
#41509=CARTESIAN_POINT('Ctrl Pts',(-0.117576903938907,0.0405212291720611,
0.589687564371866));
#41510=CARTESIAN_POINT('Ctrl Pts',(-0.117963574998021,0.000853768751192661,
0.592379808455994));
#41511=CARTESIAN_POINT('Ctrl Pts',(-0.11796202899481,1.53301186523688E-5,
0.592436711473616));
#41512=CARTESIAN_POINT('Origin',(0.,0.,-0.0924367114736152));
#41513=CARTESIAN_POINT('',(-0.117931139389423,5.50751932371175E-5,0.482563288526385));
#41514=CARTESIAN_POINT('',(-0.117634119017629,7.2868354416035E-5,0.492436711473616));
#41515=CARTESIAN_POINT('',(-0.117775,-1.30487598617993E-14,-0.0924367114736152));
#41516=CARTESIAN_POINT('Ctrl Pts',(-0.117931139389423,5.50751932371233E-5,
0.482563288526385));
#41517=CARTESIAN_POINT('Ctrl Pts',(-0.117723480179333,-0.0355774509071747,
0.48497990421533));
#41518=CARTESIAN_POINT('Ctrl Pts',(-0.0815990427908323,-0.11040399129502,
0.490029923859077));
#41519=CARTESIAN_POINT('Ctrl Pts',(0.0454314893010671,-0.131343426138561,
0.497713347457628));
#41520=CARTESIAN_POINT('Ctrl Pts',(0.134828208757446,-0.0337115697229769,
0.505613559322033));
#41521=CARTESIAN_POINT('Ctrl Pts',(0.10190123992053,0.0945053073249706,
0.513513771186441));
#41522=CARTESIAN_POINT('Ctrl Pts',(-0.0234762303627364,0.136981686432473,
0.521413983050847));
#41523=CARTESIAN_POINT('Ctrl Pts',(-0.107129919570411,0.0712336270252472,
0.527763822164162));
#41524=CARTESIAN_POINT('Ctrl Pts',(-0.117676430661069,0.0161344153441048,
0.531480257322675));
#41525=CARTESIAN_POINT('Ctrl Pts',(-0.117610072962214,5.330561485066E-5,
0.532563288526385));
#41526=CARTESIAN_POINT('Ctrl Pts',(-0.117634119017629,7.28683544160419E-5,
0.492436711473616));
#41527=CARTESIAN_POINT('Ctrl Pts',(-0.117494141600147,-0.0244488239796579,
0.494089048991258));
#41528=CARTESIAN_POINT('Ctrl Pts',(-0.0980773705094754,-0.0882836093782272,
0.498376727575405));
#41529=CARTESIAN_POINT('Ctrl Pts',(0.00633962999064621,-0.138868330932566,
0.505299747226058));
#41530=CARTESIAN_POINT('Ctrl Pts',(0.119823436886959,-0.0704765792090683,
0.513205770425575));
#41531=CARTESIAN_POINT('Ctrl Pts',(0.124450111907394,0.0619416975118724,
0.521111793625093));
#41532=CARTESIAN_POINT('Ctrl Pts',(0.0160164158031762,0.138087213996209,
0.52901781682461));
#41533=CARTESIAN_POINT('Ctrl Pts',(-0.0945587588515482,0.0937580907599652,
0.536126122774119));
#41534=CARTESIAN_POINT('Ctrl Pts',(-0.117480271566393,0.0271367046984328,
0.54059908765712));
#41535=CARTESIAN_POINT('Ctrl Pts',(-0.117697192808605,-9.79052972080122E-5,
0.542436711473616));
#41536=CARTESIAN_POINT('Origin',(0.,0.,-0.0924367114736152));
#41537=CARTESIAN_POINT('',(-0.117758961667293,-0.000104950384427651,0.432563288526384));
#41538=CARTESIAN_POINT('',(-0.117952286276812,3.39956489144189E-5,0.442436711473616));
#41539=CARTESIAN_POINT('',(-0.117775,-1.30487598617993E-14,-0.0924367114736152));
#41540=CARTESIAN_POINT('Ctrl Pts',(-0.117758961667293,-0.000104950384427652,
0.432563288526384));
#41541=CARTESIAN_POINT('Ctrl Pts',(-0.117844817924839,-0.00971740507401162,
0.43321274319838));
#41542=CARTESIAN_POINT('Ctrl Pts',(-0.11238834839588,-0.0582101957930696,
0.436495601825179));
#41543=CARTESIAN_POINT('Ctrl Pts',(-0.045454021205161,-0.13133563022352,
0.44241186440678));
#41544=CARTESIAN_POINT('Ctrl Pts',(0.085164376794762,-0.109827795821861,
0.450312076271186));
#41545=CARTESIAN_POINT('Ctrl Pts',(0.138516891217783,0.0113219546585138,
0.458212288135593));
#41546=CARTESIAN_POINT('Ctrl Pts',(0.0661991384108791,0.12219979494085,
0.4661125));
#41547=CARTESIAN_POINT('Ctrl Pts',(-0.0661781734963363,0.122211149911198,
0.474012711864406));
#41548=CARTESIAN_POINT('Ctrl Pts',(-0.116387669202521,0.0452586237679377,
0.479496308039868));
#41549=CARTESIAN_POINT('Ctrl Pts',(-0.117949767953432,0.00325157581050499,
0.482346500260528));
#41550=CARTESIAN_POINT('Ctrl Pts',(-0.117931139389423,5.50751932371233E-5,
0.482563288526385));
#41551=CARTESIAN_POINT('Ctrl Pts',(-0.117952286276812,3.39956489144155E-5,
0.442436711473616));
#41552=CARTESIAN_POINT('Ctrl Pts',(-0.117810336120504,-0.0369130001778165,
0.444943669258889));
#41553=CARTESIAN_POINT('Ctrl Pts',(-0.0792807483010678,-0.11295446192069,
0.450085968110668));
#41554=CARTESIAN_POINT('Ctrl Pts',(0.0499845850166584,-0.129715633233345,
0.457863608028953));
#41555=CARTESIAN_POINT('Ctrl Pts',(0.135973695209673,-0.0289094872912353,
0.465769631228471));
#41556=CARTESIAN_POINT('Ctrl Pts',(0.0984334954810092,0.0981603342078928,
0.473675654427988));
#41557=CARTESIAN_POINT('Ctrl Pts',(-0.0285315135918273,0.136053507770195,
0.481581677627505));
#41558=CARTESIAN_POINT('Ctrl Pts',(-0.108458155672614,0.0682577387762276,
0.487835363309382));
#41559=CARTESIAN_POINT('Ctrl Pts',(-0.117717393951882,0.0146612380616908,
0.491453707924752));
#41560=CARTESIAN_POINT('Ctrl Pts',(-0.117634119017629,7.28683544160419E-5,
0.492436711473616));
#41561=CARTESIAN_POINT('Origin',(0.,0.,-0.0924367114736152));
#41562=CARTESIAN_POINT('',(-0.117603494801586,4.59807059966066E-5,0.382563288526384));
#41563=CARTESIAN_POINT('',(-0.117726185906756,-0.000103034036682964,0.392436711473616));
#41564=CARTESIAN_POINT('',(-0.117775,-1.30487598617993E-14,-0.0924367114736152));
#41565=CARTESIAN_POINT('Ctrl Pts',(-0.117603494801586,4.59807059966007E-5,
0.382563288526384));
#41566=CARTESIAN_POINT('Ctrl Pts',(-0.117523654559104,-0.0224626175592834,
0.384078986136234));
#41567=CARTESIAN_POINT('Ctrl Pts',(-0.100492247037195,-0.0841899886309759,
0.388228087700885));
#41568=CARTESIAN_POINT('Ctrl Pts',(-0.000920295459793275,-0.138975785179272,
0.395010593220339));
#41569=CARTESIAN_POINT('Ctrl Pts',(0.115895314901344,-0.0767032710765764,
0.402910805084745));
#41570=CARTESIAN_POINT('Ctrl Pts',(0.127564216682018,0.0551587384938402,
0.410811016949152));
#41571=CARTESIAN_POINT('Ctrl Pts',(0.0234997298595607,0.136977656960748,
0.418711228813559));
#41572=CARTESIAN_POINT('Ctrl Pts',(-0.0915774899741938,0.0980128855194841,
0.42596198600597));
#41573=CARTESIAN_POINT('Ctrl Pts',(-0.117496688612794,0.0292591044291153,
0.430579339243578));
#41574=CARTESIAN_POINT('Ctrl Pts',(-0.117758961667293,-0.000104950384427652,
0.432563288526384));
#41575=CARTESIAN_POINT('Ctrl Pts',(-0.117726185906756,-0.000103034036682944,
0.392436711473616));
#41576=CARTESIAN_POINT('Ctrl Pts',(-0.117818125179144,-0.0108595471866994,
0.393162948460015));
#41577=CARTESIAN_POINT('Ctrl Pts',(-0.111550100869322,-0.0605437012261054,
0.39652452651292));
#41578=CARTESIAN_POINT('Ctrl Pts',(-0.0415471952570256,-0.13265909245389,
0.40252144563233));
#41579=CARTESIAN_POINT('Ctrl Pts',(0.0884857325734624,-0.107214175253801,
0.410427468831849));
#41580=CARTESIAN_POINT('Ctrl Pts',(0.138131189387156,0.0156326185555932,
0.418333492031365));
#41581=CARTESIAN_POINT('Ctrl Pts',(0.062287297122381,0.124277499418049,
0.426239515230884));
#41582=CARTESIAN_POINT('Ctrl Pts',(-0.0701433255283678,0.120018824057881,
0.4341455384304));
#41583=CARTESIAN_POINT('Ctrl Pts',(-0.117063601095489,0.0426502166584235,
0.439544603844645));
#41584=CARTESIAN_POINT('Ctrl Pts',(-0.117959555656036,0.00192608038356173,
0.442308328192384));
#41585=CARTESIAN_POINT('Ctrl Pts',(-0.117952286276812,3.39956489144155E-5,
0.442436711473616));
#41586=CARTESIAN_POINT('Origin',(0.,0.,-0.0924367114736152));
#41587=CARTESIAN_POINT('',(-0.117920926539219,6.26243704048756E-5,0.332563288526384));
#41588=CARTESIAN_POINT('',(-0.117615878293784,5.9477676878486E-5,0.342436711473616));
#41589=CARTESIAN_POINT('',(-0.117775,-1.30487598617993E-14,-0.0924367114736152));
#41590=CARTESIAN_POINT('Ctrl Pts',(-0.117920926539219,6.26243704048737E-5,
0.332563288526384));
#41591=CARTESIAN_POINT('Ctrl Pts',(-0.117693603628949,-0.0350666637837455,
0.334945229074087));
#41592=CARTESIAN_POINT('Ctrl Pts',(-0.0824632530796663,-0.109429893167014,
0.339960573576592));
#41593=CARTESIAN_POINT('Ctrl Pts',(0.0437107063235388,-0.131926077644361,
0.347609322033898));
#41594=CARTESIAN_POINT('Ctrl Pts',(0.134376016486386,-0.0354711432460098,
0.355509533898305));
#41595=CARTESIAN_POINT('Ctrl Pts',(0.103127892463174,0.0931651952503325,
0.363409745762711));
#41596=CARTESIAN_POINT('Ctrl Pts',(-0.0216836207666979,0.137276860396698,
0.371309957627119));
#41597=CARTESIAN_POINT('Ctrl Pts',(-0.106651080731,0.0722748925449633,0.377694471881676));
#41598=CARTESIAN_POINT('Ctrl Pts',(-0.117662370625513,0.0166442803494234,
0.381445582181431));
#41599=CARTESIAN_POINT('Ctrl Pts',(-0.117603494801586,4.59807059966007E-5,
0.382563288526384));
#41600=CARTESIAN_POINT('Ctrl Pts',(-0.117615878293784,5.94776768784704E-5,
0.342436711473616));
#41601=CARTESIAN_POINT('Ctrl Pts',(-0.11750760701874,-0.0234105356203755,
0.344017568727647));
#41602=CARTESIAN_POINT('Ctrl Pts',(-0.0993568477409689,-0.0861600913990265,
0.348233767048184));
#41603=CARTESIAN_POINT('Ctrl Pts',(0.00259563734382704,-0.138988729439456,
0.355085306435226));
#41604=CARTESIAN_POINT('Ctrl Pts',(0.117881001348277,-0.0736795342380946,
0.362991329634744));
#41605=CARTESIAN_POINT('Ctrl Pts',(0.12607389627645,0.0585660048329233,
0.370897352834261));
#41606=CARTESIAN_POINT('Ctrl Pts',(0.0197312453245754,0.137605531147394,
0.378803376033779));
#41607=CARTESIAN_POINT('Ctrl Pts',(-0.0931217327741457,0.0958562111818821,
0.385983162246897));
#41608=CARTESIAN_POINT('Ctrl Pts',(-0.117484499455465,0.0281732773148422,
0.39052760739351));
#41609=CARTESIAN_POINT('Ctrl Pts',(-0.117726185906756,-0.000103034036682944,
0.392436711473616));
#41610=CARTESIAN_POINT('Origin',(0.,0.,-0.0924367114736152));
#41611=CARTESIAN_POINT('',(-0.117774170260593,-0.000104886777209015,0.282563288526384));
#41612=CARTESIAN_POINT('',(-0.11793628481875,5.1384428605368E-5,0.292436711473616));
#41613=CARTESIAN_POINT('',(-0.117775,-1.30487598617993E-14,-0.0924367114736152));
#41614=CARTESIAN_POINT('Ctrl Pts',(-0.117774170260593,-0.00010488677720901,
0.282563288526384));
#41615=CARTESIAN_POINT('Ctrl Pts',(-0.117856360533384,-0.0092011162257308,
0.283178068057138));
#41616=CARTESIAN_POINT('Ctrl Pts',(-0.112752995425492,-0.057169777637724,
0.286426251542693));
#41617=CARTESIAN_POINT('Ctrl Pts',(-0.0471669369944997,-0.130730240818604,
0.292307838983051));
#41618=CARTESIAN_POINT('Ctrl Pts',(0.0837214480778729,-0.110931667893667,
0.300208050847457));
#41619=CARTESIAN_POINT('Ctrl Pts',(0.138653055169421,0.00951031556331505,
0.308108262711865));
#41620=CARTESIAN_POINT('Ctrl Pts',(0.0677908594821406,0.121324009085596,
0.316008474576271));
#41621=CARTESIAN_POINT('Ctrl Pts',(-0.0645749936433688,0.123065779182871,
0.323908686440678));
#41622=CARTESIAN_POINT('Ctrl Pts',(-0.116109941121323,0.0462937466385656,
0.329426957757382));
#41623=CARTESIAN_POINT('Ctrl Pts',(-0.117944925204334,0.00377125198361699,
0.332311825119284));
#41624=CARTESIAN_POINT('Ctrl Pts',(-0.117920926539219,6.26243704048737E-5,
0.332563288526384));
#41625=CARTESIAN_POINT('Ctrl Pts',(-0.11793628481875,5.13844286053676E-5,
0.292436711473616));
#41626=CARTESIAN_POINT('Ctrl Pts',(-0.117738942084994,-0.0358551097426003,
0.294872188995279));
#41627=CARTESIAN_POINT('Ctrl Pts',(-0.0811119992076199,-0.110963296543085,
0.299943007583447));
#41628=CARTESIAN_POINT('Ctrl Pts',(0.046471358419155,-0.131015331511595,
0.307649167238122));
#41629=CARTESIAN_POINT('Ctrl Pts',(0.135145386671506,-0.0325626888604762,
0.315555190437639));
#41630=CARTESIAN_POINT('Ctrl Pts',(0.101042606300054,0.0954724879559945,
0.323461213637157));
#41631=CARTESIAN_POINT('Ctrl Pts',(-0.0248553070174182,0.136772869961425,
0.331367236836674));
#41632=CARTESIAN_POINT('Ctrl Pts',(-0.107513748550757,0.0704052555566997,
0.33769240278216));
#41633=CARTESIAN_POINT('Ctrl Pts',(-0.117688098797311,0.0157147489149463,
0.341382227661141));
#41634=CARTESIAN_POINT('Ctrl Pts',(-0.117615878293784,5.94776768784704E-5,
0.342436711473616));
#41635=CARTESIAN_POINT('Origin',(0.,0.,-0.0924367114736152));
#41636=CARTESIAN_POINT('',(-0.117597921122191,3.83764452643825E-5,0.232563288526384));
#41637=CARTESIAN_POINT('',(-0.117756807889117,-0.000105309437279225,0.242436711473616));
#41638=CARTESIAN_POINT('',(-0.117775,-1.30487598617993E-14,-0.0924367114736152));
#41639=CARTESIAN_POINT('Ctrl Pts',(-0.117597921122191,3.83764452643858E-5,
0.232563288526384));
#41640=CARTESIAN_POINT('Ctrl Pts',(-0.117532990113526,-0.0219578937617309,
0.234044310994991));
#41641=CARTESIAN_POINT('Ctrl Pts',(-0.101078828998682,-0.0831558954107903,
0.238158737418399));
#41642=CARTESIAN_POINT('Ctrl Pts',(-0.00273688716624997,-0.138951881091211,
0.24490656779661));
#41643=CARTESIAN_POINT('Ctrl Pts',(0.114882759277182,-0.0782116834669906,
0.252806779661017));
#41644=CARTESIAN_POINT('Ctrl Pts',(0.128274344207101,0.0534865256689417,
0.260706991525423));
#41645=CARTESIAN_POINT('Ctrl Pts',(0.0252882731449639,0.136658768658679,
0.26860720338983));
#41646=CARTESIAN_POINT('Ctrl Pts',(-0.090841176153826,0.099022467675047,
0.275892635723484));
#41647=CARTESIAN_POINT('Ctrl Pts',(-0.117504299056729,0.0297625209893518,
0.280544664102335));
#41648=CARTESIAN_POINT('Ctrl Pts',(-0.117774170260593,-0.00010488677720901,
0.282563288526384));
#41649=CARTESIAN_POINT('Ctrl Pts',(-0.117756807889117,-0.000105309437279212,
0.242436711473616));
#41650=CARTESIAN_POINT('Ctrl Pts',(-0.117843399042527,-0.00979668321532341,
0.243091468196405));
#41651=CARTESIAN_POINT('Ctrl Pts',(-0.112329964982903,-0.058397845463228,
0.246381565985699));
#41652=CARTESIAN_POINT('Ctrl Pts',(-0.0451064993838265,-0.131491474848312,
0.252307004841499));
#41653=CARTESIAN_POINT('Ctrl Pts',(0.0855648107118161,-0.1095594241143,
0.260213028041017));
#41654=CARTESIAN_POINT('Ctrl Pts',(0.138502247321704,0.0119051136596435,
0.268119051240535));
#41655=CARTESIAN_POINT('Ctrl Pts',(0.0656132363391791,0.122554100141606,
0.276025074440052));
#41656=CARTESIAN_POINT('Ctrl Pts',(-0.066884052510702,0.121865203254083,
0.283931097639569));
#41657=CARTESIAN_POINT('Ctrl Pts',(-0.1165204945288,0.0447817101515102,
0.289401643317424));
#41658=CARTESIAN_POINT('Ctrl Pts',(-0.117952479432728,0.00299799310969985,
0.292236847928773));
#41659=CARTESIAN_POINT('Ctrl Pts',(-0.11793628481875,5.13844286053676E-5,
0.292436711473616));
#41660=CARTESIAN_POINT('Origin',(0.,0.,-0.0924367114736152));
#41661=CARTESIAN_POINT('',(-0.117909687164366,6.9664588846411E-5,0.182563288526384));
#41662=CARTESIAN_POINT('',(-0.117601649275994,4.45452448404882E-5,0.192436711473616));
#41663=CARTESIAN_POINT('',(-0.117775,-1.30487598617993E-14,-0.0924367114736152));
#41664=CARTESIAN_POINT('Ctrl Pts',(-0.117909687164366,6.96645888464118E-5,
0.182563288526384));
#41665=CARTESIAN_POINT('Ctrl Pts',(-0.11766595726848,-0.0345569219122136,
0.184910553932844));
#41666=CARTESIAN_POINT('Ctrl Pts',(-0.0833160382623138,-0.10845204978507,
0.189891223294105));
#41667=CARTESIAN_POINT('Ctrl Pts',(0.0419824540321544,-0.132486185591528,
0.197505296610169));
#41668=CARTESIAN_POINT('Ctrl Pts',(0.133900861976353,-0.0372246554226585,
0.205405508474576));
#41669=CARTESIAN_POINT('Ctrl Pts',(0.10433692245731,0.0918091630494651,
0.213305720338983));
#41670=CARTESIAN_POINT('Ctrl Pts',(-0.0198873058616059,0.137548576426424,
0.221205932203389));
#41671=CARTESIAN_POINT('Ctrl Pts',(-0.10616324692175,0.0733158722115256,
0.22762512159919));
#41672=CARTESIAN_POINT('Ctrl Pts',(-0.117648443848114,0.0171536431540524,
0.231410907040188));
#41673=CARTESIAN_POINT('Ctrl Pts',(-0.117597921122191,3.83764452643858E-5,
0.232563288526384));
#41674=CARTESIAN_POINT('Ctrl Pts',(-0.117601649275994,4.45452448404882E-5,
0.192436711473616));
#41675=CARTESIAN_POINT('Ctrl Pts',(-0.11752478280801,-0.0223710360060294,
0.193946088464036));
#41676=CARTESIAN_POINT('Ctrl Pts',(-0.100593880386987,-0.0840313287987434,
0.198090806520963));
#41677=CARTESIAN_POINT('Ctrl Pts',(-0.00115024004832317,-0.139008205490464,
0.204870865644395));
#41678=CARTESIAN_POINT('Ctrl Pts',(0.115852970087698,-0.0768289890996742,
0.212776888843912));
#41679=CARTESIAN_POINT('Ctrl Pts',(0.127606135899372,0.055147786219953,
0.22068291204343));
#41680=CARTESIAN_POINT('Ctrl Pts',(0.0234317475993789,0.137023930205902,
0.228588935242947));
#41681=CARTESIAN_POINT('Ctrl Pts',(-0.0916394876575414,0.0979452740831826,
0.235840201719676));
#41682=CARTESIAN_POINT('Ctrl Pts',(-0.11749487688974,0.0292102859676066,
0.240456127129899));
#41683=CARTESIAN_POINT('Ctrl Pts',(-0.117756807889117,-0.000105309437279212,
0.242436711473616));
#41684=CARTESIAN_POINT('Origin',(0.,0.,-0.0924367114736152));
#41685=CARTESIAN_POINT('',(-0.117789487689835,-0.000104112672946744,0.132563288526384));
#41686=CARTESIAN_POINT('',(-0.117915129103549,6.69430946510577E-5,0.142436711473616));
#41687=CARTESIAN_POINT('',(-0.117775,-1.30487598617993E-14,-0.0924367114736152));
#41688=CARTESIAN_POINT('Ctrl Pts',(-0.117789487689835,-0.000104112672946739,
0.132563288526384));
#41689=CARTESIAN_POINT('Ctrl Pts',(-0.117867447370286,-0.00868443076951223,
0.133143392915894));
#41690=CARTESIAN_POINT('Ctrl Pts',(-0.113109713752316,-0.056129702894726,
0.136356901260207));
#41691=CARTESIAN_POINT('Ctrl Pts',(-0.0488717923313075,-0.130102508888041,
0.142203813559322));
#41692=CARTESIAN_POINT('Ctrl Pts',(0.0822642127117346,-0.112016585630158,
0.150104025423729));
#41693=CARTESIAN_POINT('Ctrl Pts',(0.138765526166673,0.00769705224861128,
0.158004237288135));
#41694=CARTESIAN_POINT('Ctrl Pts',(0.0693709963376258,0.12042749084372,
0.165904449152542));
#41695=CARTESIAN_POINT('Ctrl Pts',(-0.0629607791409001,0.123899379163224,
0.173804661016949));
#41696=CARTESIAN_POINT('Ctrl Pts',(-0.115824984153554,0.0473294249038356,
0.179357607474896));
#41697=CARTESIAN_POINT('Ctrl Pts',(-0.117939398554652,0.00429074720192216,
0.182277149978042));
#41698=CARTESIAN_POINT('Ctrl Pts',(-0.117909687164366,6.96645888464118E-5,
0.182563288526384));
#41699=CARTESIAN_POINT('Ctrl Pts',(-0.117915129103549,6.69430946510529E-5,
0.142436711473616));
#41700=CARTESIAN_POINT('Ctrl Pts',(-0.117677363460081,-0.0348022339441635,
0.144800708731668));
#41701=CARTESIAN_POINT('Ctrl Pts',(-0.0828943760199795,-0.108955331093341,
0.149800047056226));
#41702=CARTESIAN_POINT('Ctrl Pts',(0.0429243879661372,-0.132219897211806,
0.15743472644729));
#41703=CARTESIAN_POINT('Ctrl Pts',(0.134218946443888,-0.0361922458912883,
0.165340749646808));
#41704=CARTESIAN_POINT('Ctrl Pts',(0.103578348063976,0.0927153171784346,
0.173246772846325));
#41705=CARTESIAN_POINT('Ctrl Pts',(-0.0211610525014389,0.137392918706172,
0.181152796045843));
#41706=CARTESIAN_POINT('Ctrl Pts',(-0.106531690673769,0.0725519877028229,
0.187549442254939));
#41707=CARTESIAN_POINT('Ctrl Pts',(-0.117658990074321,0.0167661061227608,
0.19131074739753));
#41708=CARTESIAN_POINT('Ctrl Pts',(-0.117601649275994,4.45452448404882E-5,
0.192436711473616));
#41709=CARTESIAN_POINT('Origin',(0.,0.,-0.0924367114736152));
#41710=CARTESIAN_POINT('',(-0.117593357284741,3.06645980543279E-5,0.0825632885263843));
#41711=CARTESIAN_POINT('',(-0.117788324723582,-0.000104604007662518,0.0924367114736157));
#41712=CARTESIAN_POINT('',(-0.117775,-1.30487598617993E-14,-0.0924367114736152));
#41713=CARTESIAN_POINT('Ctrl Pts',(-0.117593357284741,3.06645980543228E-5,
0.0825632885263843));
#41714=CARTESIAN_POINT('Ctrl Pts',(-0.11754301899516,-0.021452746571923,
0.0840096358537477));
#41715=CARTESIAN_POINT('Ctrl Pts',(-0.101655671713158,-0.0821210291969121,
0.0880893871359134));
#41716=CARTESIAN_POINT('Ctrl Pts',(-0.0045529857407016,-0.138904079109577,
0.0948025423728811));
#41717=CARTESIAN_POINT('Ctrl Pts',(0.113850559027731,-0.0797068119457511,
0.102702754237288));
#41718=CARTESIAN_POINT('Ctrl Pts',(0.12896255920279,0.0518052156568057,
0.110602966101695));
#41719=CARTESIAN_POINT('Ctrl Pts',(0.0270724914422277,0.136316505597261,
0.118503177966102));
#41720=CARTESIAN_POINT('Ctrl Pts',(-0.0900940209439092,0.100029588267392,
0.125823285440998));
#41721=CARTESIAN_POINT('Ctrl Pts',(-0.117513546702531,0.0302662202125134,
0.130509988961092));
#41722=CARTESIAN_POINT('Ctrl Pts',(-0.117789487689835,-0.000104112672946739,
0.132563288526384));
#41723=CARTESIAN_POINT('Ctrl Pts',(-0.117788324723582,-0.00010460400766255,
0.0924367114736157));
#41724=CARTESIAN_POINT('Ctrl Pts',(-0.117866887107117,-0.00873205619380746,
0.093019987932794));
#41725=CARTESIAN_POINT('Ctrl Pts',(-0.113075788730874,-0.0562533105277103,
0.0962386054584782));
#41726=CARTESIAN_POINT('Ctrl Pts',(-0.0486330432543111,-0.130228357167641,
0.102092564050668));
#41727=CARTESIAN_POINT('Ctrl Pts',(0.0825817545836372,-0.111825131042891,
0.109998587250186));
#41728=CARTESIAN_POINT('Ctrl Pts',(0.138772738128538,0.00816897019039422,
0.117904610449703));
#41729=CARTESIAN_POINT('Ctrl Pts',(0.0688915313895657,0.120741708772585,
0.12581063364922));
#41730=CARTESIAN_POINT('Ctrl Pts',(-0.0635762130827019,0.123623095373164,
0.133716656848738));
#41731=CARTESIAN_POINT('Ctrl Pts',(-0.115947056638979,0.0469156369390546,
0.139258682790203));
#41732=CARTESIAN_POINT('Ctrl Pts',(-0.117942420266852,0.00406928923237253,
0.142165367665162));
#41733=CARTESIAN_POINT('Ctrl Pts',(-0.117915129103549,6.69430946510529E-5,
0.142436711473616));
#41734=CARTESIAN_POINT('Origin',(0.,0.,-0.0924367114736152));
#41735=CARTESIAN_POINT('',(-0.117896184020664,8.43438525025023E-5,0.0325632885263842));
#41736=CARTESIAN_POINT('',(-0.117591431864639,2.92794590778037E-5,0.0424367114736158));
#41737=CARTESIAN_POINT('',(-0.117775,-1.30487598617993E-14,-0.0924367114736152));
#41738=CARTESIAN_POINT('Ctrl Pts',(-0.117896184020664,8.43438525024954E-5,
0.0325632885263842));
#41739=CARTESIAN_POINT('Ctrl Pts',(-0.117638881596538,-0.0340384192378303,
0.0348758787916007));
#41740=CARTESIAN_POINT('Ctrl Pts',(-0.0841595758608773,-0.107483448399194,
0.0398218730116195));
#41741=CARTESIAN_POINT('Ctrl Pts',(0.040248222246223,-0.133016439153077,
0.0474012711864405));
#41742=CARTESIAN_POINT('Ctrl Pts',(0.133402197487182,-0.0389756054074351,
0.0553014830508473));
#41743=CARTESIAN_POINT('Ctrl Pts',(0.105528454455023,0.0904394425945055,
0.0632016949152541));
#41744=CARTESIAN_POINT('Ctrl Pts',(-0.0180877669633101,0.137795734956694,
0.0711019067796609));
#41745=CARTESIAN_POINT('Ctrl Pts',(-0.105666299933038,0.0743567679416689,
0.0775557713167041));
#41746=CARTESIAN_POINT('Ctrl Pts',(-0.117634671289428,0.017662685017247,
0.0813762318989454));
#41747=CARTESIAN_POINT('Ctrl Pts',(-0.117593357284741,3.06645980543228E-5,
0.0825632885263843));
#41748=CARTESIAN_POINT('Ctrl Pts',(-0.117591431864639,2.92794590778002E-5,
0.0424367114736158));
#41749=CARTESIAN_POINT('Ctrl Pts',(-0.11754501123181,-0.0213296840770181,
0.0438746082004259));
#41750=CARTESIAN_POINT('Ctrl Pts',(-0.101789620521557,-0.0818995216066154,
0.0479478459937417));
#41751=CARTESIAN_POINT('Ctrl Pts',(-0.00489492837772915,-0.138925734589418,
0.0546564248535634));
#41752=CARTESIAN_POINT('Ctrl Pts',(0.113740629398734,-0.0799231888543136,
0.062562448053081));
#41753=CARTESIAN_POINT('Ctrl Pts',(0.129045816271948,0.0516898037714297,
0.0704684712525983));
#41754=CARTESIAN_POINT('Ctrl Pts',(0.0271151839788463,0.136342686033388,
0.0783744944521158));
#41755=CARTESIAN_POINT('Ctrl Pts',(-0.0901114389347958,0.100024405106452,
0.0856972411924549));
#41756=CARTESIAN_POINT('Ctrl Pts',(-0.117511929055312,0.0302482226905713,
0.0903846468662882));
#41757=CARTESIAN_POINT('Ctrl Pts',(-0.117788324723582,-0.00010460400766255,
0.0924367114736157));
#41758=CARTESIAN_POINT('Origin',(0.,0.,0.95));
#41759=CARTESIAN_POINT('',(-0.143203996033626,-2.30855198111598E-5,0.907000235762439));
#41760=CARTESIAN_POINT('Ctrl Pts',(-0.0334019664626807,0.112939183906322,
0.932225));
#41761=CARTESIAN_POINT('Ctrl Pts',(-0.0250603177854857,0.115799805022824,
0.931847596094215));
#41762=CARTESIAN_POINT('Ctrl Pts',(-0.0164278988467134,0.117636476238285,
0.931473565046676));
#41763=CARTESIAN_POINT('Ctrl Pts',(-0.00767106646971057,0.118512486061759,
0.931100514589335));
#41764=CARTESIAN_POINT('Ctrl Pts',(-0.00420439075546036,0.118859282922739,
0.930952830483373));
#41765=CARTESIAN_POINT('Ctrl Pts',(-0.000716143526927236,0.119054988716296,
0.930805221836912));
#41766=CARTESIAN_POINT('Ctrl Pts',(0.00277797710115842,0.119101360153194,
0.930657787404542));
#41767=CARTESIAN_POINT('Ctrl Pts',(0.00969984845123832,0.119193222213692,
0.930365719018224));
#41768=CARTESIAN_POINT('Ctrl Pts',(0.0166142532722655,0.118700388967513,
0.930075608100973));
#41769=CARTESIAN_POINT('Ctrl Pts',(0.02344427759502,0.117646722051856,0.929786344238933));
#41770=CARTESIAN_POINT('Ctrl Pts',(0.0272709497102665,0.117056381869396,
0.929624277765593));
#41771=CARTESIAN_POINT('Ctrl Pts',(0.0310712076772195,0.116289673696229,
0.929462477186978));
#41772=CARTESIAN_POINT('Ctrl Pts',(0.0348314922052066,0.115348424870015,
0.929300747212246));
#41773=CARTESIAN_POINT('Ctrl Pts',(0.0378910930422447,0.114582566415658,
0.929169153668624));
#41774=CARTESIAN_POINT('Ctrl Pts',(0.04092399616764,0.113700812218856,0.929037612549819));
#41775=CARTESIAN_POINT('Ctrl Pts',(0.0439095212807944,0.11270886835725,
0.928906608402292));
#41776=CARTESIAN_POINT('Ctrl Pts',(0.0525514734098646,0.10983757066528,
0.928527401553001));
#41777=CARTESIAN_POINT('Ctrl Pts',(0.0608263773706973,0.106040058117234,
0.928151455604188));
#41778=CARTESIAN_POINT('Ctrl Pts',(0.0685605494008651,0.101344813008116,
0.927776330408337));
#41779=CARTESIAN_POINT('Ctrl Pts',(0.072435687838791,0.0989923020054058,
0.927588377249316));
#41780=CARTESIAN_POINT('Ctrl Pts',(0.0761749070710193,0.0964136602636579,
0.92740063013395));
#41781=CARTESIAN_POINT('Ctrl Pts',(0.0797540201577765,0.0936080366646606,
0.927212782134414));
#41782=CARTESIAN_POINT('Ctrl Pts',(0.0820668650566089,0.091795025432075,
0.927091393601291));
#41783=CARTESIAN_POINT('Ctrl Pts',(0.0843049421929101,0.089893314502136,
0.926970374334797));
#41784=CARTESIAN_POINT('Ctrl Pts',(0.0864667806566824,0.087910346105634,
0.926849671848167));
#41785=CARTESIAN_POINT('Ctrl Pts',(0.0931618700565369,0.0817692070177022,
0.9264758631884));
#41786=CARTESIAN_POINT('Ctrl Pts',(0.0991298287989589,0.0748505421836024,
0.926105008552812));
#41787=CARTESIAN_POINT('Ctrl Pts',(0.104322127839002,0.0673319773813505,
0.925734762248716));
#41788=CARTESIAN_POINT('Ctrl Pts',(0.106370940812892,0.0643652505050492,
0.925588667922192));
#41789=CARTESIAN_POINT('Ctrl Pts',(0.108298617033319,0.0613046783141235,
0.925442668312145));
#41790=CARTESIAN_POINT('Ctrl Pts',(0.110100560923862,0.0581597986785966,
0.925296619306966));
#41791=CARTESIAN_POINT('Ctrl Pts',(0.11158855048605,0.0555628542917283,
0.925176016553231));
#41792=CARTESIAN_POINT('Ctrl Pts',(0.112988026000293,0.0529128751968171,
0.925055591079489));
#41793=CARTESIAN_POINT('Ctrl Pts',(0.114293875604956,0.0502227205878152,
0.92493557115538));
#41794=CARTESIAN_POINT('Ctrl Pts',(0.118434599880109,0.0416924974643938,
0.924554999448279));
#41795=CARTESIAN_POINT('Ctrl Pts',(0.121649070098747,0.0327401005258095,
0.924177564198185));
#41796=CARTESIAN_POINT('Ctrl Pts',(0.123868271499824,0.0235442585075687,
0.923800796649243));
#41797=CARTESIAN_POINT('Ctrl Pts',(0.124741985203477,0.0199237970280188,
0.923652460869335));
#41798=CARTESIAN_POINT('Ctrl Pts',(0.125460929083487,0.0162653271532848,
0.923504228586243));
#41799=CARTESIAN_POINT('Ctrl Pts',(0.126018750659753,0.0125790928555092,
0.923355949140843));
#41800=CARTESIAN_POINT('Ctrl Pts',(0.126424880564737,0.00989527772751904,
0.923247992188954));
#41801=CARTESIAN_POINT('Ctrl Pts',(0.126745061646254,0.00719882962072188,
0.923140094926841));
#41802=CARTESIAN_POINT('Ctrl Pts',(0.126976603796028,0.00450277675306522,
0.923032557085152));
#41803=CARTESIAN_POINT('Ctrl Pts',(0.12757677314312,-0.00248553311139155,
0.922753813382129));
#41804=CARTESIAN_POINT('Ctrl Pts',(0.127585234929588,-0.00948784607823892,
0.922476804764986));
#41805=CARTESIAN_POINT('Ctrl Pts',(0.126969800827767,-0.0164342950540157,
0.922200564268829));
#41806=CARTESIAN_POINT('Ctrl Pts',(0.126365890166078,-0.0232506781321251,
0.921929496123068));
#41807=CARTESIAN_POINT('Ctrl Pts',(0.125161228392162,-0.0300136540166471,
0.921659167602865));
#41808=CARTESIAN_POINT('Ctrl Pts',(0.123399407242885,-0.0366692095497128,
0.921388665049245));
#41809=CARTESIAN_POINT('Ctrl Pts',(0.122693706044386,-0.0393351064361743,
0.921280314677605));
#41810=CARTESIAN_POINT('Ctrl Pts',(0.121898903213358,-0.0419812756064514,
0.921172034233936));
#41811=CARTESIAN_POINT('Ctrl Pts',(0.121020997998916,-0.0445959600773696,
0.921064109665588));
#41812=CARTESIAN_POINT('Ctrl Pts',(0.118352374694664,-0.0525439797468811,
0.920736044615448));
#41813=CARTESIAN_POINT('Ctrl Pts',(0.11491247387436,-0.0602240203343106,
0.920410355973602));
#41814=CARTESIAN_POINT('Ctrl Pts',(0.110787244183297,-0.067540847099726,
0.920085467703143));
#41815=CARTESIAN_POINT('Ctrl Pts',(0.108602638591366,-0.0714156327150692,
0.919913416014983));
#41816=CARTESIAN_POINT('Ctrl Pts',(0.106225299026755,-0.0751884756223749,
0.919741588788067));
#41817=CARTESIAN_POINT('Ctrl Pts',(0.103664831029184,-0.0788439383503402,
0.919569751954905));
#41818=CARTESIAN_POINT('Ctrl Pts',(0.101376332819864,-0.0821111222851215,
0.919416167420609));
#41819=CARTESIAN_POINT('Ctrl Pts',(0.0989387376213173,-0.0852871325232165,
0.919262431231772));
#41820=CARTESIAN_POINT('Ctrl Pts',(0.0963759957044455,-0.088340202919688,
0.919109404658397));
#41821=CARTESIAN_POINT('Ctrl Pts',(0.0909694481938422,-0.0947811832006395,
0.918786568623332));
#41822=CARTESIAN_POINT('Ctrl Pts',(0.0849957607581912,-0.100695240401247,
0.918466028662098));
#41823=CARTESIAN_POINT('Ctrl Pts',(0.0785257616471073,-0.105984325129946,
0.918146284163942));
#41824=CARTESIAN_POINT('Ctrl Pts',(0.0742361136603187,-0.109491019840235,
0.917934291655249));
#41825=CARTESIAN_POINT('Ctrl Pts',(0.0697277556719998,-0.112722769515888,
0.917722648813756));
#41826=CARTESIAN_POINT('Ctrl Pts',(0.0650165017469215,-0.115645838880061,
0.917510918298299));
#41827=CARTESIAN_POINT('Ctrl Pts',(0.0626218558869296,-0.117131582604068,
0.917403299475299));
#41828=CARTESIAN_POINT('Ctrl Pts',(0.0601741524651638,-0.118537526250906,
0.917295638036625));
#41829=CARTESIAN_POINT('Ctrl Pts',(0.0576864529767728,-0.119853555264988,
0.917188346403244));
#41830=CARTESIAN_POINT('Ctrl Pts',(0.0492417976832846,-0.12432090006769,
0.916824138079852));
#41831=CARTESIAN_POINT('Ctrl Pts',(0.0403105010214407,-0.127774185485052,
0.916462909477301));
#41832=CARTESIAN_POINT('Ctrl Pts',(0.0310751541446225,-0.130251129571305,
0.916102510949096));
#41833=CARTESIAN_POINT('Ctrl Pts',(0.0264632552530831,-0.131488052865922,
0.91592253702988));
#41834=CARTESIAN_POINT('Ctrl Pts',(0.0217750625284288,-0.132480793424065,
0.915742770110557));
#41835=CARTESIAN_POINT('Ctrl Pts',(0.0170316000051624,-0.133229777506063,
0.915562942492132));
#41836=CARTESIAN_POINT('Ctrl Pts',(0.0138158762359995,-0.133737534424853,
0.91544103240133));
#41837=CARTESIAN_POINT('Ctrl Pts',(0.0105740209053218,-0.134132938348625,
0.915319069467609));
#41838=CARTESIAN_POINT('Ctrl Pts',(0.0073287749381158,-0.134414943979412,
0.91519757274014));
#41839=CARTESIAN_POINT('Ctrl Pts',(-0.00265707911089655,-0.135282695483764,
0.91482371861623));
#41840=CARTESIAN_POINT('Ctrl Pts',(-0.0127097596984602,-0.135087239355917,
0.914452927180717));
#41841=CARTESIAN_POINT('Ctrl Pts',(-0.0226366995613315,-0.13384562451132,
0.914082871556714));
#41842=CARTESIAN_POINT('Ctrl Pts',(-0.0278509024051071,-0.133193456598246,
0.913888496944428));
#41843=CARTESIAN_POINT('Ctrl Pts',(-0.0330306231776361,-0.132251796770583,
0.913694325339435));
#41844=CARTESIAN_POINT('Ctrl Pts',(-0.0381476304341873,-0.131017345860063,
0.913500019539069));
#41845=CARTESIAN_POINT('Ctrl Pts',(-0.0414017963667409,-0.130232295556825,
0.913376450569093));
#41846=CARTESIAN_POINT('Ctrl Pts',(-0.0446227244193663,-0.129330489295675,
0.913253123242388));
#41847=CARTESIAN_POINT('Ctrl Pts',(-0.0477977620148837,-0.128314174106561,
0.913130170982833));
#41848=CARTESIAN_POINT('Ctrl Pts',(-0.0560508514351662,-0.125672397471604,
0.912810572879819));
#41849=CARTESIAN_POINT('Ctrl Pts',(-0.0640066574241223,-0.122256042832264,
0.912493045231938));
#41850=CARTESIAN_POINT('Ctrl Pts',(-0.0715409466919047,-0.118061015146759,
0.912176128537659));
#41851=CARTESIAN_POINT('Ctrl Pts',(-0.0762921378140006,-0.11541559265395,
0.911976277996913));
#41852=CARTESIAN_POINT('Ctrl Pts',(-0.080875618778813,-0.112459902541578,
0.911776670412738));
#41853=CARTESIAN_POINT('Ctrl Pts',(-0.0852772318261866,-0.109220115387155,
0.911576939781678));
#41854=CARTESIAN_POINT('Ctrl Pts',(-0.0875530243079477,-0.107545028738423,
0.911473671851569));
#41855=CARTESIAN_POINT('Ctrl Pts',(-0.0897785308463731,-0.105794887026521,
0.911370439409319));
#41856=CARTESIAN_POINT('Ctrl Pts',(-0.0919449058640415,-0.10397965349885,
0.911267529872683));
#41857=CARTESIAN_POINT('Ctrl Pts',(-0.0992562147283688,-0.0978534136403538,
0.910920220011141));
#41858=CARTESIAN_POINT('Ctrl Pts',(-0.105919754790705,-0.0909713378622389,
0.910575510440108));
#41859=CARTESIAN_POINT('Ctrl Pts',(-0.111868517901189,-0.0834835697610656,
0.910231536759666));
#41860=CARTESIAN_POINT('Ctrl Pts',(-0.115372944257836,-0.0790725129751651,
0.910028901285812));
#41861=CARTESIAN_POINT('Ctrl Pts',(-0.118628912335923,-0.0744505089078481,
0.909826521196012));
#41862=CARTESIAN_POINT('Ctrl Pts',(-0.121618006629831,-0.0696436476859399,
0.90962401532803));
#41863=CARTESIAN_POINT('Ctrl Pts',(-0.123117391998195,-0.0672324365713985,
0.90952243461307));
#41864=CARTESIAN_POINT('Ctrl Pts',(-0.124548834320201,-0.0647754742963825,
0.909420860177745));
#41865=CARTESIAN_POINT('Ctrl Pts',(-0.125905418138961,-0.0622851116177192,
0.9093196043405));
#41866=CARTESIAN_POINT('Ctrl Pts',(-0.130761030150815,-0.0533713719953201,
0.908957179953008));
#41867=CARTESIAN_POINT('Ctrl Pts',(-0.134679363933253,-0.0440025983801541,
0.908597596571227));
#41868=CARTESIAN_POINT('Ctrl Pts',(-0.13756687326497,-0.0343371686472044,
0.908238737834252));
#41869=CARTESIAN_POINT('Ctrl Pts',(-0.139097796244526,-0.0292126731787653,
0.908048475215596));
#41870=CARTESIAN_POINT('Ctrl Pts',(-0.14033830847868,-0.0240043037722782,
0.907858416294146));
#41871=CARTESIAN_POINT('Ctrl Pts',(-0.14126916593033,-0.0187337321988357,
0.90766824565692));
#41872=CARTESIAN_POINT('Ctrl Pts',(-0.141766581419635,-0.0159173354095375,
0.907566625564177));
#41873=CARTESIAN_POINT('Ctrl Pts',(-0.142175147764435,-0.0130838950804596,
0.90746500095103));
#41874=CARTESIAN_POINT('Ctrl Pts',(-0.142491067194012,-0.010247236235083,
0.907363696319434));
#41875=CARTESIAN_POINT('Ctrl Pts',(-0.142699030773042,-0.00837991922086784,
0.907297009462638));
#41876=CARTESIAN_POINT('Ctrl Pts',(-0.142867069971313,-0.00651002641398622,
0.907230418639425));
#41877=CARTESIAN_POINT('Ctrl Pts',(-0.142994592382579,-0.00463854690639179,
0.907163910672075));
#41878=CARTESIAN_POINT('Ctrl Pts',(-0.143099304951117,-0.00310181760319464,
0.907109298937397));
#41879=CARTESIAN_POINT('Ctrl Pts',(-0.143176698406437,-0.00156401794929073,
0.907054743068754));
#41880=CARTESIAN_POINT('Ctrl Pts',(-0.143227225569541,-2.57112916194508E-5,
0.907000235770274));
#41881=CARTESIAN_POINT('',(-0.00156150813732516,0.146115848505824,0.90365));
#41882=CARTESIAN_POINT('Ctrl Pts',(-0.00156268643911937,0.146080787864432,
0.90365));
#41883=CARTESIAN_POINT('Ctrl Pts',(-0.0117053345256504,0.14465327094795,
0.904950888122905));
#41884=CARTESIAN_POINT('Ctrl Pts',(-0.0216455209286645,0.142222180286059,
0.906261527257655));
#41885=CARTESIAN_POINT('Ctrl Pts',(-0.0312038210265984,0.138800205489803,
0.907591018110418));
#41886=CARTESIAN_POINT('Ctrl Pts',(-0.0379790896742497,0.136374586047791,
0.908533409288742));
#41887=CARTESIAN_POINT('Ctrl Pts',(-0.0445622616029078,0.133450051590279,
0.909485272488055));
#41888=CARTESIAN_POINT('Ctrl Pts',(-0.0508780053273359,0.130018961446113,
0.910449848959387));
#41889=CARTESIAN_POINT('Ctrl Pts',(-0.0536010334441123,0.128539649532677,
0.910865725373444));
#41890=CARTESIAN_POINT('Ctrl Pts',(-0.0562660125378511,0.126970478129068,
0.911282720586817));
#41891=CARTESIAN_POINT('Ctrl Pts',(-0.058866712211968,0.125312368815247,
0.911700977969885));
#41892=CARTESIAN_POINT('Ctrl Pts',(-0.0626444387166601,0.12290383100335,
0.912308530628704));
#41893=CARTESIAN_POINT('Ctrl Pts',(-0.0662873724862372,0.120307303169936,
0.912918858991888));
#41894=CARTESIAN_POINT('Ctrl Pts',(-0.069778152687478,0.117522359853825,
0.913532898033536));
#41895=CARTESIAN_POINT('Ctrl Pts',(-0.0759775260377567,0.112576501798998,
0.914623386993416));
#41896=CARTESIAN_POINT('Ctrl Pts',(-0.081698277829649,0.107036582207071,
0.915725579133695));
#41897=CARTESIAN_POINT('Ctrl Pts',(-0.0868900966390514,0.100989570353443,
0.916844711368391));
#41898=CARTESIAN_POINT('Ctrl Pts',(-0.0896166640492451,0.0978138845187795,
0.917432441717011));
#41899=CARTESIAN_POINT('Ctrl Pts',(-0.0921993947360654,0.0944939977198656,
0.918025537507845));
#41900=CARTESIAN_POINT('Ctrl Pts',(-0.0946128443867119,0.0910668838926417,
0.918620601845101));
#41901=CARTESIAN_POINT('Ctrl Pts',(-0.0989927195077328,0.0848474334123951,
0.919700511461385));
#41902=CARTESIAN_POINT('Ctrl Pts',(-0.102828650181205,0.0782631455551165,
0.92078926141647));
#41903=CARTESIAN_POINT('Ctrl Pts',(-0.106079098770626,0.0713949254017264,
0.921892245864136));
#41904=CARTESIAN_POINT('Ctrl Pts',(-0.108178735463834,0.0669583786746003,
0.922604721866953));
#41905=CARTESIAN_POINT('Ctrl Pts',(-0.110033655020259,0.062403198537532,
0.923323137285097));
#41906=CARTESIAN_POINT('Ctrl Pts',(-0.111627678155428,0.0577512547785083,
0.92404894598959));
#41907=CARTESIAN_POINT('Ctrl Pts',(-0.112967174079103,0.0538421147134128,
0.924658860475512));
#41908=CARTESIAN_POINT('Ctrl Pts',(-0.114123078730198,0.049859612891567,
0.925274762706783));
#41909=CARTESIAN_POINT('Ctrl Pts',(-0.11507803961208,0.0458466780964684,
0.925893033154576));
#41910=CARTESIAN_POINT('Ctrl Pts',(-0.117097308962912,0.0373613082845972,
0.92720036897266));
#41911=CARTESIAN_POINT('Ctrl Pts',(-0.118230954345967,0.0287177049851521,
0.928521669794669));
#41912=CARTESIAN_POINT('Ctrl Pts',(-0.118391771793402,0.020045083810393,
0.929866742826164));
#41913=CARTESIAN_POINT('Ctrl Pts',(-0.11848473133085,0.0150319284238029,
0.930644254028062));
#41914=CARTESIAN_POINT('Ctrl Pts',(-0.118251755364909,0.0100092161799773,
0.931429708350036));
#41915=CARTESIAN_POINT('Ctrl Pts',(-0.11766859746431,0.00500517689817996,
0.932225));
#41916=CARTESIAN_POINT('',(-0.115101970897782,0.0902398078595341,0.90365));
#41917=CARTESIAN_POINT('Origin',(0.,0.,0.90365));
#41918=CARTESIAN_POINT('Ctrl Pts',(-0.143227225569541,-2.57112916194508E-5,
0.907000235770274));
#41919=CARTESIAN_POINT('Ctrl Pts',(-0.143488833522934,0.00793898000868948,
0.90671802038504));
#41920=CARTESIAN_POINT('Ctrl Pts',(-0.143031870701996,0.0159171358242676,
0.906437106818573));
#41921=CARTESIAN_POINT('Ctrl Pts',(-0.141906651187533,0.0238323323994448,
0.906156482679268));
#41922=CARTESIAN_POINT('Ctrl Pts',(-0.141282697379586,0.0282214466835871,
0.906000871709079));
#41923=CARTESIAN_POINT('Ctrl Pts',(-0.140452894046849,0.0325912439394045,
0.905845349734719));
#41924=CARTESIAN_POINT('Ctrl Pts',(-0.139423292881505,0.0369284672537908,
0.905689744135006));
#41925=CARTESIAN_POINT('Ctrl Pts',(-0.13875911501036,0.0397263348598034,
0.905589365658919));
#41926=CARTESIAN_POINT('Ctrl Pts',(-0.138011948498085,0.0425090563696419,
0.905489007617642));
#41927=CARTESIAN_POINT('Ctrl Pts',(-0.13718658538945,0.0452640319758816,
0.905388954073411));
#41928=CARTESIAN_POINT('Ctrl Pts',(-0.134156179660795,0.0553792088866476,
0.905021597172627));
#41929=CARTESIAN_POINT('Ctrl Pts',(-0.130067939373984,0.0651554859252432,
0.904657113682601));
#41930=CARTESIAN_POINT('Ctrl Pts',(-0.125020727014944,0.07442120635967,
0.904293300817012));
#41931=CARTESIAN_POINT('Ctrl Pts',(-0.122044721725445,0.0798845851641063,
0.904078784578074));
#41932=CARTESIAN_POINT('Ctrl Pts',(-0.118734281499311,0.0851703778496932,
0.903864501493536));
#41933=CARTESIAN_POINT('Ctrl Pts',(-0.115101970897782,0.0902398078595341,
0.90365));
#41934=CARTESIAN_POINT('',(-0.05,-6.12323399573676E-18,1.));
#41935=CARTESIAN_POINT('',(-0.1,-1.22464679914735E-17,0.95));
#41936=CARTESIAN_POINT('Origin',(0.,0.,1.));
#41937=CARTESIAN_POINT('Ctrl Pts',(0.0850780204044548,-0.119080027477571,
-0.0164977839420937));
#41938=CARTESIAN_POINT('Ctrl Pts',(0.124484376148786,-0.090925728145445,
-0.0138643799872915));
#41939=CARTESIAN_POINT('Ctrl Pts',(0.17250686669983,0.00706609547096537,
-0.00859757207768696));
#41940=CARTESIAN_POINT('Ctrl Pts',(0.0881701387729916,0.148625694711589,
-0.000697360213280174));
#41941=CARTESIAN_POINT('Ctrl Pts',(-0.0762274913006873,0.154908116339636,
0.00720285165112661));
#41942=CARTESIAN_POINT('Ctrl Pts',(-0.171431501518862,0.0208683089584473,
0.0151030635155334));
#41943=CARTESIAN_POINT('Ctrl Pts',(-0.111122107950137,-0.132218525770778,
0.0230032753799401));
#41944=CARTESIAN_POINT('Ctrl Pts',(0.050013392704176,-0.165289372702636,
0.030903487244347));
#41945=CARTESIAN_POINT('Ctrl Pts',(0.165768725130536,-0.0484320089270095,
0.0388036991087536));
#41946=CARTESIAN_POINT('Ctrl Pts',(0.131132152914396,0.112382189969905,
0.0467039109731606));
#41947=CARTESIAN_POINT('Ctrl Pts',(-0.0224762869461261,0.171228238683186,
0.0546041228375672));
#41948=CARTESIAN_POINT('Ctrl Pts',(-0.155692220471689,0.0747310615070771,
0.062504334701974));
#41949=CARTESIAN_POINT('Ctrl Pts',(-0.147655869299913,-0.0895687367181161,
0.0704045465663809));
#41950=CARTESIAN_POINT('Ctrl Pts',(-0.00565764774487061,-0.172605493336333,
0.0783047584307876));
#41951=CARTESIAN_POINT('Ctrl Pts',(0.141473396847448,-0.0990455693335685,
0.0862049702951944));
#41952=CARTESIAN_POINT('Ctrl Pts',(0.160251925615185,0.0643743860018943,
0.0941051821596012));
#41953=CARTESIAN_POINT('Ctrl Pts',(0.0336409180434769,0.169390113302136,
0.102005394024008));
#41954=CARTESIAN_POINT('Ctrl Pts',(-0.123490994764231,0.120725758497873,
0.109905605888415));
#41955=CARTESIAN_POINT('Ctrl Pts',(-0.168584982150601,-0.0374678050106281,
0.117805817752822));
#41956=CARTESIAN_POINT('Ctrl Pts',(-0.0607292448116094,-0.16166845405022,
0.125706029617228));
#41957=CARTESIAN_POINT('Ctrl Pts',(0.102223455999678,-0.139194458136055,
0.133606241481635));
#41958=CARTESIAN_POINT('Ctrl Pts',(0.172433324173149,0.00956453913465353,
0.141506453346042));
#41959=CARTESIAN_POINT('Ctrl Pts',(0.086202040450112,0.149646047845283,
0.149406665210448));
#41960=CARTESIAN_POINT('Ctrl Pts',(-0.0782365529804317,0.153960298370095,
0.157306877074856));
#41961=CARTESIAN_POINT('Ctrl Pts',(-0.171694572067167,0.0185931582621336,
0.165207088939262));
#41962=CARTESIAN_POINT('Ctrl Pts',(-0.109381677027807,-0.133642733856025,
0.173107300803669));
#41963=CARTESIAN_POINT('Ctrl Pts',(0.052168390130379,-0.164630467088263,
0.181007512668076));
#41964=CARTESIAN_POINT('Ctrl Pts',(0.166388377416592,-0.04625623707159,
0.188907724532483));
#41965=CARTESIAN_POINT('Ctrl Pts',(0.129651527078137,0.114084236996722,
0.19680793639689));
#41966=CARTESIAN_POINT('Ctrl Pts',(-0.0247124365344563,0.170921113648968,
0.204708148261296));
#41967=CARTESIAN_POINT('Ctrl Pts',(-0.156655896226217,0.072688800963294,
0.212608360125703));
#41968=CARTESIAN_POINT('Ctrl Pts',(-0.146472369316595,-0.0914908554698463,
0.22050857199011));
#41969=CARTESIAN_POINT('Ctrl Pts',(-0.00340092071136592,-0.172664893209074,
0.228408783854516));
#41970=CARTESIAN_POINT('Ctrl Pts',(0.142756033285632,-0.0971876873308804,
0.236308995718923));
#41971=CARTESIAN_POINT('Ctrl Pts',(0.159396733387471,0.0664636215805494,
0.24420920758333));
#41972=CARTESIAN_POINT('Ctrl Pts',(0.0314238061962717,0.169815417475675,
0.252109419447737));
#41973=CARTESIAN_POINT('Ctrl Pts',(-0.12505855466298,0.119101173436036,
0.260009631312144));
#41974=CARTESIAN_POINT('Ctrl Pts',(-0.168080803576887,-0.0396683132637571,
0.26790984317655));
#41975=CARTESIAN_POINT('Ctrl Pts',(-0.0586107512557457,-0.162448488590979,
0.275810055040957));
#41976=CARTESIAN_POINT('Ctrl Pts',(0.104034251124571,-0.137846313701876,
0.283710266905363));
#41977=CARTESIAN_POINT('Ctrl Pts',(0.172293565052386,0.0118177430073507,
0.291610478769771));
#41978=CARTESIAN_POINT('Ctrl Pts',(0.084238525028331,0.150760082612412,
0.299510690634177));
#41979=CARTESIAN_POINT('Ctrl Pts',(-0.0802424140921812,0.15292444732255,
0.307410902498584));
#41980=CARTESIAN_POINT('Ctrl Pts',(-0.171922949352315,0.0163472044781485,
0.315311114362991));
#41981=CARTESIAN_POINT('Ctrl Pts',(-0.107625373942229,-0.135061136127476,
0.323211326227398));
#41982=CARTESIAN_POINT('Ctrl Pts',(0.0543159572952621,-0.163934463708362,
0.331111538091804));
#41983=CARTESIAN_POINT('Ctrl Pts',(0.166978815646636,-0.0440772813759624,
0.339011749956212));
#41984=CARTESIAN_POINT('Ctrl Pts',(0.128149157817753,0.11576927467532,0.346911961820618));
#41985=CARTESIAN_POINT('Ctrl Pts',(-0.0269445799125943,0.17058347288522,
0.354812173685025));
#41986=CARTESIAN_POINT('Ctrl Pts',(-0.157592688461949,0.070634808356674,
0.362712385549432));
#41987=CARTESIAN_POINT('Ctrl Pts',(-0.145263900126163,-0.0933977030145032,
0.370612597413839));
#41988=CARTESIAN_POINT('Ctrl Pts',(-0.00114358090037083,-0.172694596994154,
0.378512809278245));
#41989=CARTESIAN_POINT('Ctrl Pts',(0.144014258847901,-0.0953132984254496,
0.386413021142653));
#41990=CARTESIAN_POINT('Ctrl Pts',(0.15851431213257,0.0685415527792242,
0.394313233007058));
#41991=CARTESIAN_POINT('Ctrl Pts',(0.0292013200165327,0.170211675620508,
0.402213444871466));
#41992=CARTESIAN_POINT('Ctrl Pts',(-0.126604742061452,0.117456250986493,
0.410113656735872));
#41993=CARTESIAN_POINT('Ctrl Pts',(-0.167547904549645,-0.0418620507055259,
0.418013868600279));
#41994=CARTESIAN_POINT('Ctrl Pts',(-0.0564822415909637,-0.163200759781041,
0.425914080464686));
#41995=CARTESIAN_POINT('Ctrl Pts',(0.105827268468801,-0.136474616162425,
0.433814292329093));
#41996=CARTESIAN_POINT('Ctrl Pts',(0.172124364506242,0.0140689285864832,
0.441714504193499));
#41997=CARTESIAN_POINT('Ctrl Pts',(0.0822606147860967,0.15184835482567,
0.449614716057907));
#41998=CARTESIAN_POINT('Ctrl Pts',(-0.0822345632875265,0.151862464780335,
0.457514927922313));
#41999=CARTESIAN_POINT('Ctrl Pts',(-0.172121948383532,0.0140984571108209,
0.465415139786721));
#42000=CARTESIAN_POINT('Ctrl Pts',(-0.105850679763545,-0.13645645899643,
0.473315351651126));
#42001=CARTESIAN_POINT('Ctrl Pts',(0.0564542429141223,-0.163210447169421,
0.481215563515534));
#42002=CARTESIAN_POINT('Ctrl Pts',(0.167540720455548,-0.0418907937079863,
0.48911577537994));
#42003=CARTESIAN_POINT('Ctrl Pts',(0.126624890361875,0.117434529628606,
0.497015987244348));
#42004=CARTESIAN_POINT('Ctrl Pts',(-0.0291721189860838,0.170216682737359,
0.504916199108753));
#42005=CARTESIAN_POINT('Ctrl Pts',(-0.158502551179345,0.068568745634494,
0.512816410973161));
#42006=CARTESIAN_POINT('Ctrl Pts',(-0.14403060816614,-0.0952885907102249,
0.520716622837567));
#42007=CARTESIAN_POINT('Ctrl Pts',(0.00111395432615138,-0.172694790639464,
0.528616834701974));
#42008=CARTESIAN_POINT('Ctrl Pts',(0.145247875180311,-0.0934226223344961,
0.536517046566381));
#42009=CARTESIAN_POINT('Ctrl Pts',(0.157604803871184,0.0706077715621608,
0.544417258430788));
#42010=CARTESIAN_POINT('Ctrl Pts',(0.0269738439003715,0.170578847907609,
0.552317470295194));
#42011=CARTESIAN_POINT('Ctrl Pts',(-0.128129295177092,0.11579125755285,
0.560217682159602));
#42012=CARTESIAN_POINT('Ctrl Pts',(-0.166986374851081,-0.0440486347386962,
0.568117894024008));
#42013=CARTESIAN_POINT('Ctrl Pts',(-0.0543440802119571,-0.163925143142123,
0.576018105888415));
#42014=CARTESIAN_POINT('Ctrl Pts',(0.107602201995467,-0.135079597771001,
0.583918317752822));
#42015=CARTESIAN_POINT('Ctrl Pts',(0.171925751260969,0.0163177100599224,
0.591818529617229));
#42016=CARTESIAN_POINT('Ctrl Pts',(0.0802686478080903,0.152910679114674,
0.599718741481635));
#42017=CARTESIAN_POINT('Ctrl Pts',(-0.0842126601987931,0.150774531902743,
0.607618953346042));
#42018=CARTESIAN_POINT('Ctrl Pts',(-0.172291535128485,0.0118473005919646,
0.615519165210449));
#42019=CARTESIAN_POINT('Ctrl Pts',(-0.104057897766774,-0.137828464116146,
0.623419377074855));
#42020=CARTESIAN_POINT('Ctrl Pts',(0.0585828816032124,-0.162458541146064,
0.631319588939263));
#42021=CARTESIAN_POINT('Ctrl Pts',(0.168073995820709,-0.0396971477198862,
0.639219800803669));
#42022=CARTESIAN_POINT('Ctrl Pts',(0.12507898518031,0.119079717309719,0.647120012668075));
#42023=CARTESIAN_POINT('Ctrl Pts',(-0.0313946731132146,0.169820805875821,
0.655020224532484));
#42024=CARTESIAN_POINT('Ctrl Pts',(-0.159385328899637,0.0664909658504678,
0.662920436396888));
#42025=CARTESIAN_POINT('Ctrl Pts',(-0.142772704183121,-0.0971631954436711,
0.670820648261297));
#42026=CARTESIAN_POINT('Ctrl Pts',(0.00337129920097031,-0.172665474109675,
0.678720860125702));
#42027=CARTESIAN_POINT('Ctrl Pts',(0.146456671479165,-0.0915159821406338,
0.68662107199011));
#42028=CARTESIAN_POINT('Ctrl Pts',(0.156668364025577,0.0726619248576747,
0.694521283854517));
#42029=CARTESIAN_POINT('Ctrl Pts',(0.0247417584705585,0.17091687158558,
0.702421495718924));
#42030=CARTESIAN_POINT('Ctrl Pts',(-0.129631953475511,0.114106477666574,
0.71032170758333));
#42031=CARTESIAN_POINT('Ctrl Pts',(-0.166396310469803,-0.0462276917499887,
0.718221919447737));
#42032=CARTESIAN_POINT('Ctrl Pts',(-0.0521966324240299,-0.164621514831807,
0.726122131312144));
#42033=CARTESIAN_POINT('Ctrl Pts',(0.109358748279947,-0.133661497021884,
0.73402234317655));
#42034=CARTESIAN_POINT('Ctrl Pts',(0.171697759489448,0.0185637033690059,
0.741922555040957));
#42035=CARTESIAN_POINT('Ctrl Pts',(0.0782629640387094,0.153946873541983,
0.749822766905365));
#42036=CARTESIAN_POINT('Ctrl Pts',(-0.0861763659646394,0.149660835369141,
0.75772297876977));
#42037=CARTESIAN_POINT('Ctrl Pts',(-0.17243168220941,0.00959411813254083,
0.765623190634177));
#42038=CARTESIAN_POINT('Ctrl Pts',(-0.102247331262163,-0.139176914249964,
0.773523402498585));
#42039=CARTESIAN_POINT('Ctrl Pts',(0.0607015038436091,-0.161678879418918,
0.78142361436299));
#42040=CARTESIAN_POINT('Ctrl Pts',(0.168578561585846,-0.0374967082074332,
0.7893238262274));
#42041=CARTESIAN_POINT('Ctrl Pts',(0.123511685603348,0.120704537490262,
0.797224038091803));
#42042=CARTESIAN_POINT('Ctrl Pts',(-0.0336118229326868,0.169395946219611,
0.805124249956213));
#42043=CARTESIAN_POINT('Ctrl Pts',(-0.16024094592625,0.0644017551688373,
0.813024461820617));
#42044=CARTESIAN_POINT('Ctrl Pts',(-0.141490260395339,-0.0990210660472952,
0.820924673685026));
#42045=CARTESIAN_POINT('Ctrl Pts',(0.0056277969043301,-0.172606900899112,
0.828824885549431));
#42046=CARTESIAN_POINT('Ctrl Pts',(0.147640956035951,-0.0895932317207615,
0.836725097413839));
#42047=CARTESIAN_POINT('Ctrl Pts',(0.15570417479137,0.0747027653435218,
0.844625309278246));
#42048=CARTESIAN_POINT('Ctrl Pts',(0.022507302267937,0.171227391193745,
0.852525521142652));
#42049=CARTESIAN_POINT('Ctrl Pts',(-0.131115987327984,0.112398966130108,
0.860425733007058));
#42050=CARTESIAN_POINT('Ctrl Pts',(-0.16577111303378,-0.0483927087664539,
0.868325944871467));
#42051=CARTESIAN_POINT('Ctrl Pts',(-0.050052991301314,-0.165301420121155,
0.876226156735872));
#42052=CARTESIAN_POINT('Ctrl Pts',(0.111120800514148,-0.132198387754511,
0.884126368600279));
#42053=CARTESIAN_POINT('Ctrl Pts',(0.171394279774569,0.0207642914265632,
0.892026580464686));
#42054=CARTESIAN_POINT('Ctrl Pts',(0.0763332480962674,0.155038078338273,
0.899926792329093));
#42055=CARTESIAN_POINT('Ctrl Pts',(-0.0883093241020301,0.148357716484315,
0.9078270041935));
#42056=CARTESIAN_POINT('Ctrl Pts',(-0.14415958729081,0.0546064221138428,
0.913093812103104));
#42057=CARTESIAN_POINT('Ctrl Pts',(-0.146217781693074,0.00621955117001918,
0.915727216057906));
#42058=CARTESIAN_POINT('Ctrl Pts',(0.0795408277542851,-0.111329858282328,
-0.0109985226280626));
#42059=CARTESIAN_POINT('Ctrl Pts',(0.116382471927282,-0.0850079450187934,
-0.00836511867326029));
#42060=CARTESIAN_POINT('Ctrl Pts',(0.161279480944341,0.00660620780878029,
-0.00309831076365578));
#42061=CARTESIAN_POINT('Ctrl Pts',(0.0824316996078882,0.138952584071836,
0.00480190110075102));
#42062=CARTESIAN_POINT('Ctrl Pts',(-0.0712663238620885,0.144826122433691,
0.0127021129651578));
#42063=CARTESIAN_POINT('Ctrl Pts',(-0.160274104511912,0.0195101221266785,
0.0206023248295645));
#42064=CARTESIAN_POINT('Ctrl Pts',(-0.103889869629501,-0.123613254448834,
0.0285025366939713));
#42065=CARTESIAN_POINT('Ctrl Pts',(0.0467583358848584,-0.154531728186116,
0.0364027485583782));
#42066=CARTESIAN_POINT('Ctrl Pts',(0.154979882582751,-0.0452798744204848,
0.0443029604227849));
#42067=CARTESIAN_POINT('Ctrl Pts',(0.122597586761272,0.105067940844772,
0.0522031722871918));
#42068=CARTESIAN_POINT('Ctrl Pts',(-0.0210134469518542,0.160084070774355,
0.0601033841515984));
#42069=CARTESIAN_POINT('Ctrl Pts',(-0.145559194164939,0.0698672872613988,
0.0680035960160053));
#42070=CARTESIAN_POINT('Ctrl Pts',(-0.138045878489652,-0.0837392716191075,
0.0759038078804119));
#42071=CARTESIAN_POINT('Ctrl Pts',(-0.00528942707681416,-0.16137168859408,
0.083804019744819));
#42072=CARTESIAN_POINT('Ctrl Pts',(0.132265784240875,-0.0925993168709629,
0.0917042316092254));
#42073=CARTESIAN_POINT('Ctrl Pts',(0.149822136811053,0.0601846625535317,
0.0996044434736326));
#42074=CARTESIAN_POINT('Ctrl Pts',(0.0314514425097271,0.15836557740051,
0.107504655338039));
#42075=CARTESIAN_POINT('Ctrl Pts',(-0.115453743482173,0.112868479032945,
0.115404867202446));
#42076=CARTESIAN_POINT('Ctrl Pts',(-0.157612847166081,-0.0350292615003714,
0.123305079066853));
#42077=CARTESIAN_POINT('Ctrl Pts',(-0.0567767606515088,-0.151146472329493,
0.13120529093126));
#42078=CARTESIAN_POINT('Ctrl Pts',(0.0955703749036966,-0.130135167300756,
0.139105502795666));
#42079=CARTESIAN_POINT('Ctrl Pts',(0.161210724837657,0.00894204350597287,
0.147005714660073));
#42080=CARTESIAN_POINT('Ctrl Pts',(0.0805916924126166,0.139906528844762,
0.15490592652448));
#42081=CARTESIAN_POINT('Ctrl Pts',(-0.0731446283672545,0.143939991967805,
0.162806138388887));
#42082=CARTESIAN_POINT('Ctrl Pts',(-0.160520053454664,0.0173830466635891,
0.170706350253294));
#42083=CARTESIAN_POINT('Ctrl Pts',(-0.102262712397196,-0.124944769797408,
0.1786065621177));
#42084=CARTESIAN_POINT('Ctrl Pts',(0.0487730780976374,-0.153915706589351,
0.186506773982107));
#42085=CARTESIAN_POINT('Ctrl Pts',(0.155559205603179,-0.0432457098552795,
0.194406985846514));
#42086=CARTESIAN_POINT('Ctrl Pts',(0.121213325537862,0.106659212347636,
0.202307197710921));
#42087=CARTESIAN_POINT('Ctrl Pts',(-0.0231040596435062,0.159796934574786,
0.210207409575327));
#42088=CARTESIAN_POINT('Ctrl Pts',(-0.146460150332438,0.0679579445972159,
0.218107621439734));
#42089=CARTESIAN_POINT('Ctrl Pts',(-0.136939405068282,-0.0855362917640029,
0.226007833304141));
#42090=CARTESIAN_POINT('Ctrl Pts',(-0.00317957619632727,-0.16142722250312,
0.233908045168548));
#42091=CARTESIAN_POINT('Ctrl Pts',(0.133464941949482,-0.0908623527095838,
0.241808257032955));
#42092=CARTESIAN_POINT('Ctrl Pts',(0.149022603660681,0.0621379229433468,
0.249708468897361));
#42093=CARTESIAN_POINT('Ctrl Pts',(0.0293786285125025,0.158763201203343,
0.257608680761768));
#42094=CARTESIAN_POINT('Ctrl Pts',(-0.11691928077733,0.111349627983502,
0.265508892626175));
#42095=CARTESIAN_POINT('Ctrl Pts',(-0.157141482401145,-0.0370865525269131,
0.273409104490581));
#42096=CARTESIAN_POINT('Ctrl Pts',(-0.0547961465019971,-0.15187573933352,
0.281309316354988));
#42097=CARTESIAN_POINT('Ctrl Pts',(0.0972633167756718,-0.12887476509914,
0.289209528219395));
#42098=CARTESIAN_POINT('Ctrl Pts',(0.161080061758064,0.0110486005260055,
0.297109740083802));
#42099=CARTESIAN_POINT('Ctrl Pts',(0.0787559698462676,0.140948058103473,
0.305009951948209));
#42100=CARTESIAN_POINT('Ctrl Pts',(-0.0750199406092437,0.142971557942657,
0.312910163812615));
#42101=CARTESIAN_POINT('Ctrl Pts',(-0.160733567100311,0.0152832678696448,
0.320810375677022));
#42102=CARTESIAN_POINT('Ctrl Pts',(-0.100620716020809,-0.12627085719605,
0.328710587541429));
#42103=CARTESIAN_POINT('Ctrl Pts',(0.050780873638021,-0.153265001687028,
0.336610799405836));
#42104=CARTESIAN_POINT('Ctrl Pts',(0.156111215926553,-0.0412085686659782,
0.344511011270243));
#42105=CARTESIAN_POINT('Ctrl Pts',(0.119808736032893,0.108234581533658,
0.35241122313465));
#42106=CARTESIAN_POINT('Ctrl Pts',(-0.0251909268639622,0.15948126872238,
0.360311434999056));
#42107=CARTESIAN_POINT('Ctrl Pts',(-0.147335972660104,0.066037633436295,
0.368211646863463));
#42108=CARTESIAN_POINT('Ctrl Pts',(-0.135809587528269,-0.0873190346085379,
0.37611185872787));
#42109=CARTESIAN_POINT('Ctrl Pts',(-0.00106915242017828,-0.16145499305586,
0.384012070592276));
#42110=CARTESIAN_POINT('Ctrl Pts',(0.134641277532382,-0.0891099559758252,
0.391912282456683));
#42111=CARTESIAN_POINT('Ctrl Pts',(0.148197613649053,0.0640806146840961,
0.39981249432109));
#42112=CARTESIAN_POINT('Ctrl Pts',(0.0273007899642087,0.159133669400588,
0.407712706185496));
#42113=CARTESIAN_POINT('Ctrl Pts',(-0.118364836573682,0.109811763178865,
0.415612918049904));
#42114=CARTESIAN_POINT('Ctrl Pts',(-0.156643266416161,-0.0391375134115731,
0.42351312991431));
#42115=CARTESIAN_POINT('Ctrl Pts',(-0.0528061681290295,-0.152579049928534,
0.431413341778717));
#42116=CARTESIAN_POINT('Ctrl Pts',(0.0989396379107883,-0.12759234271557,
0.439313553643124));
#42117=CARTESIAN_POINT('Ctrl Pts',(0.160921873410089,0.0131532706104934,
0.447213765507531));
#42118=CARTESIAN_POINT('Ctrl Pts',(0.0769067893276909,0.14196550153073,
0.455113977371937));
#42119=CARTESIAN_POINT('Ctrl Pts',(-0.0768824333571298,0.14197869315729,
0.463014189236344));
#42120=CARTESIAN_POINT('Ctrl Pts',(-0.160919614537593,0.0131808773091078,
0.470914401100751));
#42121=CARTESIAN_POINT('Ctrl Pts',(-0.098961525511766,-0.127575367285184,
0.478814612965158));
#42122=CARTESIAN_POINT('Ctrl Pts',(0.0527799917097706,-0.152588106825801,
0.486714824829564));
#42123=CARTESIAN_POINT('Ctrl Pts',(0.156636549889514,-0.0391643857129832,
0.494615036693972));
#42124=CARTESIAN_POINT('Ctrl Pts',(0.118383673548094,0.109791455527395,
0.502515248558378));
#42125=CARTESIAN_POINT('Ctrl Pts',(-0.027273489444968,0.15913835063573,
0.510415460422786));
#42126=CARTESIAN_POINT('Ctrl Pts',(-0.14818661814222,0.0641060377276359,
0.518315672287191));
#42127=CARTESIAN_POINT('Ctrl Pts',(-0.13465656277644,-0.0890868563302129,
0.526215884151598));
#42128=CARTESIAN_POINT('Ctrl Pts',(0.00104145405313166,-0.161455174098016,
0.534116096016006));
#42129=CARTESIAN_POINT('Ctrl Pts',(0.135794605545242,-0.0873423320868967,
0.542016307880412));
#42130=CARTESIAN_POINT('Ctrl Pts',(0.147347299553637,0.0660123562965002,
0.549916519744819));
#42131=CARTESIAN_POINT('Ctrl Pts',(0.025218286243035,0.15947694475544,0.557816731609225));
#42132=CARTESIAN_POINT('Ctrl Pts',(-0.119790166126449,0.108255133684104,
0.565716943473633));
#42133=CARTESIAN_POINT('Ctrl Pts',(-0.156118283149977,-0.0411817864579589,
0.573617155338038));
#42134=CARTESIAN_POINT('Ctrl Pts',(-0.0508071662111437,-0.153256287737759,
0.581517367202447));
#42135=CARTESIAN_POINT('Ctrl Pts',(0.10059905219016,-0.126288117287442,
0.589417579066852));
#42136=CARTESIAN_POINT('Ctrl Pts',(0.160736186650373,0.0152556930573902,
0.597317790931261));
#42137=CARTESIAN_POINT('Ctrl Pts',(0.0750444669377644,0.14295868582074,
0.605218002795666));
#42138=CARTESIAN_POINT('Ctrl Pts',(-0.0787317883956269,0.140961566980476,
0.613118214660074));
#42139=CARTESIAN_POINT('Ctrl Pts',(-0.161078163949129,0.0110762343935455,
0.62101842652448));
#42140=CARTESIAN_POINT('Ctrl Pts',(-0.097285424406824,-0.128858077230555,
0.628918638388887));
#42141=CARTESIAN_POINT('Ctrl Pts',(0.0547700907096662,-0.151885137631092,
0.636818850253293));
#42142=CARTESIAN_POINT('Ctrl Pts',(0.157135117718952,-0.037113510329848,
0.644719062117701));
#42143=CARTESIAN_POINT('Ctrl Pts',(0.116938381600928,0.111329568301349,
0.652619273982107));
#42144=CARTESIAN_POINT('Ctrl Pts',(-0.0293513915183856,0.158768238906452,
0.660519485846514));
#42145=CARTESIAN_POINT('Ctrl Pts',(-0.149011941419152,0.0621634875469089,
0.668419697710921));
#42146=CARTESIAN_POINT('Ctrl Pts',(-0.133480527843221,-0.0908394548451002,
0.676319909575327));
#42147=CARTESIAN_POINT('Ctrl Pts',(0.00315188256353199,-0.161427765596558,
0.684220121439734));
#42148=CARTESIAN_POINT('Ctrl Pts',(0.136924728904249,-0.0855597830979986,
0.692120333304141));
#42149=CARTESIAN_POINT('Ctrl Pts',(0.14647180668124,0.0679328176880866,
0.700020545168548));
#42150=CARTESIAN_POINT('Ctrl Pts',(0.0231314731994126,0.159792968600594,
0.707920757032954));
#42151=CARTESIAN_POINT('Ctrl Pts',(-0.121195025857785,0.106680005512326,
0.715820968897362));
#42152=CARTESIAN_POINT('Ctrl Pts',(-0.155566622343907,-0.0432190223689262,
0.723721180761768));
#42153=CARTESIAN_POINT('Ctrl Pts',(-0.0487994822782217,-0.1539073369789,
0.731621392626175));
#42154=CARTESIAN_POINT('Ctrl Pts',(0.102241275937164,-0.124962311786944,
0.739521604490582));
#42155=CARTESIAN_POINT('Ctrl Pts',(0.160523033427699,0.0173555088039932,
0.747421816354988));
#42156=CARTESIAN_POINT('Ctrl Pts',(0.0731693204960455,0.143927440877225,
0.755322028219396));
#42157=CARTESIAN_POINT('Ctrl Pts',(-0.0805676889177445,0.139920353941802,
0.763222240083802));
#42158=CARTESIAN_POINT('Ctrl Pts',(-0.161209189739,0.00896969739313117,
0.771122451948209));
#42159=CARTESIAN_POINT('Ctrl Pts',(-0.0955926962756769,-0.130118765235746,
0.779022663812615));
#42160=CARTESIAN_POINT('Ctrl Pts',(0.0567508251684453,-0.151156219176586,
0.786922875677023));
#42161=CARTESIAN_POINT('Ctrl Pts',(0.157606844475459,-0.0350562835700847,
0.794823087541428));
#42162=CARTESIAN_POINT('Ctrl Pts',(0.115473087684851,0.112848639167101,
0.802723299405837));
#42163=CARTESIAN_POINT('Ctrl Pts',(-0.0314242410165019,0.158371030690115,
0.810623511270242));
#42164=CARTESIAN_POINT('Ctrl Pts',(-0.149811871720937,0.0602102504337274,
0.81852372313465));
#42165=CARTESIAN_POINT('Ctrl Pts',(-0.132281550246616,-0.0925764083493082,
0.826423934999057));
#42166=CARTESIAN_POINT('Ctrl Pts',(0.00526151903952945,-0.161373004547461,
0.834324146863462));
#42167=CARTESIAN_POINT('Ctrl Pts',(0.138031935836139,-0.0837621723962628,
0.842224358727871));
#42168=CARTESIAN_POINT('Ctrl Pts',(0.145570370453223,0.0698408327169628,
0.850124570592276));
#42169=CARTESIAN_POINT('Ctrl Pts',(0.0210424436816558,0.160083278442666,
0.858024782456684));
#42170=CARTESIAN_POINT('Ctrl Pts',(-0.122582473291093,0.105083625150338,
0.86592499432109));
#42171=CARTESIAN_POINT('Ctrl Pts',(-0.154982115072408,-0.0452431320599261,
0.873825206185497));
#42172=CARTESIAN_POINT('Ctrl Pts',(-0.0467953572586411,-0.154542991514022,
0.881725418049904));
#42173=CARTESIAN_POINT('Ctrl Pts',(0.103888647286289,-0.123594427089244,
0.88962562991431));
#42174=CARTESIAN_POINT('Ctrl Pts',(0.160239305296586,0.0194128744409952,
0.897525841778718));
#42175=CARTESIAN_POINT('Ctrl Pts',(0.0713651976137454,0.14494762602415,
0.905426053643123));
#42176=CARTESIAN_POINT('Ctrl Pts',(-0.0825618262402486,0.138702046860037,
0.913326265507531));
#42177=CARTESIAN_POINT('Ctrl Pts',(-0.134777147462009,0.0510524339304846,
0.918593073417135));
#42178=CARTESIAN_POINT('Ctrl Pts',(-0.136701386950153,0.00581475974607277,
0.921226477371938));
#42179=CARTESIAN_POINT('Ctrl Pts',(0.0740036351041154,-0.103579689087084,
-0.00549926131403137));
#42180=CARTESIAN_POINT('Ctrl Pts',(0.108280567705778,-0.0790901618921417,
-0.00286585735922911));
#42181=CARTESIAN_POINT('Ctrl Pts',(0.150052095188851,0.00614632014659505,
0.00240095055037541));
#42182=CARTESIAN_POINT('Ctrl Pts',(0.0766932604427849,0.129279473432083,
0.0103011624147822));
#42183=CARTESIAN_POINT('Ctrl Pts',(-0.0663051564234898,0.134744128527746,
0.018201374279189));
#42184=CARTESIAN_POINT('Ctrl Pts',(-0.149116707504962,0.0181519352949098,
0.0261015861435957));
#42185=CARTESIAN_POINT('Ctrl Pts',(-0.0966576313088641,-0.115007983126889,
0.0340017980080025));
#42186=CARTESIAN_POINT('Ctrl Pts',(0.0435032790655407,-0.143774083669597,
0.0419020098724094));
#42187=CARTESIAN_POINT('Ctrl Pts',(0.144191040034967,-0.04212773991396,
0.0498022217368161));
#42188=CARTESIAN_POINT('Ctrl Pts',(0.114063020608148,0.0977536917196387,
0.0577024336012229));
#42189=CARTESIAN_POINT('Ctrl Pts',(-0.0195506069575822,0.148939902865525,
0.0656026454656297));
#42190=CARTESIAN_POINT('Ctrl Pts',(-0.13542616785819,0.0650035130157202,
0.0735028573300364));
#42191=CARTESIAN_POINT('Ctrl Pts',(-0.12843588767939,-0.0779098065200985,
0.0814030691944432));
#42192=CARTESIAN_POINT('Ctrl Pts',(-0.00492120640875794,-0.150137883851829,
0.0893032810588501));
#42193=CARTESIAN_POINT('Ctrl Pts',(0.123058171634303,-0.0861530644083569,
0.0972034929232567));
#42194=CARTESIAN_POINT('Ctrl Pts',(0.139392348006922,0.0559949391051687,
0.105103704787664));
#42195=CARTESIAN_POINT('Ctrl Pts',(0.0292619669759775,0.147341041498886,
0.11300391665207));
#42196=CARTESIAN_POINT('Ctrl Pts',(-0.107416492200115,0.105011199568016,
0.120904128516477));
#42197=CARTESIAN_POINT('Ctrl Pts',(-0.146640712181561,-0.0325907179901145,
0.128804340380884));
#42198=CARTESIAN_POINT('Ctrl Pts',(-0.0528242764914083,-0.140624490608767,
0.136704552245291));
#42199=CARTESIAN_POINT('Ctrl Pts',(0.0889172938077157,-0.121075876465457,
0.144604764109697));
#42200=CARTESIAN_POINT('Ctrl Pts',(0.149988125502165,0.00831954787729212,
0.152504975974104));
#42201=CARTESIAN_POINT('Ctrl Pts',(0.0749813443751213,0.130167009844241,
0.160405187838511));
#42202=CARTESIAN_POINT('Ctrl Pts',(-0.0680527037540773,0.133919685565514,
0.168305399702918));
#42203=CARTESIAN_POINT('Ctrl Pts',(-0.149345534842162,0.0161729350650448,
0.176205611567325));
#42204=CARTESIAN_POINT('Ctrl Pts',(-0.0951437477665844,-0.116246805738792,
0.184105823431731));
#42205=CARTESIAN_POINT('Ctrl Pts',(0.0453777660648959,-0.143200946090439,
0.192006035296138));
#42206=CARTESIAN_POINT('Ctrl Pts',(0.144730033789766,-0.040235182638969,
0.199906247160545));
#42207=CARTESIAN_POINT('Ctrl Pts',(0.112775123997586,0.0992341876985505,
0.207806459024951));
#42208=CARTESIAN_POINT('Ctrl Pts',(-0.021495682752556,0.148672755500605,
0.215706670889359));
#42209=CARTESIAN_POINT('Ctrl Pts',(-0.136264404438658,0.063227088231138,
0.223606882753765));
#42210=CARTESIAN_POINT('Ctrl Pts',(-0.127406440819969,-0.0795817280581598,
0.231507094618172));
#42211=CARTESIAN_POINT('Ctrl Pts',(-0.00295823168128856,-0.150189551797165,
0.239407306482579));
#42212=CARTESIAN_POINT('Ctrl Pts',(0.124173850613332,-0.0845370180882872,
0.247307518346986));
#42213=CARTESIAN_POINT('Ctrl Pts',(0.138648473933891,0.0578122243061442,
0.255207730211393));
#42214=CARTESIAN_POINT('Ctrl Pts',(0.0273334508287331,0.147710984931011,
0.263107942075799));
#42215=CARTESIAN_POINT('Ctrl Pts',(-0.108780006891681,0.103598082530968,
0.271008153940206));
#42216=CARTESIAN_POINT('Ctrl Pts',(-0.146202161225402,-0.0345047917900689,
0.278908365804612));
#42217=CARTESIAN_POINT('Ctrl Pts',(-0.0509815417482485,-0.141302990076062,
0.28680857766902));
#42218=CARTESIAN_POINT('Ctrl Pts',(0.0904923824267724,-0.119903216496403,
0.294708789533426));
#42219=CARTESIAN_POINT('Ctrl Pts',(0.149866558463742,0.0102794580446603,
0.302609001397833));
#42220=CARTESIAN_POINT('Ctrl Pts',(0.0732734146642041,0.131136033594535,
0.31050921326224));
#42221=CARTESIAN_POINT('Ctrl Pts',(-0.0697974671263062,0.133018668562764,
0.318409425126647));
#42222=CARTESIAN_POINT('Ctrl Pts',(-0.149544184848307,0.0142193312611412,
0.326309636991054));
#42223=CARTESIAN_POINT('Ctrl Pts',(-0.0936160580993886,-0.117480578264625,
0.33420984885546));
#42224=CARTESIAN_POINT('Ctrl Pts',(0.0472457899807798,-0.142595539665694,
0.342110060719868));
#42225=CARTESIAN_POINT('Ctrl Pts',(0.14524361620647,-0.0383398559559941,
0.350010272584273));
#42226=CARTESIAN_POINT('Ctrl Pts',(0.111468314248034,0.100699888391995,
0.357910484448681));
#42227=CARTESIAN_POINT('Ctrl Pts',(-0.02343727381533,0.148379064559539,
0.365810696313087));
#42228=CARTESIAN_POINT('Ctrl Pts',(-0.137079256858259,0.0614404585159162,
0.373710908177495));
#42229=CARTESIAN_POINT('Ctrl Pts',(-0.126355274930375,-0.0812403662025727,
0.381611120041901));
#42230=CARTESIAN_POINT('Ctrl Pts',(-0.000994723939985704,-0.150215389117566,
0.389511331906308));
#42231=CARTESIAN_POINT('Ctrl Pts',(0.125268296216863,-0.0829066135262008,
0.397411543770714));
#42232=CARTESIAN_POINT('Ctrl Pts',(0.137880915165535,0.0596196765889682,
0.405311755635121));
#42233=CARTESIAN_POINT('Ctrl Pts',(0.0254002599118846,0.148055663180668,
0.413211967499528));
#42234=CARTESIAN_POINT('Ctrl Pts',(-0.110124931085911,0.102167275371236,
0.421112179363935));
#42235=CARTESIAN_POINT('Ctrl Pts',(-0.145738628282677,-0.0364129761176204,
0.429012391228342));
#42236=CARTESIAN_POINT('Ctrl Pts',(-0.0491300946670952,-0.141957340076027,
0.436912603092748));
#42237=CARTESIAN_POINT('Ctrl Pts',(0.0920520073527751,-0.118710069268716,
0.444812814957155));
#42238=CARTESIAN_POINT('Ctrl Pts',(0.149719382313936,0.0122376126345037,
0.452713026821562));
#42239=CARTESIAN_POINT('Ctrl Pts',(0.0715529638692849,0.13208264823579,
0.460613238685969));
#42240=CARTESIAN_POINT('Ctrl Pts',(-0.071530303426733,0.132094921534244,
0.468513450550375));
#42241=CARTESIAN_POINT('Ctrl Pts',(-0.149717280691655,0.0122632975073946,
0.476413662414783));
#42242=CARTESIAN_POINT('Ctrl Pts',(-0.0920723712599867,-0.118694275573937,
0.484313874279189));
#42243=CARTESIAN_POINT('Ctrl Pts',(0.0491057405054188,-0.141965766482181,
0.492214086143596));
#42244=CARTESIAN_POINT('Ctrl Pts',(0.14573237932348,-0.03643797771798,0.500114298008002));
#42245=CARTESIAN_POINT('Ctrl Pts',(0.110142456734312,0.102148381426183,
0.50801450987241));
#42246=CARTESIAN_POINT('Ctrl Pts',(-0.0253748599038521,0.148060018534101,
0.515914721736816));
#42247=CARTESIAN_POINT('Ctrl Pts',(-0.137870685105096,0.0596433298207777,
0.523814933601224));
#42248=CARTESIAN_POINT('Ctrl Pts',(-0.125282517386741,-0.0828851219502007,
0.531715145465628));
#42249=CARTESIAN_POINT('Ctrl Pts',(0.00096895378011186,-0.150215557556568,
0.539615357330038));
#42250=CARTESIAN_POINT('Ctrl Pts',(0.126341335910172,-0.0812620418392971,
0.547515569194442));
#42251=CARTESIAN_POINT('Ctrl Pts',(0.137089795236089,0.0614169410308395,
0.55541578105885));
#42252=CARTESIAN_POINT('Ctrl Pts',(0.0234627285856986,0.148375041603271,
0.563315992923257));
#42253=CARTESIAN_POINT('Ctrl Pts',(-0.111451037075805,0.100719009815358,
0.571216204787664));
#42254=CARTESIAN_POINT('Ctrl Pts',(-0.145250191448873,-0.0383149381772212,
0.57911641665207));
#42255=CARTESIAN_POINT('Ctrl Pts',(-0.0472702522103304,-0.142587432333395,
0.587016628516477));
#42256=CARTESIAN_POINT('Ctrl Pts',(0.0935959023848529,-0.117496636803883,
0.594916840380884));
#42257=CARTESIAN_POINT('Ctrl Pts',(0.149546622039777,0.0141936760548576,
0.60281705224529));
#42258=CARTESIAN_POINT('Ctrl Pts',(0.0698202860674386,0.133006692526806,
0.610717264109698));
#42259=CARTESIAN_POINT('Ctrl Pts',(-0.0732509165924606,0.13114860205821,
0.618617475974104));
#42260=CARTESIAN_POINT('Ctrl Pts',(-0.149864792769772,0.0103051681951267,
0.626517687838512));
#42261=CARTESIAN_POINT('Ctrl Pts',(-0.0905129510468744,-0.119887690344964,
0.634417899702917));
#42262=CARTESIAN_POINT('Ctrl Pts',(0.0509572998161204,-0.141311734116118,
0.642318111567325));
#42263=CARTESIAN_POINT('Ctrl Pts',(0.146196239617194,-0.0345298729398102,
0.650218323431731));
#42264=CARTESIAN_POINT('Ctrl Pts',(0.108797778021546,0.103579419292979,
0.658118535296138));
#42265=CARTESIAN_POINT('Ctrl Pts',(-0.0273081099235566,0.147715671937082,
0.666018747160545));
#42266=CARTESIAN_POINT('Ctrl Pts',(-0.138638553938667,0.0578360092433499,
0.673918959024952));
#42267=CARTESIAN_POINT('Ctrl Pts',(-0.124188351503322,-0.0845157142465292,
0.681819170889359));
#42268=CARTESIAN_POINT('Ctrl Pts',(0.00293246592609361,-0.150190057083441,
0.689719382753765));
#42269=CARTESIAN_POINT('Ctrl Pts',(0.127392786329333,-0.0796035840553634,
0.697619594618173));
#42270=CARTESIAN_POINT('Ctrl Pts',(0.136275249336903,0.0632037105184985,
0.705519806482578));
#42271=CARTESIAN_POINT('Ctrl Pts',(0.0215211879282666,0.148669065615609,
0.713420018346986));
#42272=CARTESIAN_POINT('Ctrl Pts',(-0.11275809824006,0.0992535333580773,
0.721320230211393));
#42273=CARTESIAN_POINT('Ctrl Pts',(-0.144736934218011,-0.0402103529878636,
0.729220442075799));
#42274=CARTESIAN_POINT('Ctrl Pts',(-0.0454023321324136,-0.143193159125993,
0.737120653940206));
#42275=CARTESIAN_POINT('Ctrl Pts',(0.0951238035943801,-0.116263126552003,
0.745020865804613));
#42276=CARTESIAN_POINT('Ctrl Pts',(0.149348307365949,0.0161473142389802,
0.75292107766902));
#42277=CARTESIAN_POINT('Ctrl Pts',(0.0680756769533821,0.133908008212467,
0.760821289533426));
#42278=CARTESIAN_POINT('Ctrl Pts',(-0.0749590118708499,0.130179872514462,
0.768721501397833));
#42279=CARTESIAN_POINT('Ctrl Pts',(-0.149986697268588,0.00834527665372157,
0.77662171326224));
#42280=CARTESIAN_POINT('Ctrl Pts',(-0.0889380612891912,-0.121060616221528,
0.784521925126647));
#42281=CARTESIAN_POINT('Ctrl Pts',(0.0528001464932815,-0.140633558934255,
0.792422136991054));
#42282=CARTESIAN_POINT('Ctrl Pts',(0.146635127365071,-0.0326158589327362,
0.80032234885546));
#42283=CARTESIAN_POINT('Ctrl Pts',(0.107434489766355,0.104992740843939,
0.808222560719866));
#42284=CARTESIAN_POINT('Ctrl Pts',(-0.0292366591003167,0.147346115160618,
0.816122772584275));
#42285=CARTESIAN_POINT('Ctrl Pts',(-0.139382797515625,0.0560187456986177,
0.82402298444868));
#42286=CARTESIAN_POINT('Ctrl Pts',(-0.123072840097892,-0.0861317506513214,
0.831923196313088));
#42287=CARTESIAN_POINT('Ctrl Pts',(0.00489524117472862,-0.150139108195811,
0.839823408177494));
#42288=CARTESIAN_POINT('Ctrl Pts',(0.128422915636328,-0.0779311130717641,
0.847723620041902));
#42289=CARTESIAN_POINT('Ctrl Pts',(0.135436566115076,0.0649789000904037,
0.855623831906308));
#42290=CARTESIAN_POINT('Ctrl Pts',(0.0195775850953746,0.148939165691587,
0.863524043770715));
#42291=CARTESIAN_POINT('Ctrl Pts',(-0.114048959254202,0.0977682841705676,
0.871424255635121));
#42292=CARTESIAN_POINT('Ctrl Pts',(-0.144193117111036,-0.0420935553533985,
0.879324467499528));
#42293=CARTESIAN_POINT('Ctrl Pts',(-0.0435377232159684,-0.143784562906888,
0.887224679363934));
#42294=CARTESIAN_POINT('Ctrl Pts',(0.09665649405843,-0.114990466423977,
0.895124891228342));
#42295=CARTESIAN_POINT('Ctrl Pts',(0.149084330818603,0.0180614574554272,
0.903025103092748));
#42296=CARTESIAN_POINT('Ctrl Pts',(0.0663971471312236,0.134857173710026,
0.910925314957155));
#42297=CARTESIAN_POINT('Ctrl Pts',(-0.0768143283784672,0.129046377235758,
0.918825526821562));
#42298=CARTESIAN_POINT('Ctrl Pts',(-0.125394707633209,0.0474984457471263,
0.924092334731166));
#42299=CARTESIAN_POINT('Ctrl Pts',(-0.127184992207232,0.00540996832212636,
0.926725738685969));
#42300=CARTESIAN_POINT('Ctrl Pts',(0.0684664424539458,-0.0958295198918399,
-1.80411241501588E-16));
#42301=CARTESIAN_POINT('Ctrl Pts',(0.100178663484274,-0.0731723787654901,
0.00263340395480208));
#42302=CARTESIAN_POINT('Ctrl Pts',(0.138824709433362,0.00568643248440989,
0.00790021186440659));
#42303=CARTESIAN_POINT('Ctrl Pts',(0.0709548212776815,0.119606362792331,
0.0158004237288134));
#42304=CARTESIAN_POINT('Ctrl Pts',(-0.0613439889848912,0.1246621346218,
0.0237006355932201));
#42305=CARTESIAN_POINT('Ctrl Pts',(-0.137959310498012,0.016793748463141,
0.0316008474576269));
#42306=CARTESIAN_POINT('Ctrl Pts',(-0.0894253929882274,-0.106402711804945,
0.0395010593220337));
#42307=CARTESIAN_POINT('Ctrl Pts',(0.040248222246223,-0.133016439153077,
0.0474012711864405));
#42308=CARTESIAN_POINT('Ctrl Pts',(0.133402197487182,-0.0389756054074351,
0.0553014830508473));
#42309=CARTESIAN_POINT('Ctrl Pts',(0.105528454455023,0.0904394425945055,
0.0632016949152541));
#42310=CARTESIAN_POINT('Ctrl Pts',(-0.0180877669633101,0.137795734956694,
0.0711019067796609));
#42311=CARTESIAN_POINT('Ctrl Pts',(-0.125293141551441,0.0601397387700418,
0.0790021186440675));
#42312=CARTESIAN_POINT('Ctrl Pts',(-0.118825896869129,-0.0720803414210898,
0.0869023305084746));
#42313=CARTESIAN_POINT('Ctrl Pts',(-0.0045529857407016,-0.138904079109577,
0.0948025423728811));
#42314=CARTESIAN_POINT('Ctrl Pts',(0.113850559027731,-0.0797068119457511,
0.102702754237288));
#42315=CARTESIAN_POINT('Ctrl Pts',(0.12896255920279,0.0518052156568057,
0.110602966101695));
#42316=CARTESIAN_POINT('Ctrl Pts',(0.0270724914422277,0.136316505597261,
0.118503177966102));
#42317=CARTESIAN_POINT('Ctrl Pts',(-0.0993792409180562,0.0971539201030866,
0.126403389830508));
#42318=CARTESIAN_POINT('Ctrl Pts',(-0.135668577197041,-0.0301521744798576,
0.134303601694915));
#42319=CARTESIAN_POINT('Ctrl Pts',(-0.0488717923313075,-0.130102508888041,
0.142203813559322));
#42320=CARTESIAN_POINT('Ctrl Pts',(0.0822642127117346,-0.112016585630158,
0.150104025423729));
#42321=CARTESIAN_POINT('Ctrl Pts',(0.138765526166673,0.00769705224861128,
0.158004237288135));
#42322=CARTESIAN_POINT('Ctrl Pts',(0.0693709963376258,0.12042749084372,
0.165904449152542));
#42323=CARTESIAN_POINT('Ctrl Pts',(-0.0629607791409001,0.123899379163224,
0.173804661016949));
#42324=CARTESIAN_POINT('Ctrl Pts',(-0.138171016229659,0.0149628234665004,
0.181704872881356));
#42325=CARTESIAN_POINT('Ctrl Pts',(-0.088024783135973,-0.107548841680175,
0.189605084745762));
#42326=CARTESIAN_POINT('Ctrl Pts',(0.0419824540321544,-0.132486185591528,
0.197505296610169));
#42327=CARTESIAN_POINT('Ctrl Pts',(0.133900861976353,-0.0372246554226585,
0.205405508474576));
#42328=CARTESIAN_POINT('Ctrl Pts',(0.10433692245731,0.0918091630494651,
0.213305720338983));
#42329=CARTESIAN_POINT('Ctrl Pts',(-0.0198873058616059,0.137548576426424,
0.221205932203389));
#42330=CARTESIAN_POINT('Ctrl Pts',(-0.126068658544878,0.0584962318650602,
0.229106144067797));
#42331=CARTESIAN_POINT('Ctrl Pts',(-0.117873476571655,-0.0736271643523165,
0.237006355932203));
#42332=CARTESIAN_POINT('Ctrl Pts',(-0.00273688716624997,-0.138951881091211,
0.24490656779661));
#42333=CARTESIAN_POINT('Ctrl Pts',(0.114882759277182,-0.0782116834669906,
0.252806779661017));
#42334=CARTESIAN_POINT('Ctrl Pts',(0.128274344207101,0.0534865256689417,
0.260706991525423));
#42335=CARTESIAN_POINT('Ctrl Pts',(0.0252882731449639,0.136658768658679,
0.26860720338983));
#42336=CARTESIAN_POINT('Ctrl Pts',(-0.100640733006032,0.0958465370784341,
0.276507415254237));
#42337=CARTESIAN_POINT('Ctrl Pts',(-0.13526284004966,-0.0319230310532247,
0.284407627118644));
#42338=CARTESIAN_POINT('Ctrl Pts',(-0.0471669369944997,-0.130730240818604,
0.292307838983051));
#42339=CARTESIAN_POINT('Ctrl Pts',(0.0837214480778729,-0.110931667893667,
0.300208050847457));
#42340=CARTESIAN_POINT('Ctrl Pts',(0.138653055169421,0.00951031556331505,
0.308108262711865));
#42341=CARTESIAN_POINT('Ctrl Pts',(0.0677908594821406,0.121324009085596,
0.316008474576271));
#42342=CARTESIAN_POINT('Ctrl Pts',(-0.0645749936433688,0.123065779182871,
0.323908686440678));
#42343=CARTESIAN_POINT('Ctrl Pts',(-0.138354802596303,0.0131553946526375,
0.331808898305084));
#42344=CARTESIAN_POINT('Ctrl Pts',(-0.0866114001779684,-0.108690299333199,
0.339709110169492));
#42345=CARTESIAN_POINT('Ctrl Pts',(0.0437107063235388,-0.131926077644361,
0.347609322033898));
#42346=CARTESIAN_POINT('Ctrl Pts',(0.134376016486386,-0.0354711432460098,
0.355509533898305));
#42347=CARTESIAN_POINT('Ctrl Pts',(0.103127892463174,0.0931651952503325,
0.363409745762711));
#42348=CARTESIAN_POINT('Ctrl Pts',(-0.0216836207666979,0.137276860396698,
0.371309957627119));
#42349=CARTESIAN_POINT('Ctrl Pts',(-0.126822541056414,0.0568432835955372,
0.379210169491525));
#42350=CARTESIAN_POINT('Ctrl Pts',(-0.116900962332481,-0.0751616977966073,
0.387110381355933));
#42351=CARTESIAN_POINT('Ctrl Pts',(-0.000920295459793275,-0.138975785179272,
0.395010593220339));
#42352=CARTESIAN_POINT('Ctrl Pts',(0.115895314901344,-0.0767032710765764,
0.402910805084745));
#42353=CARTESIAN_POINT('Ctrl Pts',(0.127564216682018,0.0551587384938402,
0.410811016949152));
#42354=CARTESIAN_POINT('Ctrl Pts',(0.0234997298595607,0.136977656960748,
0.418711228813559));
#42355=CARTESIAN_POINT('Ctrl Pts',(-0.10188502559814,0.0945227875636074,
0.426611440677966));
#42356=CARTESIAN_POINT('Ctrl Pts',(-0.134833990149192,-0.0336884388236675,
0.434511652542373));
#42357=CARTESIAN_POINT('Ctrl Pts',(-0.045454021205161,-0.13133563022352,
0.44241186440678));
#42358=CARTESIAN_POINT('Ctrl Pts',(0.085164376794762,-0.109827795821861,
0.450312076271186));
#42359=CARTESIAN_POINT('Ctrl Pts',(0.138516891217783,0.0113219546585138,
0.458212288135593));
#42360=CARTESIAN_POINT('Ctrl Pts',(0.0661991384108791,0.12219979494085,
0.4661125));
#42361=CARTESIAN_POINT('Ctrl Pts',(-0.0661781734963363,0.122211149911198,
0.474012711864406));
#42362=CARTESIAN_POINT('Ctrl Pts',(-0.138514946845716,0.0113457177056816,
0.481912923728814));
#42363=CARTESIAN_POINT('Ctrl Pts',(-0.0851832170082076,-0.109813183862691,
0.48981313559322));
#42364=CARTESIAN_POINT('Ctrl Pts',(0.0454314893010671,-0.131343426138561,
0.497713347457628));
#42365=CARTESIAN_POINT('Ctrl Pts',(0.134828208757446,-0.0337115697229769,
0.505613559322033));
#42366=CARTESIAN_POINT('Ctrl Pts',(0.10190123992053,0.0945053073249706,
0.513513771186441));
#42367=CARTESIAN_POINT('Ctrl Pts',(-0.0234762303627364,0.136981686432473,
0.521413983050847));
#42368=CARTESIAN_POINT('Ctrl Pts',(-0.127554752067971,0.0551806219139196,
0.529314194915254));
#42369=CARTESIAN_POINT('Ctrl Pts',(-0.115908471997041,-0.0766833875701887,
0.537214406779661));
#42370=CARTESIAN_POINT('Ctrl Pts',(0.000896453507092177,-0.13897594101512,
0.545114618644068));
#42371=CARTESIAN_POINT('Ctrl Pts',(0.116888066275103,-0.0751817515916976,
0.553014830508475));
#42372=CARTESIAN_POINT('Ctrl Pts',(0.126832290918542,0.0568215257651788,
0.560915042372882));
#42373=CARTESIAN_POINT('Ctrl Pts',(0.0217071709283622,0.137273138451102,
0.568815254237287));
#42374=CARTESIAN_POINT('Ctrl Pts',(-0.103111908025161,0.0931828859466119,
0.576715466101696));
#42375=CARTESIAN_POINT('Ctrl Pts',(-0.134382099747769,-0.0354480898964837,
0.584615677966101));
#42376=CARTESIAN_POINT('Ctrl Pts',(-0.0437333382095171,-0.131918576929031,
0.592515889830509));
#42377=CARTESIAN_POINT('Ctrl Pts',(0.0865927525795457,-0.108705156320324,
0.600416101694915));
#42378=CARTESIAN_POINT('Ctrl Pts',(0.138357057429181,0.0131316590523252,
0.608316313559322));
#42379=CARTESIAN_POINT('Ctrl Pts',(0.0645961051971127,0.123054699232873,
0.616216525423729));
#42380=CARTESIAN_POINT('Ctrl Pts',(-0.0677700447892944,0.121335637135943,
0.624116737288135));
#42381=CARTESIAN_POINT('Ctrl Pts',(-0.138651421590416,0.00953410199670787,
0.632016949152542));
#42382=CARTESIAN_POINT('Ctrl Pts',(-0.0837404776869246,-0.110917303459374,
0.639917161016949));
#42383=CARTESIAN_POINT('Ctrl Pts',(0.0471445089225743,-0.130738330601145,
0.647817372881356));
#42384=CARTESIAN_POINT('Ctrl Pts',(0.135257361515437,-0.0319462355497722,
0.655717584745763));
#42385=CARTESIAN_POINT('Ctrl Pts',(0.100657174442164,0.0958292702846084,
0.66361779661017));
#42386=CARTESIAN_POINT('Ctrl Pts',(-0.0252648283287276,0.136663104967713,
0.671518008474576));
#42387=CARTESIAN_POINT('Ctrl Pts',(-0.128265166458182,0.0535085309397911,
0.679418220338983));
#42388=CARTESIAN_POINT('Ctrl Pts',(-0.114896175163422,-0.0781919736479584,
0.68731843220339));
#42389=CARTESIAN_POINT('Ctrl Pts',(0.00271304928865532,-0.138952348570324,
0.695218644067796));
#42390=CARTESIAN_POINT('Ctrl Pts',(0.117860843754417,-0.0736473850127282,
0.703118855932203));
#42391=CARTESIAN_POINT('Ctrl Pts',(0.126078691992566,0.0584746033489104,
0.711019067796611));
#42392=CARTESIAN_POINT('Ctrl Pts',(0.0199109026571207,0.137545162630623,
0.718919279661016));
#42393=CARTESIAN_POINT('Ctrl Pts',(-0.104321170622334,0.0918270612038291,
0.726819491525424));
#42394=CARTESIAN_POINT('Ctrl Pts',(-0.133907246092115,-0.0372016836068011,
0.73471970338983));
#42395=CARTESIAN_POINT('Ctrl Pts',(-0.0420051819866054,-0.132478981273086,
0.742619915254238));
#42396=CARTESIAN_POINT('Ctrl Pts',(0.0880063312515965,-0.107563941317063,
0.750520127118644));
#42397=CARTESIAN_POINT('Ctrl Pts',(0.1381735813042,0.0149391196739674,0.758420338983051));
#42398=CARTESIAN_POINT('Ctrl Pts',(0.0629820334107182,0.123888575547709,
0.766320550847457));
#42399=CARTESIAN_POINT('Ctrl Pts',(-0.069350334823955,0.120439391087123,
0.774220762711865));
#42400=CARTESIAN_POINT('Ctrl Pts',(-0.138764204798178,0.00772085591431189,
0.78212097457627));
#42401=CARTESIAN_POINT('Ctrl Pts',(-0.0822834263027052,-0.112002467207309,
0.790021186440679));
#42402=CARTESIAN_POINT('Ctrl Pts',(0.0488494678181175,-0.130110898691923,
0.797921398305084));
#42403=CARTESIAN_POINT('Ctrl Pts',(0.135663410254684,-0.0301754342953877,
0.805821610169492));
#42404=CARTESIAN_POINT('Ctrl Pts',(0.0993958918478579,0.0971368425207782,
0.813721822033898));
#42405=CARTESIAN_POINT('Ctrl Pts',(-0.0270490771841315,0.136321199631122,
0.821622033898304));
#42406=CARTESIAN_POINT('Ctrl Pts',(-0.128953723310312,0.0518272409635079,
0.829522245762713));
#42407=CARTESIAN_POINT('Ctrl Pts',(-0.113864129949169,-0.0796870929533346,
0.837422457627119));
#42408=CARTESIAN_POINT('Ctrl Pts',(0.00452896330992775,-0.13890521184416,
0.845322669491525));
#42409=CARTESIAN_POINT('Ctrl Pts',(0.118813895436517,-0.0721000537472655,
0.853222881355933));
#42410=CARTESIAN_POINT('Ctrl Pts',(0.125302761776928,0.0601169674638447,
0.861123093220339));
#42411=CARTESIAN_POINT('Ctrl Pts',(0.0181127265090936,0.137795052940508,
0.869023305084746));
#42412=CARTESIAN_POINT('Ctrl Pts',(-0.105515445217312,0.0904529431907972,
0.876923516949153));
#42413=CARTESIAN_POINT('Ctrl Pts',(-0.133404119149664,-0.0389439786468707,
0.88482372881356));
#42414=CARTESIAN_POINT('Ctrl Pts',(-0.0402800891732956,-0.133026134299755,
0.892723940677965));
#42415=CARTESIAN_POINT('Ctrl Pts',(0.0894243408305711,-0.10638650575871,
0.900624152542373));
#42416=CARTESIAN_POINT('Ctrl Pts',(0.137929356340621,0.0167100404698593,
0.908524364406779));
#42417=CARTESIAN_POINT('Ctrl Pts',(0.0614290966487016,0.124766721395902,
0.916424576271187));
#42418=CARTESIAN_POINT('Ctrl Pts',(-0.0710668305166857,0.11939070761148,
0.924324788135593));
#42419=CARTESIAN_POINT('Ctrl Pts',(-0.116012267804409,0.0439444575637681,
0.929591596045198));
#42420=CARTESIAN_POINT('Ctrl Pts',(-0.11766859746431,0.00500517689817995,
0.932225));
#42421=CARTESIAN_POINT('',(0.0684664424539459,-0.0958295198918398,0.));
#42422=CARTESIAN_POINT('Ctrl Pts',(0.0684664424539458,-0.0958295198918399,
-1.80411241501588E-16));
#42423=CARTESIAN_POINT('Ctrl Pts',(0.100178663484274,-0.0731723787654901,
0.00263340395480208));
#42424=CARTESIAN_POINT('Ctrl Pts',(0.138824709433362,0.00568643248440989,
0.00790021186440659));
#42425=CARTESIAN_POINT('Ctrl Pts',(0.0709548212776815,0.119606362792331,
0.0158004237288134));
#42426=CARTESIAN_POINT('Ctrl Pts',(-0.0613439889848912,0.1246621346218,
0.0237006355932201));
#42427=CARTESIAN_POINT('Ctrl Pts',(-0.115532083261749,0.0483695320037083,
0.0292882571924104));
#42428=CARTESIAN_POINT('Ctrl Pts',(-0.117931878255507,0.00481801833454289,
0.0322424748367984));
#42429=CARTESIAN_POINT('Ctrl Pts',(-0.117896184020664,8.43438525024954E-5,
0.0325632885263842));
#42430=CARTESIAN_POINT('Ctrl Pts',(0.0635538308725813,0.132076982143461,
2.60208521396521E-18));
#42431=CARTESIAN_POINT('Ctrl Pts',(0.0672186180130936,0.129896798349724,
2.66126088244575E-18));
#42432=CARTESIAN_POINT('Ctrl Pts',(0.0707747244255609,0.12755097155874,
-6.59520968701772E-18));
#42433=CARTESIAN_POINT('Ctrl Pts',(0.0742090918971922,0.125038932664582,
-4.55364912443912E-18));
#42434=CARTESIAN_POINT('Ctrl Pts',(0.080224006754745,0.120639374320277,
-2.50552574932592E-18));
#42435=CARTESIAN_POINT('Ctrl Pts',(0.0858662145577153,0.115730301363634,
1.59702880631994E-17));
#42436=CARTESIAN_POINT('Ctrl Pts',(0.0911015321007297,0.110378142457541,
2.25514051876985E-17));
#42437=CARTESIAN_POINT('Ctrl Pts',(0.0937720491785869,0.107648025011046,
2.59084099019214E-17));
#42438=CARTESIAN_POINT('Ctrl Pts',(0.0963357255281008,0.104802798728268,
-1.64960383635052E-18));
#42439=CARTESIAN_POINT('Ctrl Pts',(0.0987794574485338,0.101861414187154,
-4.33680868994202E-19));
#42440=CARTESIAN_POINT('Ctrl Pts',(0.10293496714428,0.0968596577026072,
1.63396805676607E-18));
#42441=CARTESIAN_POINT('Ctrl Pts',(0.106751261320725,0.0915729561578743,
3.03784192455847E-17));
#42442=CARTESIAN_POINT('Ctrl Pts',(0.110204305377691,0.08604549563647,2.73218947466347E-17));
#42443=CARTESIAN_POINT('Ctrl Pts',(0.111935557805272,0.0832741931890737,
2.57894452987073E-17));
#42444=CARTESIAN_POINT('Ctrl Pts',(0.113575375365209,0.0804423219653594,
5.7323915193469E-18));
#42445=CARTESIAN_POINT('Ctrl Pts',(0.115119932079619,0.077555293108205,
9.54097911787244E-18));
#42446=CARTESIAN_POINT('Ctrl Pts',(0.116773389847001,0.0744647103902093,
1.36180963184181E-17));
#42447=CARTESIAN_POINT('Ctrl Pts',(0.118313357645953,0.0713188633723711,
-9.33067413676427E-18));
#42448=CARTESIAN_POINT('Ctrl Pts',(0.119735247150481,0.0681278580844796,
-4.33680868994202E-18));
#42449=CARTESIAN_POINT('Ctrl Pts',(0.123742606948277,0.059134538797346,
9.73757301374157E-18));
#42450=CARTESIAN_POINT('Ctrl Pts',(0.126819919828835,0.0497749725291024,
2.44496492997929E-17));
#42451=CARTESIAN_POINT('Ctrl Pts',(0.128866909768778,0.040203097865136,
1.21430643318376E-17));
#42452=CARTESIAN_POINT('Ctrl Pts',(0.129678753995803,0.0364068548860612,
7.26222453596554E-18));
#42453=CARTESIAN_POINT('Ctrl Pts',(0.130327963181773,0.0325772120613575,
7.16378425601151E-18));
#42454=CARTESIAN_POINT('Ctrl Pts',(0.130805907644987,0.0287241348669356,
3.46944695195361E-18));
#42455=CARTESIAN_POINT('Ctrl Pts',(0.131145551201884,0.0259860074399329,
8.44125478642762E-19));
#42456=CARTESIAN_POINT('Ctrl Pts',(0.131398222957245,0.023238193513084,
1.89851870451249E-17));
#42457=CARTESIAN_POINT('Ctrl Pts',(0.131560851492827,0.0204930145081475,
1.56125112837913E-17));
#42458=CARTESIAN_POINT('Ctrl Pts',(0.131856680066531,0.0154994112226654,
9.47746335708933E-18));
#42459=CARTESIAN_POINT('Ctrl Pts',(0.131855937211452,0.0105061465300757,
1.21882171850414E-17));
#42460=CARTESIAN_POINT('Ctrl Pts',(0.131544012134307,0.00553446959878105,
1.73472347597681E-17));
#42461=CARTESIAN_POINT('Ctrl Pts',(0.131183605376493,-0.00020994178392047,
2.50428281171472E-17));
#42462=CARTESIAN_POINT('Ctrl Pts',(0.130407809774817,-0.00592569963173127,
6.69723701682335E-18));
#42463=CARTESIAN_POINT('Ctrl Pts',(0.129236296320737,-0.0115776207498215,
6.93889390390723E-18));
#42464=CARTESIAN_POINT('Ctrl Pts',(0.128494418700647,-0.0151567804883794,
7.09192657770507E-18));
#42465=CARTESIAN_POINT('Ctrl Pts',(0.127593716302061,-0.0187102876496501,
1.81123981287573E-17));
#42466=CARTESIAN_POINT('Ctrl Pts',(0.126538054496122,-0.0222283432593045,
1.73472347597681E-17));
#42467=CARTESIAN_POINT('Ctrl Pts',(0.125628643409289,-0.0252590096692432,
1.66880766401104E-17));
#42468=CARTESIAN_POINT('Ctrl Pts',(0.124606340862147,-0.0282558643089978,
1.76789329645073E-17));
#42469=CARTESIAN_POINT('Ctrl Pts',(0.123476980164864,-0.0312080791264482,
1.38777878078145E-17));
#42470=CARTESIAN_POINT('Ctrl Pts',(0.120897724271906,-0.0379504046593839,
5.19665867965098E-18));
#42471=CARTESIAN_POINT('Ctrl Pts',(0.117758352703866,-0.0444696874516502,
3.23003755723985E-17));
#42472=CARTESIAN_POINT('Ctrl Pts',(0.114097802370374,-0.050694248232474,
2.94902990916057E-17));
#42473=CARTESIAN_POINT('Ctrl Pts',(0.11100985408088,-0.0559451313142133,
2.71197891759751E-17));
#42474=CARTESIAN_POINT('Ctrl Pts',(0.107550620981395,-0.0609862743257036,
5.91633367061488E-18));
#42475=CARTESIAN_POINT('Ctrl Pts',(0.103737131336817,-0.0657661572550731,
2.08166817117217E-17));
#42476=CARTESIAN_POINT('Ctrl Pts',(0.10192691642303,-0.0680351067400168,
2.78896869532561E-17));
#42477=CARTESIAN_POINT('Ctrl Pts',(0.10004287794431,-0.0702374362624183,
3.79094719020518E-18));
#42478=CARTESIAN_POINT('Ctrl Pts',(0.098088083467589,-0.0723681596371707,
3.46944695195361E-18));
#42479=CARTESIAN_POINT('Ctrl Pts',(0.092197190805992,-0.078789224788366,
2.50058632912494E-18));
#42480=CARTESIAN_POINT('Ctrl Pts',(0.0856641330198359,-0.0845647204793276,
-6.81778632605364E-18));
#42481=CARTESIAN_POINT('Ctrl Pts',(0.0785460746715851,-0.0895442682019542,
-6.93889390390723E-18));
#42482=CARTESIAN_POINT('Ctrl Pts',(0.0753062120776356,-0.0918107641495869,
-6.9940173507989E-18));
#42483=CARTESIAN_POINT('Ctrl Pts',(0.0719448689431282,-0.0939117521002605,
3.85531108019535E-18));
#42484=CARTESIAN_POINT('Ctrl Pts',(0.068466442453948,-0.0958295198918383,
3.46944695195361E-18));
#42485=CARTESIAN_POINT('Ctrl Pts',(-0.00156268643912563,0.146080787864432,
0.903650000000001));
#42486=CARTESIAN_POINT('Ctrl Pts',(0.0213629386064158,0.146372019480346,
0.902408930776365));
#42487=CARTESIAN_POINT('Ctrl Pts',(0.0443374951530579,0.14156774719521,
0.901167861552729));
#42488=CARTESIAN_POINT('Ctrl Pts',(0.0647363246762687,0.131545720210662,
0.899926792329093));
#42489=CARTESIAN_POINT('Ctrl Pts',(0.108020258655701,0.110280149367703,
0.897293388374291));
#42490=CARTESIAN_POINT('Ctrl Pts',(0.139707269215135,0.0655222203971333,
0.894659984419488));
#42491=CARTESIAN_POINT('Ctrl Pts',(0.145505194618115,0.0176494760483365,
0.892026580464686));
#42492=CARTESIAN_POINT('Ctrl Pts',(0.151303120021096,-0.0302232683004618,
0.889393176509884));
#42493=CARTESIAN_POINT('Ctrl Pts',(0.131211960267621,-0.0812108280274876,
0.886759772555081));
#42494=CARTESIAN_POINT('Ctrl Pts',(0.0943040817549728,-0.112221779952107,
0.884126368600279));
#42495=CARTESIAN_POINT('Ctrl Pts',(0.0573962032423251,-0.143232731876727,
0.881492964645477));
#42496=CARTESIAN_POINT('Ctrl Pts',(0.0036716059705044,-0.15426707599894,
0.878859560690674));
#42497=CARTESIAN_POINT('Ctrl Pts',(-0.0424770462874833,-0.140299462834264,
0.876226156735872));
#42498=CARTESIAN_POINT('Ctrl Pts',(-0.0886256985454704,-0.126331849669587,
0.87359275278107));
#42499=CARTESIAN_POINT('Ctrl Pts',(-0.127198405789625,-0.0873622792180203,
0.870959348826268));
#42500=CARTESIAN_POINT('Ctrl Pts',(-0.140708905127403,-0.0410788815094769,
0.868325944871466));
#42501=CARTESIAN_POINT('Ctrl Pts',(-0.144574583355673,-0.027836090226996,
0.867572464775741));
#42502=CARTESIAN_POINT('Ctrl Pts',(-0.146388495105525,-0.0139945382267495,
0.866818984680017));
#42503=CARTESIAN_POINT('Ctrl Pts',(-0.146273246343463,-0.000123611542196964,
0.866065504584292));
#42504=CARTESIAN_POINT('Origin',(0.,0.,-0.0924367114736152));
#42505=CARTESIAN_POINT('',(-0.0684664424539439,-0.0958295198918412,0.));
#42506=CARTESIAN_POINT('Ctrl Pts',(-0.0686121729278148,-0.0959472995825297,
4.17959937493162E-17));
#42507=CARTESIAN_POINT('Ctrl Pts',(-0.0396139635805184,-0.116414379406814,
0.00240676188548629));
#42508=CARTESIAN_POINT('Ctrl Pts',(0.042075530384929,-0.130578648252184,
0.00744886483747836));
#42509=CARTESIAN_POINT('Ctrl Pts',(0.133186295059001,-0.0398205273591854,
0.0151263088559762));
#42510=CARTESIAN_POINT('Ctrl Pts',(0.106043485420733,0.0899039768168324,
0.0230323320554937));
#42511=CARTESIAN_POINT('Ctrl Pts',(-0.0174538572390982,0.137906280269365,
0.0309383552550111));
#42512=CARTESIAN_POINT('Ctrl Pts',(-0.105510720744521,0.0746991700253994,
0.0374064817277185));
#42513=CARTESIAN_POINT('Ctrl Pts',(-0.11763008980369,0.0178164887288322,
0.0412392671339201));
#42514=CARTESIAN_POINT('Ctrl Pts',(-0.117591431864639,2.92794590778002E-5,
0.0424367114736158));
#42515=CARTESIAN_POINT('Origin',(0.,0.,0.));
#42516=CARTESIAN_POINT('Ctrl Pts',(-0.0510216505388444,0.106149619882937,
-0.0164977839420935));
#42517=CARTESIAN_POINT('Ctrl Pts',(-0.0861748725546967,0.0892529469510397,
-0.0138624428755877));
#42518=CARTESIAN_POINT('Ctrl Pts',(-0.137790539141881,0.0181049606281334,
-0.0085917607425761));
#42519=CARTESIAN_POINT('Ctrl Pts',(-0.0902797247787074,-0.10582739645577,
-0.000685737543058663));
#42520=CARTESIAN_POINT('Ctrl Pts',(0.0393629057248093,-0.133280773711466,
0.00722028565645879));
#42521=CARTESIAN_POINT('Ctrl Pts',(0.133186295059001,-0.0398205273591854,
0.0151263088559762));
#42522=CARTESIAN_POINT('Ctrl Pts',(0.106043485420733,0.0899039768168324,
0.0230323320554937));
#42523=CARTESIAN_POINT('Ctrl Pts',(-0.0174538572390982,0.137906280269365,
0.0309383552550111));
#42524=CARTESIAN_POINT('Ctrl Pts',(-0.125086200033906,0.0606479146403327,
0.0388443784545286));
#42525=CARTESIAN_POINT('Ctrl Pts',(-0.119084788854313,-0.0717206569949895,
0.046750401654046));
#42526=CARTESIAN_POINT('Ctrl Pts',(-0.00489492837772915,-0.138925734589418,
0.0546564248535634));
#42527=CARTESIAN_POINT('Ctrl Pts',(0.113740629398734,-0.0799231888543136,
0.062562448053081));
#42528=CARTESIAN_POINT('Ctrl Pts',(0.129045816271948,0.0516898037714297,
0.0704684712525983));
#42529=CARTESIAN_POINT('Ctrl Pts',(0.0271151839788463,0.136342686033388,
0.0783744944521158));
#42530=CARTESIAN_POINT('Ctrl Pts',(-0.0994488545192835,0.097131556418157,
0.0862805176516332));
#42531=CARTESIAN_POINT('Ctrl Pts',(-0.135665746467832,-0.0303218706918135,
0.0941865408511506));
#42532=CARTESIAN_POINT('Ctrl Pts',(-0.0486330432543111,-0.130228357167641,
0.102092564050668));
#42533=CARTESIAN_POINT('Ctrl Pts',(0.0825817545836372,-0.111825131042891,
0.109998587250186));
#42534=CARTESIAN_POINT('Ctrl Pts',(0.138772738128538,0.00816897019039422,
0.117904610449703));
#42535=CARTESIAN_POINT('Ctrl Pts',(0.0688915313895657,0.120741708772585,
0.12581063364922));
#42536=CARTESIAN_POINT('Ctrl Pts',(-0.0635762130827019,0.123623095373164,
0.133716656848738));
#42537=CARTESIAN_POINT('Ctrl Pts',(-0.138286275523292,0.014195432572335,
0.141622680048255));
#42538=CARTESIAN_POINT('Ctrl Pts',(-0.0873660952430369,-0.108128486159945,
0.149528703247773));
#42539=CARTESIAN_POINT('Ctrl Pts',(0.0429243879661372,-0.132219897211806,
0.15743472644729));
#42540=CARTESIAN_POINT('Ctrl Pts',(0.134218946443888,-0.0361922458912883,
0.165340749646808));
#42541=CARTESIAN_POINT('Ctrl Pts',(0.103578348063976,0.0927153171784346,
0.173246772846325));
#42542=CARTESIAN_POINT('Ctrl Pts',(-0.0211610525014389,0.137392918706172,
0.181152796045843));
#42543=CARTESIAN_POINT('Ctrl Pts',(-0.126676071448117,0.0572518747851005,
0.18905881924536));
#42544=CARTESIAN_POINT('Ctrl Pts',(-0.117108480713923,-0.074901321664099,
0.196964842444878));
#42545=CARTESIAN_POINT('Ctrl Pts',(-0.00115024004832317,-0.139008205490464,
0.204870865644395));
#42546=CARTESIAN_POINT('Ctrl Pts',(0.115852970087698,-0.0768289890996742,
0.212776888843912));
#42547=CARTESIAN_POINT('Ctrl Pts',(0.127606135899372,0.055147786219953,
0.22068291204343));
#42548=CARTESIAN_POINT('Ctrl Pts',(0.0234317475993789,0.137023930205902,
0.228588935242947));
#42549=CARTESIAN_POINT('Ctrl Pts',(-0.102029902232137,0.0944166473397004,
0.236494958442465));
#42550=CARTESIAN_POINT('Ctrl Pts',(-0.134799481036655,-0.0339662208175969,
0.244400981641982));
#42551=CARTESIAN_POINT('Ctrl Pts',(-0.0451064993838265,-0.131491474848312,
0.252307004841499));
#42552=CARTESIAN_POINT('Ctrl Pts',(0.0855648107118161,-0.1095594241143,
0.260213028041017));
#42553=CARTESIAN_POINT('Ctrl Pts',(0.138502247321704,0.0119051136596435,
0.268119051240535));
#42554=CARTESIAN_POINT('Ctrl Pts',(0.0656132363391791,0.122554100141606,
0.276025074440052));
#42555=CARTESIAN_POINT('Ctrl Pts',(-0.066884052510702,0.121865203254083,
0.283931097639569));
#42556=CARTESIAN_POINT('Ctrl Pts',(-0.138618553097211,0.010464271673199,
0.291837120839087));
#42557=CARTESIAN_POINT('Ctrl Pts',(-0.0844209446825288,-0.110443235842333,
0.299743144038604));
#42558=CARTESIAN_POINT('Ctrl Pts',(0.046471358419155,-0.131015331511595,
0.307649167238122));
#42559=CARTESIAN_POINT('Ctrl Pts',(0.135145386671506,-0.0325626888604762,
0.315555190437639));
#42560=CARTESIAN_POINT('Ctrl Pts',(0.101042606300054,0.0954724879559945,
0.323461213637157));
#42561=CARTESIAN_POINT('Ctrl Pts',(-0.0248553070174182,0.136772869961425,
0.331367236836674));
#42562=CARTESIAN_POINT('Ctrl Pts',(-0.12817268430534,0.0538179081940093,
0.339273260036191));
#42563=CARTESIAN_POINT('Ctrl Pts',(-0.115047809886908,-0.0780295180341452,
0.347179283235709));
#42564=CARTESIAN_POINT('Ctrl Pts',(0.00259563734382704,-0.138988729439456,
0.355085306435226));
#42565=CARTESIAN_POINT('Ctrl Pts',(0.117881001348277,-0.0736795342380946,
0.362991329634744));
#42566=CARTESIAN_POINT('Ctrl Pts',(0.12607389627645,0.0585660048329233,
0.370897352834261));
#42567=CARTESIAN_POINT('Ctrl Pts',(0.0197312453245754,0.137605531147394,
0.378803376033779));
#42568=CARTESIAN_POINT('Ctrl Pts',(-0.104536836829869,0.0916332580999962,
0.386709399233296));
#42569=CARTESIAN_POINT('Ctrl Pts',(-0.133835349354862,-0.0375859482716227,
0.394615422432814));
#42570=CARTESIAN_POINT('Ctrl Pts',(-0.0415471952570256,-0.13265909245389,
0.40252144563233));
#42571=CARTESIAN_POINT('Ctrl Pts',(0.0884857325734624,-0.107214175253801,
0.410427468831849));
#42572=CARTESIAN_POINT('Ctrl Pts',(0.138131189387156,0.0156326185555932,
0.418333492031365));
#42573=CARTESIAN_POINT('Ctrl Pts',(0.062287297122381,0.124277499418049,
0.426239515230884));
#42574=CARTESIAN_POINT('Ctrl Pts',(-0.0701433255283678,0.120018824057881,
0.4341455384304));
#42575=CARTESIAN_POINT('Ctrl Pts',(-0.138850177307333,0.00672551158926456,
0.442051561629919));
#42576=CARTESIAN_POINT('Ctrl Pts',(-0.0814144942465354,-0.11267779005197,
0.449957584829435));
#42577=CARTESIAN_POINT('Ctrl Pts',(0.0499845850166584,-0.129715633233345,
0.457863608028953));
#42578=CARTESIAN_POINT('Ctrl Pts',(0.135973695209673,-0.0289094872912353,
0.465769631228471));
#42579=CARTESIAN_POINT('Ctrl Pts',(0.0984334954810092,0.0981603342078928,
0.473675654427988));
#42580=CARTESIAN_POINT('Ctrl Pts',(-0.0285315135918273,0.136053507770195,
0.481581677627505));
#42581=CARTESIAN_POINT('Ctrl Pts',(-0.129576228451988,0.0503448633385094,
0.489487700827023));
#42582=CARTESIAN_POINT('Ctrl Pts',(-0.112903600569895,-0.0811010556205559,
0.49739372402654));
#42583=CARTESIAN_POINT('Ctrl Pts',(0.00633962999064621,-0.138868330932566,
0.505299747226058));
#42584=CARTESIAN_POINT('Ctrl Pts',(0.119823436886959,-0.0704765792090683,
0.513205770425575));
#42585=CARTESIAN_POINT('Ctrl Pts',(0.124450111907394,0.0619416975118724,
0.521111793625093));
#42586=CARTESIAN_POINT('Ctrl Pts',(0.0160164158031762,0.138087213996209,
0.52901781682461));
#42587=CARTESIAN_POINT('Ctrl Pts',(-0.106967865166254,0.0887833321417318,
0.536923840024128));
#42588=CARTESIAN_POINT('Ctrl Pts',(-0.132774037183017,-0.0411783838262002,
0.544829863223645));
#42589=CARTESIAN_POINT('Ctrl Pts',(-0.0379577228913647,-0.133730383672961,
0.552735886423163));
#42590=CARTESIAN_POINT('Ctrl Pts',(0.0913424031974019,-0.104791076063462,
0.56064190962268));
#42591=CARTESIAN_POINT('Ctrl Pts',(0.137659831668342,0.0193487722984857,
0.568547932822197));
#42592=CARTESIAN_POINT('Ctrl Pts',(0.0589161298691768,0.125910658348106,
0.576453956021715));
#42593=CARTESIAN_POINT('Ctrl Pts',(-0.0733516660922674,0.11808529682354,
0.584359979221232));
#42594=CARTESIAN_POINT('Ctrl Pts',(-0.138980979661871,0.00298186797856315,
0.59226600242075));
#42595=CARTESIAN_POINT('Ctrl Pts',(-0.0783489271385985,-0.114830526693234,
0.600172025620267));
#42596=CARTESIAN_POINT('Ctrl Pts',(0.0534615168199478,-0.12832174587234,
0.608078048819785));
#42597=CARTESIAN_POINT('Ctrl Pts',(0.136703270562712,-0.0252352939724056,
0.615984072019302));
#42598=CARTESIAN_POINT('Ctrl Pts',(0.0957529101571512,0.100776904302778,
0.623890095218819));
#42599=CARTESIAN_POINT('Ctrl Pts',(-0.0321870028708045,0.135235354440354,
0.631796118418337));
#42600=CARTESIAN_POINT('Ctrl Pts',(-0.130885684740464,0.0468352620836017,
0.639702141617854));
#42601=CARTESIAN_POINT('Ctrl Pts',(-0.110677409719003,-0.0841137041290149,
0.647608164817372));
#42602=CARTESIAN_POINT('Ctrl Pts',(0.0100790193068892,-0.138647097388359,
0.655514188016889));
#42603=CARTESIAN_POINT('Ctrl Pts',(0.121678866262096,-0.0672224497442505,
0.663420211216407));
#42604=CARTESIAN_POINT('Ctrl Pts',(0.122735961854403,0.0652724131012164,
0.671326234415924));
#42605=CARTESIAN_POINT('Ctrl Pts',(0.0122899564463577,0.138468628991968,
0.679232257615441));
#42606=CARTESIAN_POINT('Ctrl Pts',(-0.109321222024174,0.0858689388531973,
0.687138280814959));
#42607=CARTESIAN_POINT('Ctrl Pts',(-0.131616315159593,-0.0447409189438641,
0.695044304014476));
#42608=CARTESIAN_POINT('Ctrl Pts',(-0.0343406886760894,-0.134704570618338,
0.702950327213994));
#42609=CARTESIAN_POINT('Ctrl Pts',(0.0941327483034478,-0.102291886006113,
0.710856350413511));
#42610=CARTESIAN_POINT('Ctrl Pts',(0.137088516418336,0.0230508765206803,
0.718762373613029));
#42611=CARTESIAN_POINT('Ctrl Pts',(0.0555021824679276,0.127452391053421,
0.726668396812546));
#42612=CARTESIAN_POINT('Ctrl Pts',(-0.0765067445957343,0.116066025541209,
0.734574420012063));
#42613=CARTESIAN_POINT('Ctrl Pts',(-0.139010865120405,-0.000763940859230431,
0.742480443211581));
#42614=CARTESIAN_POINT('Ctrl Pts',(-0.0752264694457675,-0.116899882557203,
0.750386466411098));
#42615=CARTESIAN_POINT('Ctrl Pts',(0.0568996293847587,-0.126834681679914,
0.758292489610617));
#42616=CARTESIAN_POINT('Ctrl Pts',(0.137333582544999,-0.0215427765762162,
0.766198512810132));
#42617=CARTESIAN_POINT('Ctrl Pts',(0.0930027975645983,0.103320297856606,
0.774104536009652));
#42618=CARTESIAN_POINT('Ctrl Pts',(-0.035819122070238,0.13431900488649,
0.782010559209168));
#42619=CARTESIAN_POINT('Ctrl Pts',(-0.13210009942588,0.0432916512297215,
0.789916582408685));
#42620=CARTESIAN_POINT('Ctrl Pts',(-0.108370859366875,-0.0870652729953126,
0.797822605608204));
#42621=CARTESIAN_POINT('Ctrl Pts',(0.0138111005924944,-0.138325195186183,
0.80572862880772));
#42622=CARTESIAN_POINT('Ctrl Pts',(0.123445922182148,-0.0639194978340518,
0.813634652007238));
#42623=CARTESIAN_POINT('Ctrl Pts',(0.120932728835538,0.0685557124046954,
0.821540675206756));
#42624=CARTESIAN_POINT('Ctrl Pts',(0.0085545008581314,0.138749538494654,
0.829446698406273));
#42625=CARTESIAN_POINT('Ctrl Pts',(-0.111595061352101,0.0828921197631381,
0.837352721605791));
#42626=CARTESIAN_POINT('Ctrl Pts',(-0.130363284584795,-0.0482708249720888,
0.845258744805308));
#42627=CARTESIAN_POINT('Ctrl Pts',(-0.0306982239304521,-0.135581215292453,
0.853164768004825));
#42628=CARTESIAN_POINT('Ctrl Pts',(0.0968538014257187,-0.0997179081430208,
0.861070791204343));
#42629=CARTESIAN_POINT('Ctrl Pts',(0.136419444538435,0.0267352712365894,
0.86897681440386));
#42630=CARTESIAN_POINT('Ctrl Pts',(0.0520445414416943,0.128903423908239,
0.876882837603378));
#42631=CARTESIAN_POINT('Ctrl Pts',(-0.0795998263876522,0.113958970288921,
0.884788860802895));
#42632=CARTESIAN_POINT('Ctrl Pts',(-0.138952053011478,-0.00450253390371847,
0.892694884002413));
#42633=CARTESIAN_POINT('Ctrl Pts',(-0.0720261204166176,-0.118897020856024,
0.90060090720193));
#42634=CARTESIAN_POINT('Ctrl Pts',(0.0602520802431792,-0.125231345176025,
0.908506930401448));
#42635=CARTESIAN_POINT('Ctrl Pts',(0.137949690524835,-0.017881538827179,
0.916412953600965));
#42636=CARTESIAN_POINT('Ctrl Pts',(0.0900118016872842,0.105886249500893,
0.924318976800482));
#42637=CARTESIAN_POINT('Ctrl Pts',(0.00399973323748277,0.12400080376067,
0.929589658933494));
#42638=CARTESIAN_POINT('Ctrl Pts',(-0.0334019664626807,0.112939183906322,
0.932225));
#42639=CARTESIAN_POINT('Ctrl Pts',(-0.0551480035117367,0.114734422509853,
-0.0109985226280624));
#42640=CARTESIAN_POINT('Ctrl Pts',(-0.0931442265014884,0.0964712387762041,
-0.00836318156155655));
#42641=CARTESIAN_POINT('Ctrl Pts',(-0.148934286841532,0.0195691911522949,
-0.00309249942854491));
#42642=CARTESIAN_POINT('Ctrl Pts',(-0.097581056797534,-0.114386139408358,
0.00481352377097251));
#42643=CARTESIAN_POINT('Ctrl Pts',(0.0425463629697991,-0.144059796166161,
0.01271954697049));
#42644=CARTESIAN_POINT('Ctrl Pts',(0.143957676595294,-0.0430409945474375,
0.0206255701700074));
#42645=CARTESIAN_POINT('Ctrl Pts',(0.114619704470892,0.0971749203887298,
0.0285315933695248));
#42646=CARTESIAN_POINT('Ctrl Pts',(-0.0188654300703636,0.149059388480494,
0.0364376165690423));
#42647=CARTESIAN_POINT('Ctrl Pts',(-0.13520249003877,0.065552787380297,
0.0443436397685597));
#42648=CARTESIAN_POINT('Ctrl Pts',(-0.128715717437097,-0.0775210327782809,
0.0522496629680772));
#42649=CARTESIAN_POINT('Ctrl Pts',(-0.0052908035023142,-0.150161290708834,
0.0601556861675946));
#42650=CARTESIAN_POINT('Ctrl Pts',(0.122939351496148,-0.0863869407017978,
0.0680617093671122));
#42651=CARTESIAN_POINT('Ctrl Pts',(0.139482338453993,0.0558701933356218,
0.0759677325666295));
#42652=CARTESIAN_POINT('Ctrl Pts',(0.0293081122522375,0.147369339265975,
0.0838737557661469));
#42653=CARTESIAN_POINT('Ctrl Pts',(-0.10749173576994,0.104987027230155,
0.0917797789656645));
#42654=CARTESIAN_POINT('Ctrl Pts',(-0.146637652518404,-0.032774138306667,
0.0996858021651818));
#42655=CARTESIAN_POINT('Ctrl Pts',(-0.0525662186905025,-0.140760516811213,
0.107591825364699));
#42656=CARTESIAN_POINT('Ctrl Pts',(0.089260516735274,-0.120868938074804,
0.115497848564217));
#42657=CARTESIAN_POINT('Ctrl Pts',(0.149995920728193,0.0088296319697477,
0.123403871763734));
#42658=CARTESIAN_POINT('Ctrl Pts',(0.0744631029156597,0.130506640006368,
0.131309894963252));
#42659=CARTESIAN_POINT('Ctrl Pts',(-0.0687179106383172,0.133621057448557,
0.139215918162769));
#42660=CARTESIAN_POINT('Ctrl Pts',(-0.149470115679177,0.0153434817784622,
0.147121941362287));
#42661=CARTESIAN_POINT('Ctrl Pts',(-0.0944317887874227,-0.116873328704402,
0.155027964561804));
#42662=CARTESIAN_POINT('Ctrl Pts',(0.0463958784809096,-0.142913121758123,
0.162933987761322));
#42663=CARTESIAN_POINT('Ctrl Pts',(0.145073843195134,-0.0391192774524402,
0.170840010960839));
#42664=CARTESIAN_POINT('Ctrl Pts',(0.111955200242363,0.10021362663396,0.178746034160356));
#42665=CARTESIAN_POINT('Ctrl Pts',(-0.0228724430773341,0.148504509032441,
0.186652057359874));
#42666=CARTESIAN_POINT('Ctrl Pts',(-0.136920941586459,0.0618820943336314,
0.194558080559391));
#42667=CARTESIAN_POINT('Ctrl Pts',(-0.12657957626731,-0.0809589322677961,
0.202464103758909));
#42668=CARTESIAN_POINT('Ctrl Pts',(-0.00124326519339163,-0.150250431406802,
0.210370126958426));
#42669=CARTESIAN_POINT('Ctrl Pts',(0.125222526785514,-0.0830424989377088,
0.218276150157944));
#42670=CARTESIAN_POINT('Ctrl Pts',(0.137926224580685,0.0596078385548706,
0.226182173357461));
#42671=CARTESIAN_POINT('Ctrl Pts',(0.0253267796170755,0.148105678753651,
0.234088196556978));
#42672=CARTESIAN_POINT('Ctrl Pts',(-0.110281524552332,0.102052551104597,
0.241994219756496));
#42673=CARTESIAN_POINT('Ctrl Pts',(-0.145701328261229,-0.036713223605009,
0.249900242956013));
#42674=CARTESIAN_POINT('Ctrl Pts',(-0.0487544671752176,-0.142125788564551,
0.25780626615553));
#42675=CARTESIAN_POINT('Ctrl Pts',(0.0924848261822464,-0.11841999312036,
0.265712289355049));
#42676=CARTESIAN_POINT('Ctrl Pts',(0.149703554099366,0.012867934356803,
0.273618312554565));
#42677=CARTESIAN_POINT('Ctrl Pts',(0.0709196772318203,0.132465607709839,
0.281524335754083));
#42678=CARTESIAN_POINT('Ctrl Pts',(-0.0722932700879834,0.131720996597282,
0.289430358953601));
#42679=CARTESIAN_POINT('Ctrl Pts',(-0.149829266052005,0.0113105649246307,
0.297336382153118));
#42680=CARTESIAN_POINT('Ctrl Pts',(-0.0912484505038084,-0.119375282723234,
0.305242405352635));
#42681=CARTESIAN_POINT('Ctrl Pts',(0.0502297085693762,-0.141611137350254,
0.313148428552153));
#42682=CARTESIAN_POINT('Ctrl Pts',(0.14607520885827,-0.0351961816339526,
0.32105445175167));
#42683=CARTESIAN_POINT('Ctrl Pts',(0.109214381507085,0.103193782354472,
0.328960474951188));
#42684=CARTESIAN_POINT('Ctrl Pts',(-0.0268654687609187,0.147834314125149,
0.336866498150705));
#42685=CARTESIAN_POINT('Ctrl Pts',(-0.13853859233343,0.0581704072434516,
0.344772521350223));
#42686=CARTESIAN_POINT('Ctrl Pts',(-0.124352249616671,-0.0843401201082281,
0.35267854454974));
#42687=CARTESIAN_POINT('Ctrl Pts',(0.00280555834318869,-0.150229380238954,
0.360584567749258));
#42688=CARTESIAN_POINT('Ctrl Pts',(0.127414574159504,-0.0796383333348297,
0.368490590948775));
#42689=CARTESIAN_POINT('Ctrl Pts',(0.136270065769409,0.0633025040563021,
0.376396614148293));
#42690=CARTESIAN_POINT('Ctrl Pts',(0.0213270008899901,0.148734316408943,
0.38430263734781));
#42691=CARTESIAN_POINT('Ctrl Pts',(-0.112991206354848,0.0990440565156409,
0.392208660547328));
#42692=CARTESIAN_POINT('Ctrl Pts',(-0.144659222864564,-0.0406256948841215,
0.400114683746845));
#42693=CARTESIAN_POINT('Ctrl Pts',(-0.0449073059326639,-0.143387836717301,
0.408020706946362));
#42694=CARTESIAN_POINT('Ctrl Pts',(0.0956419762819073,-0.115885073316145,
0.41592673014588));
#42695=CARTESIAN_POINT('Ctrl Pts',(0.149302487021736,0.0168968995298395,
0.423832753345397));
#42696=CARTESIAN_POINT('Ctrl Pts',(0.0673247541811015,0.134328386125389,
0.431738776544915));
#42697=CARTESIAN_POINT('Ctrl Pts',(-0.0758161353407861,0.129725292316436,
0.439644799744432));
#42698=CARTESIAN_POINT('Ctrl Pts',(-0.150079622765641,0.007269434305358,
0.447550822943949));
#42699=CARTESIAN_POINT('Ctrl Pts',(-0.0879988547449296,-0.121790555496631,
0.455456846143467));
#42700=CARTESIAN_POINT('Ctrl Pts',(0.0540270657832349,-0.140206326560007,
0.463362869342984));
#42701=CARTESIAN_POINT('Ctrl Pts',(0.146970506475833,-0.0312475290356562,
0.471268892542502));
#42702=CARTESIAN_POINT('Ctrl Pts',(0.106394260027447,0.106099006959581,
0.479174915742019));
#42703=CARTESIAN_POINT('Ctrl Pts',(-0.0308389868837996,0.147056773841187,
0.487080938941536));
#42704=CARTESIAN_POINT('Ctrl Pts',(-0.140055647479839,0.0544164814518564,
0.494986962141054));
#42705=CARTESIAN_POINT('Ctrl Pts',(-0.122034628338338,-0.0876600669114554,
0.502892985340571));
#42706=CARTESIAN_POINT('Ctrl Pts',(0.00685234470650933,-0.150099244557128,
0.51079900854009));
#42707=CARTESIAN_POINT('Ctrl Pts',(0.129514103296199,-0.076176340762594,
0.518705031739606));
#42708=CARTESIAN_POINT('Ctrl Pts',(0.134514958571949,0.066951204357981,
0.526611054939125));
#42709=CARTESIAN_POINT('Ctrl Pts',(0.0173117362067031,0.149254955140882,
0.534517078138641));
#42710=CARTESIAN_POINT('Ctrl Pts',(-0.11561884301137,0.0959636440810236,
0.542423101338159));
#42711=CARTESIAN_POINT('Ctrl Pts',(-0.143512077549549,-0.0445086670437286,
0.550329124537675));
#42712=CARTESIAN_POINT('Ctrl Pts',(-0.0410275366085405,-0.144545768130486,
0.558235147737195));
#42713=CARTESIAN_POINT('Ctrl Pts',(0.098729678853994,-0.113266007071779,
0.56614117093671));
#42714=CARTESIAN_POINT('Ctrl Pts',(0.14879300846003,0.0209135955304358,
0.57404719413623));
#42715=CARTESIAN_POINT('Ctrl Pts',(0.0636809452969333,0.136093626047241,
0.581953217335745));
#42716=CARTESIAN_POINT('Ctrl Pts',(-0.0792839490005986,0.127635391939178,
0.589859240535265));
#42717=CARTESIAN_POINT('Ctrl Pts',(-0.150221003701602,0.00322302520629366,
0.59776526373478));
#42718=CARTESIAN_POINT('Ctrl Pts',(-0.0846853612799296,-0.124117393742718,
0.605671286934299));
#42719=CARTESIAN_POINT('Ctrl Pts',(0.0577851928777687,-0.138699709187424,
0.613577310133815));
#42720=CARTESIAN_POINT('Ctrl Pts',(0.147759085906459,-0.0272761869894916,
0.621483333333334));
#42721=CARTESIAN_POINT('Ctrl Pts',(0.103496883574659,0.108927190980628,
0.62938935653285));
#42722=CARTESIAN_POINT('Ctrl Pts',(-0.0347901122093251,0.146172452729842,
0.637295379732368));
#42723=CARTESIAN_POINT('Ctrl Pts',(-0.141471005454986,0.0506230427785409,
0.645201402931886));
#42724=CARTESIAN_POINT('Ctrl Pts',(-0.119628395306551,-0.0909163620091147,
0.653107426131403));
#42725=CARTESIAN_POINT('Ctrl Pts',(0.0108941554469695,-0.149860118849825,
0.661013449330921));
#42726=CARTESIAN_POINT('Ctrl Pts',(0.131519589685118,-0.0726590350451557,
0.668919472530437));
#42727=CARTESIAN_POINT('Ctrl Pts',(0.132662177406628,0.0705512900682209,
0.676825495729956));
#42728=CARTESIAN_POINT('Ctrl Pts',(0.0132839011303035,0.149667216902378,
0.684731518929473));
#42729=CARTESIAN_POINT('Ctrl Pts',(-0.118162526543641,0.0928135505498801,
0.69263754212899));
#42730=CARTESIAN_POINT('Ctrl Pts',(-0.142260725279696,-0.0483593205820741,
0.700543565328508));
#42731=CARTESIAN_POINT('Ctrl Pts',(-0.0371179763826477,-0.145598742005641,
0.708449588528025));
#42732=CARTESIAN_POINT('Ctrl Pts',(0.101745691861845,-0.110564696145857,
0.716355611727543));
#42733=CARTESIAN_POINT('Ctrl Pts',(0.148175488346884,0.0249151057616852,
0.72426163492706));
#42734=CARTESIAN_POINT('Ctrl Pts',(0.0599908964395442,0.137760045689666,
0.732167658126578));
#42735=CARTESIAN_POINT('Ctrl Pts',(-0.0826941930548661,0.125452813002725,
0.740073681326094));
#42736=CARTESIAN_POINT('Ctrl Pts',(-0.150253306133115,-0.000825724231627113,
0.747979704525614));
#42737=CARTESIAN_POINT('Ctrl Pts',(-0.081310376229644,-0.126354107828757,
0.755885727725129));
#42738=CARTESIAN_POINT('Ctrl Pts',(0.0615013612454227,-0.137092379349209,
0.763791750924648));
#42739=CARTESIAN_POINT('Ctrl Pts',(0.148440374085997,-0.0232850389144764,
0.771697774124165));
#42740=CARTESIAN_POINT('Ctrl Pts',(0.100524356866682,0.111676280340869,
0.779603797323682));
#42741=CARTESIAN_POINT('Ctrl Pts',(-0.0387159774106656,0.145181993819149,
0.7875098205232));
#42742=CARTESIAN_POINT('Ctrl Pts',(-0.142783635380297,0.0467928439952764,
0.795415843722717));
#42743=CARTESIAN_POINT('Ctrl Pts',(-0.117135303735115,-0.0941066376761042,
0.803321866922235));
#42744=CARTESIAN_POINT('Ctrl Pts',(0.0149280671231108,-0.149512182952249,
0.811227890121752));
#42745=CARTESIAN_POINT('Ctrl Pts',(0.133429555455635,-0.0690889583890887,
0.819133913321269));
#42746=CARTESIAN_POINT('Ctrl Pts',(0.13071310873075,0.0741001247218646,
0.827039936520788));
#42747=CARTESIAN_POINT('Ctrl Pts',(0.00924634225633868,0.149970844834382,
0.834945959720303));
#42748=CARTESIAN_POINT('Ctrl Pts',(-0.120620261601548,0.0895959825586721,
0.842851982919823));
#42749=CARTESIAN_POINT('Ctrl Pts',(-0.140906356422368,-0.0521747061680897,
0.850758006119338));
#42750=CARTESIAN_POINT('Ctrl Pts',(-0.0331809289437206,-0.146546284922345,
0.858664029318857));
#42751=CARTESIAN_POINT('Ctrl Pts',(0.104686808927989,-0.107782548984136,
0.866570052518374));
#42752=CARTESIAN_POINT('Ctrl Pts',(0.147452305580495,0.0288974742383162,
0.874476075717892));
#42753=CARTESIAN_POINT('Ctrl Pts',(0.0562536202549592,0.139328430172098,
0.882382098917409));
#42754=CARTESIAN_POINT('Ctrl Pts',(-0.0860374264415029,0.123175350607342,
0.890288122116927));
#42755=CARTESIAN_POINT('Ctrl Pts',(-0.150189737621406,-0.00486667430221375,
0.898194145316444));
#42756=CARTESIAN_POINT('Ctrl Pts',(-0.0778512004163494,-0.128512763786642,
0.906100168515961));
#42757=CARTESIAN_POINT('Ctrl Pts',(0.0651249400548213,-0.135359373728788,
0.914006191715479));
#42758=CARTESIAN_POINT('Ctrl Pts',(0.149106309520794,-0.0193277002139675,
0.921912214914997));
#42759=CARTESIAN_POINT('Ctrl Pts',(0.0972914655469444,0.114449752166959,
0.929818238114513));
#42760=CARTESIAN_POINT('Ctrl Pts',(0.00432320985889779,0.134029312831529,
0.935088920247525));
#42761=CARTESIAN_POINT('Ctrl Pts',(-0.0361033354336585,0.122073089461047,
0.937724261314031));
#42762=CARTESIAN_POINT('Ctrl Pts',(-0.0592743564846289,0.123319225136769,
-0.00549926131403118));
#42763=CARTESIAN_POINT('Ctrl Pts',(-0.10011358044828,0.103689530601369,
-0.00286392024752536));
#42764=CARTESIAN_POINT('Ctrl Pts',(-0.160078034541183,0.0210334216764563,
0.00240676188548625));
#42765=CARTESIAN_POINT('Ctrl Pts',(-0.104882388816361,-0.122944882360947,
0.0103127850850037));
#42766=CARTESIAN_POINT('Ctrl Pts',(0.0457298202147887,-0.154838818620857,
0.0182188082845211));
#42767=CARTESIAN_POINT('Ctrl Pts',(0.154729058131587,-0.0462614617356896,
0.0261248314840386));
#42768=CARTESIAN_POINT('Ctrl Pts',(0.123195923521052,0.104445863960627,
0.034030854683556));
#42769=CARTESIAN_POINT('Ctrl Pts',(-0.0202770029016287,0.160212496691623,
0.0419368778830735));
#42770=CARTESIAN_POINT('Ctrl Pts',(-0.145318780043635,0.0704576601202616,
0.049842901082591));
#42771=CARTESIAN_POINT('Ctrl Pts',(-0.138346646019881,-0.0833214085615725,
0.0577489242821084));
#42772=CARTESIAN_POINT('Ctrl Pts',(-0.00568667862689953,-0.16139684682825,
0.0656549474816259));
#42773=CARTESIAN_POINT('Ctrl Pts',(0.132138073593561,-0.0928506925492821,
0.0735609706811433));
#42774=CARTESIAN_POINT('Ctrl Pts',(0.149918860636037,0.060050582899814,
0.0814669938806607));
#42775=CARTESIAN_POINT('Ctrl Pts',(0.031501040525629,0.158395992498563,
0.0893730170801781));
#42776=CARTESIAN_POINT('Ctrl Pts',(-0.115534617020597,0.112842498042153,
0.0972790402796957));
#42777=CARTESIAN_POINT('Ctrl Pts',(-0.157609558568976,-0.0352264059215207,
0.105185063479213));
#42778=CARTESIAN_POINT('Ctrl Pts',(-0.0564993941266941,-0.151292676454786,
0.113091086678731));
#42779=CARTESIAN_POINT('Ctrl Pts',(0.0959392788869109,-0.129912745106718,
0.120997109878248));
#42780=CARTESIAN_POINT('Ctrl Pts',(0.161219103327847,0.00949029374910116,
0.128903133077765));
#42781=CARTESIAN_POINT('Ctrl Pts',(0.0800346744417541,0.140271571240151,
0.136809156277283));
#42782=CARTESIAN_POINT('Ctrl Pts',(-0.0738596081939327,0.143619019523951,
0.1447151794768));
#42783=CARTESIAN_POINT('Ctrl Pts',(-0.160653955835061,0.0164915309845896,
0.152621202676318));
#42784=CARTESIAN_POINT('Ctrl Pts',(-0.101497482331809,-0.125618171248858,
0.160527225875835));
#42785=CARTESIAN_POINT('Ctrl Pts',(0.0498673689956821,-0.15360634630444,
0.168433249075353));
#42786=CARTESIAN_POINT('Ctrl Pts',(0.15592873994638,-0.0420463090135921,
0.17633927227487));
#42787=CARTESIAN_POINT('Ctrl Pts',(0.120332052420749,0.107711936089485,
0.184245295474388));
#42788=CARTESIAN_POINT('Ctrl Pts',(-0.0245838336532294,0.15961609935871,
0.192151318673905));
#42789=CARTESIAN_POINT('Ctrl Pts',(-0.147165811724802,0.0665123138821622,
0.200057341873423));
#42790=CARTESIAN_POINT('Ctrl Pts',(-0.136050671820698,-0.0870165428714931,
0.20796336507294));
#42791=CARTESIAN_POINT('Ctrl Pts',(-0.00133629033845999,-0.16149265732314,
0.215869388272457));
#42792=CARTESIAN_POINT('Ctrl Pts',(0.134592083483329,-0.0892560087757434,
0.223775411471975));
#42793=CARTESIAN_POINT('Ctrl Pts',(0.148246313261997,0.0640678908897882,
0.231681434671492));
#42794=CARTESIAN_POINT('Ctrl Pts',(0.0272218116347722,0.159187427301401,
0.23958745787101));
#42795=CARTESIAN_POINT('Ctrl Pts',(-0.118533146872527,0.109688454869495,
0.247493481070527));
#42796=CARTESIAN_POINT('Ctrl Pts',(-0.156603175485803,-0.0394602263924212,
0.255399504270045));
#42797=CARTESIAN_POINT('Ctrl Pts',(-0.0524024349666086,-0.152760102280791,
0.263305527469562));
#42798=CARTESIAN_POINT('Ctrl Pts',(0.0994048416526766,-0.127280562126421,
0.27121155066908));
#42799=CARTESIAN_POINT('Ctrl Pts',(0.160904860877029,0.0138307550539624,
0.279117573868597));
#42800=CARTESIAN_POINT('Ctrl Pts',(0.0762261181244613,0.142377115278073,
0.287023597068114));
#42801=CARTESIAN_POINT('Ctrl Pts',(-0.0777024876652646,0.141576789940481,
0.294929620267632));
#42802=CARTESIAN_POINT('Ctrl Pts',(-0.1610399790068,0.0121568581760624,
0.302835643467149));
#42803=CARTESIAN_POINT('Ctrl Pts',(-0.098075956325088,-0.128307329604135,
0.310741666666667));
#42804=CARTESIAN_POINT('Ctrl Pts',(0.0539880587195976,-0.152206943188912,
0.318647689866184));
#42805=CARTESIAN_POINT('Ctrl Pts',(0.157005031045033,-0.037829674407429,
0.326553713065702));
#42806=CARTESIAN_POINT('Ctrl Pts',(0.117386156714116,0.11091507675295,0.334459736265219));
#42807=CARTESIAN_POINT('Ctrl Pts',(-0.0288756305044191,0.158895758288873,
0.342365759464736));
#42808=CARTESIAN_POINT('Ctrl Pts',(-0.14890450036152,0.0625229062928939,
0.350271782664254));
#42809=CARTESIAN_POINT('Ctrl Pts',(-0.133656689346435,-0.0906507221823109,
0.358177805863771));
#42810=CARTESIAN_POINT('Ctrl Pts',(0.0030154793425501,-0.161470031038451,
0.366083829063289));
#42811=CARTESIAN_POINT('Ctrl Pts',(0.136948146970731,-0.0855971324315648,
0.373989852262806));
#42812=CARTESIAN_POINT('Ctrl Pts',(0.146466235262368,0.0680390032796811,
0.381895875462324));
#42813=CARTESIAN_POINT('Ctrl Pts',(0.0229227564554051,0.159863101670492,
0.389801898661841));
#42814=CARTESIAN_POINT('Ctrl Pts',(-0.121445575879827,0.106454854931286,
0.397707921861359));
#42815=CARTESIAN_POINT('Ctrl Pts',(-0.155483096374265,-0.0436654414966204,
0.405613945060876));
#42816=CARTESIAN_POINT('Ctrl Pts',(-0.0482674166083024,-0.154116580980712,
0.413519968260394));
#42817=CARTESIAN_POINT('Ctrl Pts',(0.102798219990352,-0.124555971378489,
0.421425991459911));
#42818=CARTESIAN_POINT('Ctrl Pts',(0.160473784656316,0.018161180504086,
0.429332014659428));
#42819=CARTESIAN_POINT('Ctrl Pts',(0.072362211239822,0.144379272832728,
0.437238037858946));
#42820=CARTESIAN_POINT('Ctrl Pts',(-0.0814889451532045,0.139431760574992,
0.445144061058463));
#42821=CARTESIAN_POINT('Ctrl Pts',(-0.16130906822395,0.00781335702145124,
0.453050084257981));
#42822=CARTESIAN_POINT('Ctrl Pts',(-0.0945832152433237,-0.130903320941292,
0.460956107457498));
#42823=CARTESIAN_POINT('Ctrl Pts',(0.0580695465498112,-0.150697019886669,
0.468862130657016));
#42824=CARTESIAN_POINT('Ctrl Pts',(0.157967317741994,-0.033585570780077,
0.476768153856533));
#42825=CARTESIAN_POINT('Ctrl Pts',(0.114355024573885,0.114037679711269,
0.48467417705605));
#42826=CARTESIAN_POINT('Ctrl Pts',(-0.0331464601757716,0.15806003991218,
0.492580200255568));
#42827=CARTESIAN_POINT('Ctrl Pts',(-0.15053506650769,0.0584880995652034,
0.500486223455085));
#42828=CARTESIAN_POINT('Ctrl Pts',(-0.131165656106781,-0.0942190782023548,
0.508392246654604));
#42829=CARTESIAN_POINT('Ctrl Pts',(0.00736505942237213,-0.161330158181689,
0.51629826985412));
#42830=CARTESIAN_POINT('Ctrl Pts',(0.139204769705438,-0.0818761023161199,
0.524204293053638));
#42831=CARTESIAN_POINT('Ctrl Pts',(0.144579805236504,0.0719607112040898,
0.532110316253155));
#42832=CARTESIAN_POINT('Ctrl Pts',(0.0186070566102303,0.160422696285555,
0.540016339452673));
#42833=CARTESIAN_POINT('Ctrl Pts',(-0.124269820856485,0.103143956020315,
0.547922362652189));
#42834=CARTESIAN_POINT('Ctrl Pts',(-0.154250117916081,-0.047838950261257,
0.555828385851708));
#42835=CARTESIAN_POINT('Ctrl Pts',(-0.0440973503257164,-0.15536115258801,
0.563734409051225));
#42836=CARTESIAN_POINT('Ctrl Pts',(0.106116954510586,-0.121740938080097,
0.571640432250743));
#42837=CARTESIAN_POINT('Ctrl Pts',(0.159926185251717,0.022478418762386,
0.579546455450259));
#42838=CARTESIAN_POINT('Ctrl Pts',(0.06844576072469,0.146276593746376,0.587452478649778));
#42839=CARTESIAN_POINT('Ctrl Pts',(-0.08521623190893,0.137185487054817,
0.595358501849294));
#42840=CARTESIAN_POINT('Ctrl Pts',(-0.161461027741333,0.00346418243402402,
0.603264525048813));
#42841=CARTESIAN_POINT('Ctrl Pts',(-0.0910217954212606,-0.133404260792202,
0.611170548248329));
#42842=CARTESIAN_POINT('Ctrl Pts',(0.0621088689355897,-0.149077672502509,
0.619076571447848));
#42843=CARTESIAN_POINT('Ctrl Pts',(0.158814901250206,-0.0293170800065776,
0.626982594647363));
#42844=CARTESIAN_POINT('Ctrl Pts',(0.111240856992166,0.117077477658479,
0.634888617846883));
#42845=CARTESIAN_POINT('Ctrl Pts',(-0.0373932215478457,0.15710955101933,
0.642794641046398));
#42846=CARTESIAN_POINT('Ctrl Pts',(-0.152056326169508,0.0544108234734799,
0.650700664245917));
#42847=CARTESIAN_POINT('Ctrl Pts',(-0.1285793808941,-0.0977190198892145,
0.658606687445434));
#42848=CARTESIAN_POINT('Ctrl Pts',(0.0117092915870499,-0.161073140311291,
0.666512710644951));
#42849=CARTESIAN_POINT('Ctrl Pts',(0.14136031310814,-0.0780956203460609,
0.67441873384447));
#42850=CARTESIAN_POINT('Ctrl Pts',(0.142588392958853,0.0758301670352254,
0.682324757043986));
#42851=CARTESIAN_POINT('Ctrl Pts',(0.0142778458142493,0.160865804812787,
0.690230780243504));
#42852=CARTESIAN_POINT('Ctrl Pts',(-0.127003831063107,0.0997581622465629,
0.698136803443022));
#42853=CARTESIAN_POINT('Ctrl Pts',(-0.152905135399799,-0.0519777222202838,
0.706042826642539));
#42854=CARTESIAN_POINT('Ctrl Pts',(-0.0398952640892059,-0.156492913392945,
0.713948849842056));
#42855=CARTESIAN_POINT('Ctrl Pts',(0.109358635420242,-0.118837506285601,
0.721854873041575));
#42856=CARTESIAN_POINT('Ctrl Pts',(0.159262460275431,0.0267793350026898,
0.729760896241091));
#42857=CARTESIAN_POINT('Ctrl Pts',(0.0644796104111608,0.148067700325911,
0.737666919440608));
#42858=CARTESIAN_POINT('Ctrl Pts',(-0.0888816415139979,0.134839600464242,
0.745572942640127));
#42859=CARTESIAN_POINT('Ctrl Pts',(-0.161495747145824,-0.000887507604023794,
0.753478965839642));
#42860=CARTESIAN_POINT('Ctrl Pts',(-0.0873942830135206,-0.135808333100311,
0.761384989039162));
#42861=CARTESIAN_POINT('Ctrl Pts',(0.0661030931060867,-0.147350077018504,
0.769291012238677));
#42862=CARTESIAN_POINT('Ctrl Pts',(0.159547165626996,-0.0250273012527367,
0.777197035438197));
#42863=CARTESIAN_POINT('Ctrl Pts',(0.108045916168766,0.120032262825132,
0.785103058637712));
#42864=CARTESIAN_POINT('Ctrl Pts',(-0.0416128327510934,0.156044982751807,
0.793009081837232));
#42865=CARTESIAN_POINT('Ctrl Pts',(-0.153467171334714,0.0502940367608314,
0.800915105036747));
#42866=CARTESIAN_POINT('Ctrl Pts',(-0.125899748103356,-0.101148002356896,
0.808821128236267));
#42867=CARTESIAN_POINT('Ctrl Pts',(0.0160450336537275,-0.160699170718315,
0.816727151435783));
#42868=CARTESIAN_POINT('Ctrl Pts',(0.143413188729122,-0.0742584189441255,
0.824633174635301));
#42869=CARTESIAN_POINT('Ctrl Pts',(0.140493488625962,0.0796445370390336,
0.832539197834818));
#42870=CARTESIAN_POINT('Ctrl Pts',(0.00993818365454583,0.161192151174111,
0.840445221034335));
#42871=CARTESIAN_POINT('Ctrl Pts',(-0.129645461850996,0.0962998453542059,
0.848351244233853));
#42872=CARTESIAN_POINT('Ctrl Pts',(-0.151449428259942,-0.0560785873640905,
0.85625726743337));
#42873=CARTESIAN_POINT('Ctrl Pts',(-0.0356636339569891,-0.157511354552237,
0.864163290632887));
#42874=CARTESIAN_POINT('Ctrl Pts',(0.112519816430259,-0.115847189825252,
0.872069313832405));
#42875=CARTESIAN_POINT('Ctrl Pts',(0.158485166622555,0.0310596772400429,
0.879975337031923));
#42876=CARTESIAN_POINT('Ctrl Pts',(0.0604626990682241,0.149753436435956,
0.88788136023144));
#42877=CARTESIAN_POINT('Ctrl Pts',(-0.0924750264953536,0.132391730925763,
0.895787383430957));
#42878=CARTESIAN_POINT('Ctrl Pts',(-0.161427422231335,-0.00523081470070893,
0.903693406630475));
#42879=CARTESIAN_POINT('Ctrl Pts',(-0.083676280416081,-0.13812850671726,
0.911599429829993));
#42880=CARTESIAN_POINT('Ctrl Pts',(0.0699977998664634,-0.145487402281552,
0.91950545302951));
#42881=CARTESIAN_POINT('Ctrl Pts',(0.160262928516753,-0.020773861600756,
0.927411476229027));
#42882=CARTESIAN_POINT('Ctrl Pts',(0.104571129406605,0.123013254833025,
0.935317499428545));
#42883=CARTESIAN_POINT('Ctrl Pts',(0.0046466864803128,0.144057821902388,
0.940588181561556));
#42884=CARTESIAN_POINT('Ctrl Pts',(-0.0388047044046363,0.131206995015772,
0.943223522628062));
#42885=CARTESIAN_POINT('Ctrl Pts',(-0.0634007094575211,0.131904027763685,
0.));
#42886=CARTESIAN_POINT('Ctrl Pts',(-0.107082934395072,0.110907822426533,
0.00263534106650582));
#42887=CARTESIAN_POINT('Ctrl Pts',(-0.171221782240834,0.0224976522006178,
0.00790602319951745));
#42888=CARTESIAN_POINT('Ctrl Pts',(-0.112183720835187,-0.131503625313535,
0.0158120463990349));
#42889=CARTESIAN_POINT('Ctrl Pts',(0.0489132774597784,-0.165617841075552,
0.0237180695985523));
#42890=CARTESIAN_POINT('Ctrl Pts',(0.165500439667881,-0.0494819289239417,
0.0316240927980698));
#42891=CARTESIAN_POINT('Ctrl Pts',(0.131772142571212,0.111716807532525,
0.0395301159975872));
#42892=CARTESIAN_POINT('Ctrl Pts',(-0.0216885757328939,0.171365604902752,
0.0474361391971047));
#42893=CARTESIAN_POINT('Ctrl Pts',(-0.155435070048499,0.0753625328602259,
0.055342162396622));
#42894=CARTESIAN_POINT('Ctrl Pts',(-0.147977574602665,-0.0891217843448639,
0.0632481855961397));
#42895=CARTESIAN_POINT('Ctrl Pts',(-0.00608255375148451,-0.172632402947666,
0.0711542087956569));
#42896=CARTESIAN_POINT('Ctrl Pts',(0.141336795690974,-0.0993144443967663,
0.0790602319951745));
#42897=CARTESIAN_POINT('Ctrl Pts',(0.160355382818083,0.0642309724640062,
0.0869662551946919));
#42898=CARTESIAN_POINT('Ctrl Pts',(0.03369396879902,0.16942264573115,0.0948722783942093));
#42899=CARTESIAN_POINT('Ctrl Pts',(-0.123577498271253,0.120697968854151,
0.102778301593727));
#42900=CARTESIAN_POINT('Ctrl Pts',(-0.168581464619548,-0.0376786735363742,
0.110684324793244));
#42901=CARTESIAN_POINT('Ctrl Pts',(-0.0604325695628853,-0.161824836098358,
0.118590347992762));
#42902=CARTESIAN_POINT('Ctrl Pts',(0.102618041038548,-0.138956552138631,
0.126496371192279));
#42903=CARTESIAN_POINT('Ctrl Pts',(0.172442285927502,0.0101509555284547,
0.134402394391796));
#42904=CARTESIAN_POINT('Ctrl Pts',(0.085606245967848,0.150036502473934,
0.142308417591314));
#42905=CARTESIAN_POINT('Ctrl Pts',(-0.0790013057495479,0.153616981599344,
0.150214440790831));
#42906=CARTESIAN_POINT('Ctrl Pts',(-0.171837795990946,0.0176395801907167,
0.158120463990349));
#42907=CARTESIAN_POINT('Ctrl Pts',(-0.108563175876194,-0.134363013793315,
0.166026487189866));
#42908=CARTESIAN_POINT('Ctrl Pts',(0.0533388595104543,-0.164299570850757,
0.173932510389384));
#42909=CARTESIAN_POINT('Ctrl Pts',(0.166783636697626,-0.0449733405747439,
0.181838533588901));
#42910=CARTESIAN_POINT('Ctrl Pts',(0.128708904599136,0.11521024554501,0.189744556788419));
#42911=CARTESIAN_POINT('Ctrl Pts',(-0.0262952242291247,0.170727689684979,
0.197650579987936));
#42912=CARTESIAN_POINT('Ctrl Pts',(-0.157410681863144,0.071142533430693,
0.205556603187454));
#42913=CARTESIAN_POINT('Ctrl Pts',(-0.145521767374085,-0.0930741534751901,
0.213462626386971));
#42914=CARTESIAN_POINT('Ctrl Pts',(-0.00142931548352814,-0.172734883239477,
0.221368649586489));
#42915=CARTESIAN_POINT('Ctrl Pts',(0.143961640181145,-0.0954695186137778,
0.229274672786006));
#42916=CARTESIAN_POINT('Ctrl Pts',(0.15856640194331,0.0685279432247057,
0.237180695985524));
#42917=CARTESIAN_POINT('Ctrl Pts',(0.0291168436524689,0.17026917584915,
0.24508671918504));
#42918=CARTESIAN_POINT('Ctrl Pts',(-0.126784769192722,0.117324358634392,
0.252992742384559));
#42919=CARTESIAN_POINT('Ctrl Pts',(-0.167505022710376,-0.0422072291798334,
0.260898765584075));
#42920=CARTESIAN_POINT('Ctrl Pts',(-0.0560504027579997,-0.16339441599703,
0.268804788783594));
#42921=CARTESIAN_POINT('Ctrl Pts',(0.106324857123107,-0.136141131132482,
0.27671081198311));
#42922=CARTESIAN_POINT('Ctrl Pts',(0.172106167654692,0.0147935757511219,
0.284616835182629));
#42923=CARTESIAN_POINT('Ctrl Pts',(0.0815325590171024,0.152288622846307,
0.292522858382145));
#42924=CARTESIAN_POINT('Ctrl Pts',(-0.0831117052425459,0.151432583283679,
0.300428881581663));
#42925=CARTESIAN_POINT('Ctrl Pts',(-0.172250691961594,0.0130031514274941,
0.30833490478118));
#42926=CARTESIAN_POINT('Ctrl Pts',(-0.104903462146368,-0.137239376485036,
0.316240927980698));
#42927=CARTESIAN_POINT('Ctrl Pts',(0.0577464088698189,-0.16280274902757,
0.324146951180215));
#42928=CARTESIAN_POINT('Ctrl Pts',(0.167934853231796,-0.0404631671809053,
0.332052974379733));
#42929=CARTESIAN_POINT('Ctrl Pts',(0.125557931921148,0.118636371151428,
0.33995899757925));
#42930=CARTESIAN_POINT('Ctrl Pts',(-0.0308857922479196,0.169957202452597,
0.347865020778768));
#42931=CARTESIAN_POINT('Ctrl Pts',(-0.15927040838961,0.0668754053423362,
0.355771043978284));
#42932=CARTESIAN_POINT('Ctrl Pts',(-0.142961129076198,-0.0969613242563938,
0.363677067177803));
#42933=CARTESIAN_POINT('Ctrl Pts',(0.0032254003419117,-0.172710681837949,
0.371583090377319));
#42934=CARTESIAN_POINT('Ctrl Pts',(0.146481719781958,-0.0915559315282998,
0.379489113576838));
#42935=CARTESIAN_POINT('Ctrl Pts',(0.156662404755327,0.0727755025030601,
0.387395136776354));
#42936=CARTESIAN_POINT('Ctrl Pts',(0.0245185120208197,0.170991886932041,
0.395301159975873));
#42937=CARTESIAN_POINT('Ctrl Pts',(-0.129899945404805,0.113865653346931,
0.403207183175389));
#42938=CARTESIAN_POINT('Ctrl Pts',(-0.166306969883967,-0.0467051881091194,
0.411113206374907));
#42939=CARTESIAN_POINT('Ctrl Pts',(-0.0516275272839405,-0.164845325244123,
0.419019229574424));
#42940=CARTESIAN_POINT('Ctrl Pts',(0.109954463698797,-0.133226869440833,
0.426925252773942));
#42941=CARTESIAN_POINT('Ctrl Pts',(0.171645082290897,0.0194254614783324,
0.434831275973459));
#42942=CARTESIAN_POINT('Ctrl Pts',(0.0773996682985425,0.154430159540067,
0.442737299172977));
#42943=CARTESIAN_POINT('Ctrl Pts',(-0.0871617549656229,0.149138228833548,
0.450643322372495));
#42944=CARTESIAN_POINT('Ctrl Pts',(-0.172538513682259,0.00835727973754467,
0.458549345572012));
#42945=CARTESIAN_POINT('Ctrl Pts',(-0.101167575741718,-0.140016086385953,
0.466455368771529));
#42946=CARTESIAN_POINT('Ctrl Pts',(0.0621120273163875,-0.161187713213332,
0.474361391971047));
#42947=CARTESIAN_POINT('Ctrl Pts',(0.168964129008155,-0.0359236125244978,
0.482267415170563));
#42948=CARTESIAN_POINT('Ctrl Pts',(0.122315789120323,0.121976352462958,
0.490173438370083));
#42949=CARTESIAN_POINT('Ctrl Pts',(-0.0354539334677437,0.169063305983172,
0.498079461569598));
#42950=CARTESIAN_POINT('Ctrl Pts',(-0.161014485535541,0.0625597176785504,
0.505985484769117));
#42951=CARTESIAN_POINT('Ctrl Pts',(-0.140296683875224,-0.100778089493254,
0.513891507968634));
#42952=CARTESIAN_POINT('Ctrl Pts',(0.00787777413823514,-0.17256107180625,
0.521797531168151));
#42953=CARTESIAN_POINT('Ctrl Pts',(0.148895436114678,-0.0875758638696457,
0.529703554367669));
#42954=CARTESIAN_POINT('Ctrl Pts',(0.154644651901059,0.0769702180501986,
0.537609577567186));
#42955=CARTESIAN_POINT('Ctrl Pts',(0.0199023770137573,0.171590437430228,
0.545515600766704));
#42956=CARTESIAN_POINT('Ctrl Pts',(-0.132920798701601,0.110324267959608,
0.553421623966221));
#42957=CARTESIAN_POINT('Ctrl Pts',(-0.164988158282613,-0.0511692334787857,
0.561327647165738));
#42958=CARTESIAN_POINT('Ctrl Pts',(-0.0471671640428923,-0.166176537045534,
0.569233670365257));
#42959=CARTESIAN_POINT('Ctrl Pts',(0.113504230167178,-0.130215869088414,
0.577139693564773));
#42960=CARTESIAN_POINT('Ctrl Pts',(0.171059362043405,0.0240432419943362,
0.585045716764291));
#42961=CARTESIAN_POINT('Ctrl Pts',(0.0732105761524465,0.156459561445511,
0.592951739963808));
#42962=CARTESIAN_POINT('Ctrl Pts',(-0.0911485148172611,0.146735582170455,
0.600857763163326));
#42963=CARTESIAN_POINT('Ctrl Pts',(-0.172701051781065,0.00370533966175465,
0.608763786362843));
#42964=CARTESIAN_POINT('Ctrl Pts',(-0.0973582295625918,-0.142691127841686,
0.616669809562361));
#42965=CARTESIAN_POINT('Ctrl Pts',(0.0664325449934107,-0.159455635817593,
0.624575832761878));
#42966=CARTESIAN_POINT('Ctrl Pts',(0.169870716593952,-0.0313579730236637,
0.632481855961396));
#42967=CARTESIAN_POINT('Ctrl Pts',(0.118984830409674,0.12522776433633,0.640387879160913));
#42968=CARTESIAN_POINT('Ctrl Pts',(-0.0399963308863663,0.168046649308817,
0.648293902360431));
#42969=CARTESIAN_POINT('Ctrl Pts',(-0.162641646884031,0.0581986041684188,
0.656199925559947));
#42970=CARTESIAN_POINT('Ctrl Pts',(-0.137530366481649,-0.104521677769314,
0.664105948759466));
#42971=CARTESIAN_POINT('Ctrl Pts',(0.0125244277271302,-0.172286161772757,
0.672011971958982));
#42972=CARTESIAN_POINT('Ctrl Pts',(0.151201036531162,-0.0835322056469662,
0.679917995158501));
#42973=CARTESIAN_POINT('Ctrl Pts',(0.152514608511077,0.08110904400223,0.687824018358017));
#42974=CARTESIAN_POINT('Ctrl Pts',(0.015271790498195,0.172064392723197,
0.695730041557536));
#42975=CARTESIAN_POINT('Ctrl Pts',(-0.135845135582574,0.106702773943246,
0.703636064757053));
#42976=CARTESIAN_POINT('Ctrl Pts',(-0.163549545519903,-0.0555961238584937,
0.71154208795657));
#42977=CARTESIAN_POINT('Ctrl Pts',(-0.042672551795764,-0.167387084780248,
0.719448111156087));
#42978=CARTESIAN_POINT('Ctrl Pts',(0.116971578978639,-0.127110316425345,
0.727354134355605));
#42979=CARTESIAN_POINT('Ctrl Pts',(0.170349432203978,0.0286435642436946,
0.735260157555123));
#42980=CARTESIAN_POINT('Ctrl Pts',(0.0689683243827774,0.158375354962157,
0.74316618075464));
#42981=CARTESIAN_POINT('Ctrl Pts',(-0.0950690899731296,0.144226387925758,
0.751072203954158));
#42982=CARTESIAN_POINT('Ctrl Pts',(-0.172738188158534,-0.000949290976420475,
0.758978227153675));
#42983=CARTESIAN_POINT('Ctrl Pts',(-0.0934781897973971,-0.145262558371866,
0.766884250353192));
#42984=CARTESIAN_POINT('Ctrl Pts',(0.0707048249667505,-0.157607774687799,
0.77479027355271));
#42985=CARTESIAN_POINT('Ctrl Pts',(0.170653957167994,-0.026769563590997,
0.782696296752227));
#42986=CARTESIAN_POINT('Ctrl Pts',(0.115567475470849,0.128388245309395,
0.790602319951745));
#42987=CARTESIAN_POINT('Ctrl Pts',(-0.044509688091521,0.166907971684466,
0.798508343151262));
#42988=CARTESIAN_POINT('Ctrl Pts',(-0.164150707289131,0.0537952295263864,
0.806414366350779));
#42989=CARTESIAN_POINT('Ctrl Pts',(-0.134664192471597,-0.108189367037688,
0.814320389550297));
#42990=CARTESIAN_POINT('Ctrl Pts',(0.0171620001843438,-0.171886158484381,
0.822226412749814));
#42991=CARTESIAN_POINT('Ctrl Pts',(0.153396822002609,-0.0794278794991626,
0.830132435949332));
#42992=CARTESIAN_POINT('Ctrl Pts',(0.150273868521174,0.0851889493562029,
0.838038459148849));
#42993=CARTESIAN_POINT('Ctrl Pts',(0.010630025052753,0.17241345751384,0.845944482348367));
#42994=CARTESIAN_POINT('Ctrl Pts',(-0.138670662100443,0.10300370814974,
0.853850505547884));
#42995=CARTESIAN_POINT('Ctrl Pts',(-0.161992500097515,-0.0599824685600915,
0.861756528747401));
#42996=CARTESIAN_POINT('Ctrl Pts',(-0.0381463389702577,-0.16847642418213,
0.869662551946919));
#42997=CARTESIAN_POINT('Ctrl Pts',(0.120352823932529,-0.123911830666367,
0.877568575146436));
#42998=CARTESIAN_POINT('Ctrl Pts',(0.169518027664615,0.0332218802417698,
0.885474598345955));
#42999=CARTESIAN_POINT('Ctrl Pts',(0.064671777881489,0.160178442699814,
0.89338062154547));
#43000=CARTESIAN_POINT('Ctrl Pts',(-0.0989126265492044,0.141608111244184,
0.90128664474499));
#43001=CARTESIAN_POINT('Ctrl Pts',(-0.172665106841263,-0.00559495509920419,
0.909192667944505));
#43002=CARTESIAN_POINT('Ctrl Pts',(-0.0895013604158129,-0.147744249647878,
0.917098691144024));
#43003=CARTESIAN_POINT('Ctrl Pts',(0.0748706596781056,-0.155615430834315,
0.925004714343541));
#43004=CARTESIAN_POINT('Ctrl Pts',(0.171419547512711,-0.0222200229875446,
0.932910737543058));
#43005=CARTESIAN_POINT('Ctrl Pts',(0.111850793266265,0.131576757499091,
0.940816760742576));
#43006=CARTESIAN_POINT('Ctrl Pts',(0.00497016310172783,0.154086330973247,
0.946087442875587));
#43007=CARTESIAN_POINT('Ctrl Pts',(-0.0415060733756141,0.140340900570497,
0.948722783942093));
#43008=CARTESIAN_POINT('Ctrl Pts',(-0.146190615322833,-9.92620605964336E-5,
0.858934495415709));
#43009=CARTESIAN_POINT('Ctrl Pts',(-0.146299982018485,-0.0174419138812775,
0.85987517319294));
#43010=CARTESIAN_POINT('Ctrl Pts',(-0.143444813888727,-0.0347497500736094,
0.860815850970171));
#43011=CARTESIAN_POINT('Ctrl Pts',(-0.13746450024346,-0.0509004317121259,
0.861756528747401));
#43012=CARTESIAN_POINT('Ctrl Pts',(-0.120710446388429,-0.0961471204341042,
0.864391869813907));
#43013=CARTESIAN_POINT('Ctrl Pts',(-0.0794283926793434,-0.132311772308117,
0.867027210880413));
#43014=CARTESIAN_POINT('Ctrl Pts',(-0.032370838674336,-0.142966665992496,
0.869662551946919));
#43015=CARTESIAN_POINT('Ctrl Pts',(0.014686715330672,-0.153621559676876,
0.872297893013425));
#43016=CARTESIAN_POINT('Ctrl Pts',(0.0675197696316001,-0.138766695171622,
0.874933234079931));
#43017=CARTESIAN_POINT('Ctrl Pts',(0.10213049740408,-0.105150311100971,
0.877568575146437));
#43018=CARTESIAN_POINT('Ctrl Pts',(0.136741225176558,-0.0715339270303214,
0.880203916212942));
#43019=CARTESIAN_POINT('Ctrl Pts',(0.153129626420586,-0.019156023394278,
0.882839257279448));
#43020=CARTESIAN_POINT('Ctrl Pts',(0.143849452078747,0.028192355500085,
0.885474598345954));
#43021=CARTESIAN_POINT('Ctrl Pts',(0.134569277736908,0.0755407343944486,
0.88810993941246));
#43022=CARTESIAN_POINT('Ctrl Pts',(0.0996205278091978,0.117859588547133,
0.890745280478965));
#43023=CARTESIAN_POINT('Ctrl Pts',(0.0548820854402278,0.135923960380868,
0.893380621545471));
#43024=CARTESIAN_POINT('Ctrl Pts',(0.0101436430712571,0.153988332214605,
0.896015962611977));
#43025=CARTESIAN_POINT('Ctrl Pts',(-0.0443844917389754,0.147798221729394,
0.898651303678484));
#43026=CARTESIAN_POINT('Ctrl Pts',(-0.0839406391927675,0.120169322096223,
0.901286644744989));
#43027=CARTESIAN_POINT('Ctrl Pts',(-0.0957651970765149,0.111910188080244,
0.902074429829993));
#43028=CARTESIAN_POINT('Ctrl Pts',(-0.106251862209464,0.10173528965009,
0.902862214914997));
#43029=CARTESIAN_POINT('Ctrl Pts',(-0.115101970897794,0.0902398078595192,
0.903650000000001));
#43030=CARTESIAN_POINT('Ctrl Pts',(-0.0686121729278153,-0.0959472995825293,
-5.42101086242752E-19));
#43031=CARTESIAN_POINT('Ctrl Pts',(-0.0716149353959019,-0.0943161956304311,
-1.06730581618305E-18));
#43032=CARTESIAN_POINT('Ctrl Pts',(-0.0745354620527207,-0.0925505885939475,
1.1783117230653E-17));
#43033=CARTESIAN_POINT('Ctrl Pts',(-0.0773634912799965,-0.0906526488910235,
6.72205346941013E-18));
#43034=CARTESIAN_POINT('Ctrl Pts',(-0.0815539383946836,-0.0878403667988651,
-2.29049000805066E-18));
#43035=CARTESIAN_POINT('Ctrl Pts',(-0.0855414709026766,-0.0847378275400617,
-2.5182094749946E-17));
#43036=CARTESIAN_POINT('Ctrl Pts',(-0.089317923041959,-0.0813786482814292,
-3.31765864780564E-17));
#43037=CARTESIAN_POINT('Ctrl Pts',(-0.0927862368571965,-0.0782935601084891,
-4.05187703807701E-17));
#43038=CARTESIAN_POINT('Ctrl Pts',(-0.0960787339139733,-0.0749884873641515,
4.97114916498215E-19));
#43039=CARTESIAN_POINT('Ctrl Pts',(-0.0991698906024268,-0.0715076841230725,
-8.67361737988404E-19));
#43040=CARTESIAN_POINT('Ctrl Pts',(-0.103663297594998,-0.0664478740909087,
-2.85080986385392E-18));
#43041=CARTESIAN_POINT('Ctrl Pts',(-0.107740134647113,-0.0610110581939007,
-1.51788304147971E-17));
#43042=CARTESIAN_POINT('Ctrl Pts',(-0.111378619976329,-0.0552695407791115,
-1.51788304147971E-17));
#43043=CARTESIAN_POINT('Ctrl Pts',(-0.113566215904755,-0.0518175218802795,
-1.51788304147971E-17));
#43044=CARTESIAN_POINT('Ctrl Pts',(-0.115595886809481,-0.0482525855570875,
-3.79982201238933E-17));
#43045=CARTESIAN_POINT('Ctrl Pts',(-0.117451481229743,-0.0446106777439056,
-3.20923843055709E-17));
#43046=CARTESIAN_POINT('Ctrl Pts',(-0.121759272594108,-0.0361559319998316,
-1.83818944163349E-17));
#43047=CARTESIAN_POINT('Ctrl Pts',(-0.125146870804877,-0.027267170883122,
-1.0758832179559E-17));
#43048=CARTESIAN_POINT('Ctrl Pts',(-0.127551512867323,-0.0181239349359946,
-1.21430643318376E-17));
#43049=CARTESIAN_POINT('Ctrl Pts',(-0.128525246808636,-0.0144214798745123,
-1.27035942545157E-17));
#43050=CARTESIAN_POINT('Ctrl Pts',(-0.129337364222068,-0.0106768832185224,
-3.87407706984377E-19));
#43051=CARTESIAN_POINT('Ctrl Pts',(-0.129981634111732,-0.00690081199580598,
2.60208521396521E-18));
#43052=CARTESIAN_POINT('Ctrl Pts',(-0.130488787940845,-0.00392837915310221,
4.95534245334234E-18));
#43053=CARTESIAN_POINT('Ctrl Pts',(-0.130891436982594,-0.000937368841373321,
-5.77147351242312E-18));
#43054=CARTESIAN_POINT('Ctrl Pts',(-0.131185766414779,0.00205408358364406,
-5.20417042793042E-18));
#43055=CARTESIAN_POINT('Ctrl Pts',(-0.131681056523625,0.00708802390756766,
-4.24952717536476E-18));
#43056=CARTESIAN_POINT('Ctrl Pts',(-0.131871567589099,0.0121324651245783,
-2.3640808795201E-17));
#43057=CARTESIAN_POINT('Ctrl Pts',(-0.131747571113314,0.0171617682916428,
-1.73472347597681E-17));
#43058=CARTESIAN_POINT('Ctrl Pts',(-0.131588224313727,0.0236248823338087,
-9.16854279395534E-18));
#43059=CARTESIAN_POINT('Ctrl Pts',(-0.130910003388584,0.0300630957896326,
1.9164721863282E-18));
#43060=CARTESIAN_POINT('Ctrl Pts',(-0.129749448943416,0.0364359420359482,
1.73472347597681E-18));
#43061=CARTESIAN_POINT('Ctrl Pts',(-0.129188162258574,0.039518084159911,
1.64682313529719E-18));
#43062=CARTESIAN_POINT('Ctrl Pts',(-0.128513877700937,0.0425849598402651,
-2.5119873647686E-17));
#43063=CARTESIAN_POINT('Ctrl Pts',(-0.127729776371406,0.0456319959092621,
-2.60208521396521E-17));
#43064=CARTESIAN_POINT('Ctrl Pts',(-0.126905460209866,0.0488353077541379,
-2.69680398361349E-17));
#43065=CARTESIAN_POINT('Ctrl Pts',(-0.125961589290349,0.0520090496451376,
-6.80234412585701E-18));
#43066=CARTESIAN_POINT('Ctrl Pts',(-0.124905367512152,0.0551421622546814,
-8.67361737988404E-18));
#43067=CARTESIAN_POINT('Ctrl Pts',(-0.122242239861443,0.0630419035736882,
-1.33917927173935E-17));
#43068=CARTESIAN_POINT('Ctrl Pts',(-0.118863777535182,0.0706951392673794,
8.60987302363936E-19));
#43069=CARTESIAN_POINT('Ctrl Pts',(-0.114842094503769,0.0780194918792452,
1.73472347597681E-18));
#43070=CARTESIAN_POINT('Ctrl Pts',(-0.112169428435535,0.0828869935059547,
2.31537714896978E-18));
#43071=CARTESIAN_POINT('Ctrl Pts',(-0.109212095329563,0.0876093199712314,
1.58690079118504E-17));
#43072=CARTESIAN_POINT('Ctrl Pts',(-0.105985186696901,0.0921609434032714,
1.90819582357449E-17));
#43073=CARTESIAN_POINT('Ctrl Pts',(-0.104153982707569,0.0947438956760198,
2.09052411731938E-17));
#43074=CARTESIAN_POINT('Ctrl Pts',(-0.102235981964729,0.0972711925776025,
1.37027400976072E-17));
#43075=CARTESIAN_POINT('Ctrl Pts',(-0.10024275281245,0.0997277902811201,
1.21430643318376E-17));
#43076=CARTESIAN_POINT('Ctrl Pts',(-0.0937332858648147,0.107750521403832,
7.04949150570437E-18));
#43077=CARTESIAN_POINT('Ctrl Pts',(-0.0864043214638765,0.115051138974542,
-2.08047340785725E-18));
#43078=CARTESIAN_POINT('Ctrl Pts',(-0.0783638198438572,0.121477900017692,
0.));
#43079=CARTESIAN_POINT('Ctrl Pts',(-0.0736196559743728,0.125269903176152,
1.22754863308587E-18));
#43080=CARTESIAN_POINT('Ctrl Pts',(-0.0686268317545984,0.128757413629593,
6.34938948147863E-19));
#43081=CARTESIAN_POINT('Ctrl Pts',(-0.0634007094575211,0.131904027763685,
0.));
#43082=CARTESIAN_POINT('Origin',(0.,0.,0.));
#43083=CARTESIAN_POINT('Origin',(-0.0577350269189626,-0.1,-0.3));
#43084=CARTESIAN_POINT('',(-0.0577350269189626,-0.1,-0.3));
#43085=CARTESIAN_POINT('',(0.0577350269189626,-0.1,-0.3));
#43086=CARTESIAN_POINT('',(-0.0288675134594813,-0.1,-0.3));
#43087=CARTESIAN_POINT('',(-0.0577350269189626,-0.1,-0.1));
#43088=CARTESIAN_POINT('',(-0.0577350269189626,-0.1,-0.3));
#43089=CARTESIAN_POINT('',(0.0577350269189626,-0.1,-0.1));
#43090=CARTESIAN_POINT('',(-0.0577350269189626,-0.1,-0.1));
#43091=CARTESIAN_POINT('',(0.0577350269189626,-0.1,-0.3));
#43092=CARTESIAN_POINT('Origin',(-0.115470053837925,1.41410031829988E-17,
-0.3));
#43093=CARTESIAN_POINT('',(-0.115470053837925,1.41410031829988E-17,-0.3));
#43094=CARTESIAN_POINT('',(-0.101036297108185,-0.025,-0.3));
#43095=CARTESIAN_POINT('',(-0.115470053837925,1.38777878078145E-17,-0.1));
#43096=CARTESIAN_POINT('',(-0.115470053837925,1.41410031829988E-17,-0.3));
#43097=CARTESIAN_POINT('',(-0.115470053837925,1.41410031829988E-17,-0.1));
#43098=CARTESIAN_POINT('Origin',(-0.0577350269189626,0.1,-0.3));
#43099=CARTESIAN_POINT('',(-0.0577350269189626,0.1,-0.3));
#43100=CARTESIAN_POINT('',(-0.0721687836487032,0.075,-0.3));
#43101=CARTESIAN_POINT('',(-0.0577350269189626,0.1,-0.1));
#43102=CARTESIAN_POINT('',(-0.0577350269189626,0.1,-0.3));
#43103=CARTESIAN_POINT('',(-0.0577350269189626,0.1,-0.1));
#43104=CARTESIAN_POINT('Origin',(0.0577350269189626,0.1,-0.3));
#43105=CARTESIAN_POINT('',(0.0577350269189626,0.1,-0.3));
#43106=CARTESIAN_POINT('',(0.0288675134594813,0.1,-0.3));
#43107=CARTESIAN_POINT('',(0.0577350269189626,0.1,-0.1));
#43108=CARTESIAN_POINT('',(0.0577350269189626,0.1,-0.3));
#43109=CARTESIAN_POINT('',(0.0577350269189626,0.1,-0.1));
#43110=CARTESIAN_POINT('Origin',(0.115470053837925,0.,-0.3));
#43111=CARTESIAN_POINT('',(0.115470053837925,0.,-0.3));
#43112=CARTESIAN_POINT('',(0.101036297108185,0.025,-0.3));
#43113=CARTESIAN_POINT('',(0.115470053837925,0.,-0.1));
#43114=CARTESIAN_POINT('',(0.115470053837925,0.,-0.3));
#43115=CARTESIAN_POINT('',(0.115470053837925,0.,-0.1));
#43116=CARTESIAN_POINT('Origin',(0.0577350269189626,-0.1,-0.3));
#43117=CARTESIAN_POINT('',(0.0721687836487032,-0.075,-0.3));
#43118=CARTESIAN_POINT('',(0.0577350269189626,-0.1,-0.1));
#43119=CARTESIAN_POINT('Origin',(0.,0.,-0.1));
#43120=CARTESIAN_POINT('Origin',(0.,0.,0.));
#43121=CARTESIAN_POINT('',(-0.3,-3.67394039744206E-17,0.));
#43122=CARTESIAN_POINT('Origin',(0.,0.,0.));
#43123=CARTESIAN_POINT('Origin',(0.,0.,-0.3));
#43124=CARTESIAN_POINT('',(-0.3,-3.67394039744206E-17,-0.3));
#43125=CARTESIAN_POINT('',(-0.3,-3.67394039744206E-17,-0.3));
#43126=CARTESIAN_POINT('Origin',(0.,0.,-0.3));
#43127=CARTESIAN_POINT('Origin',(0.,0.,-0.3));
#43128=CARTESIAN_POINT('Origin',(0.,0.,1.));
#43129=CARTESIAN_POINT('',(0.,0.,0.));
#43130=CARTESIAN_POINT('Origin',(0.,0.,0.));
#43131=CARTESIAN_POINT('',(-0.492481417404046,0.000356103300314048,0.0483841525903583));
#43132=CARTESIAN_POINT('',(-0.492579697791124,0.00014242512799704,0.0266158474096417));
#43133=CARTESIAN_POINT('',(-0.4925,-6.03138548580071E-17,0.));
#43134=CARTESIAN_POINT('',(0.216839587231055,0.442195480991683,0.));
#43135=CARTESIAN_POINT('Ctrl Pts',(-0.492481417404046,0.000356103300314048,
0.0483841525903583));
#43136=CARTESIAN_POINT('Ctrl Pts',(-0.492781970042288,0.0365118891852549,
0.0466308494026249));
#43137=CARTESIAN_POINT('Ctrl Pts',(-0.489117551943374,0.0726092955132097,
0.0448775462148916));
#43138=CARTESIAN_POINT('Ctrl Pts',(-0.481251921643029,0.107767962452072,
0.0431242430271582));
#43139=CARTESIAN_POINT('Ctrl Pts',(-0.446686359481315,0.262272946947089,
0.0354193410663739));
#43140=CARTESIAN_POINT('Ctrl Pts',(-0.330988306870102,0.398649291214372,
0.0277144391055896));
#43141=CARTESIAN_POINT('Ctrl Pts',(-0.184035775927903,0.457657279283401,
0.0200095371448053));
#43142=CARTESIAN_POINT('Ctrl Pts',(-0.0568244611321571,0.508738289576891,
0.0133396914298702));
#43143=CARTESIAN_POINT('Ctrl Pts',(0.0938080781422166,0.501841636033798,
0.00666984571493511));
#43144=CARTESIAN_POINT('Ctrl Pts',(0.217447815076511,0.442338803773993,
3.90312782094782E-18));
#43145=CARTESIAN_POINT('',(-0.216839587231055,0.442195480991683,0.));
#43146=CARTESIAN_POINT('Origin',(0.,0.,0.));
#43147=CARTESIAN_POINT('Ctrl Pts',(-0.216839587231054,0.442195480991683,
0.));
#43148=CARTESIAN_POINT('Ctrl Pts',(-0.288701679351503,0.406956436128511,
0.00387968930265135));
#43149=CARTESIAN_POINT('Ctrl Pts',(-0.351338791070612,0.353873869634597,
0.00775937860530267));
#43150=CARTESIAN_POINT('Ctrl Pts',(-0.398480091786207,0.289102201512631,
0.011639067907954));
#43151=CARTESIAN_POINT('Ctrl Pts',(-0.445621392501803,0.224330533390666,
0.0155187572106054));
#43152=CARTESIAN_POINT('Ctrl Pts',(-0.477266882213885,0.147869763640648,
0.0193984465132567));
#43153=CARTESIAN_POINT('Ctrl Pts',(-0.488203763978274,0.068702451394776,
0.0232781358159081));
#43154=CARTESIAN_POINT('Ctrl Pts',(-0.491340111094124,0.0459998038960704,
0.0243907063471526));
#43155=CARTESIAN_POINT('Ctrl Pts',(-0.492773468136237,0.0230745815620001,
0.0255032768783972));
#43156=CARTESIAN_POINT('Ctrl Pts',(-0.492579697791124,0.00014242512799704,
0.0266158474096417));
#43157=CARTESIAN_POINT('Origin',(0.,0.,0.));
#43158=CARTESIAN_POINT('',(-0.492300964172325,-0.000364928074014725,0.198384152590358));
#43159=CARTESIAN_POINT('',(-0.491861190935719,-0.000202060802622812,0.176615847409642));
#43160=CARTESIAN_POINT('',(-0.4925,-6.03138548580071E-17,0.));
#43161=CARTESIAN_POINT('Ctrl Pts',(-0.492300964172325,-0.000364928074014725,
0.198384152590358));
#43162=CARTESIAN_POINT('Ctrl Pts',(-0.491417602280064,0.113686713783483,
0.192860261167331));
#43163=CARTESIAN_POINT('Ctrl Pts',(-0.451685363551956,0.228287340070974,
0.187336369744303));
#43164=CARTESIAN_POINT('Ctrl Pts',(-0.379073885019767,0.315519852460857,
0.181812478321276));
#43165=CARTESIAN_POINT('Ctrl Pts',(-0.2777930522746,0.43719457491378,0.174107576360492));
#43166=CARTESIAN_POINT('Ctrl Pts',(-0.11254378321799,0.505623070834234,
0.166402674399707));
#43167=CARTESIAN_POINT('Ctrl Pts',(0.0451027730094741,0.491145507720989,
0.158697772438923));
#43168=CARTESIAN_POINT('Ctrl Pts',(0.202749329236939,0.476667944607744,
0.150992870478139));
#43169=CARTESIAN_POINT('Ctrl Pts',(0.352793172635258,0.379284322460801,
0.143287968517354));
#43170=CARTESIAN_POINT('Ctrl Pts',(0.430212224753047,0.241196209673131,
0.13558306655657));
#43171=CARTESIAN_POINT('Ctrl Pts',(0.507631276870837,0.103108096885462,
0.127878164595786));
#43172=CARTESIAN_POINT('Ctrl Pts',(0.512425537708097,-0.0756845065429327,
0.120173262635001));
#43173=CARTESIAN_POINT('Ctrl Pts',(0.442539342879764,-0.217735430292011,
0.112468360674217));
#43174=CARTESIAN_POINT('Ctrl Pts',(0.372653148051431,-0.35978635404109,
0.104763458713433));
#43175=CARTESIAN_POINT('Ctrl Pts',(0.228086497557505,-0.465095598110853,
0.0970585567526484));
#43176=CARTESIAN_POINT('Ctrl Pts',(0.0714359265950831,-0.488016791697039,
0.0893536547918641));
#43177=CARTESIAN_POINT('Ctrl Pts',(-0.0852146443673392,-0.510937985283226,
0.0816487528310798));
#43178=CARTESIAN_POINT('Ctrl Pts',(-0.253949135798258,-0.451471128385836,
0.0739438508702954));
#43179=CARTESIAN_POINT('Ctrl Pts',(-0.361599845657609,-0.335420887575765,
0.0662389489095111));
#43180=CARTESIAN_POINT('Ctrl Pts',(-0.444753899528498,-0.245778673523871,
0.0602873501364602));
#43181=CARTESIAN_POINT('Ctrl Pts',(-0.491461189570368,-0.122374940832272,
0.0543357513634092));
#43182=CARTESIAN_POINT('Ctrl Pts',(-0.492481417404046,0.000356103300314048,
0.0483841525903583));
#43183=CARTESIAN_POINT('Ctrl Pts',(-0.492579697791124,0.00014242512799704,
0.0266158474096417));
#43184=CARTESIAN_POINT('Ctrl Pts',(-0.491422059458777,-0.136860702548402,
0.0332626554836999));
#43185=CARTESIAN_POINT('Ctrl Pts',(-0.43218895190202,-0.274111322283754,
0.039909463557758));
#43186=CARTESIAN_POINT('Ctrl Pts',(-0.331056890567679,-0.365627465232998,
0.0465562716318162));
#43187=CARTESIAN_POINT('Ctrl Pts',(-0.212996921890301,-0.472461962893863,
0.0543156502371188));
#43188=CARTESIAN_POINT('Ctrl Pts',(-0.0378376527975418,-0.516970163740431,
0.0620750288424216));
#43189=CARTESIAN_POINT('Ctrl Pts',(0.117082871749507,-0.479203433651414,
0.0698344074477242));
#43190=CARTESIAN_POINT('Ctrl Pts',(0.272003396296556,-0.441436703562397,
0.077593786053027));
#43191=CARTESIAN_POINT('Ctrl Pts',(0.406685176297894,-0.321395042537794,
0.0853531646583296));
#43192=CARTESIAN_POINT('Ctrl Pts',(0.46224191715632,-0.171962621091513,
0.0931125432636324));
#43193=CARTESIAN_POINT('Ctrl Pts',(0.517798658014746,-0.0225301996452326,
0.100871921868935));
#43194=CARTESIAN_POINT('Ctrl Pts',(0.494230359730261,0.156292982222727,
0.108631300474238));
#43195=CARTESIAN_POINT('Ctrl Pts',(0.401766762010813,0.286123680734623,
0.11639067907954));
#43196=CARTESIAN_POINT('Ctrl Pts',(0.309303164291365,0.415954379246519,
0.124150057684843));
#43197=CARTESIAN_POINT('Ctrl Pts',(0.147944267136953,0.496792594402351,
0.131909436290146));
#43198=CARTESIAN_POINT('Ctrl Pts',(-0.0114321433727825,0.493107659430119,
0.139668814895449));
#43199=CARTESIAN_POINT('Ctrl Pts',(-0.170808553882518,0.489422724457888,
0.147428193500751));
#43200=CARTESIAN_POINT('Ctrl Pts',(-0.328202477747577,0.401214639357593,
0.155187572106054));
#43201=CARTESIAN_POINT('Ctrl Pts',(-0.414565342728602,0.267223128123415,
0.162946950711357));
#43202=CARTESIAN_POINT('Ctrl Pts',(-0.465277525582474,0.188543454631027,
0.167503249610785));
#43203=CARTESIAN_POINT('Ctrl Pts',(-0.491498014918926,0.094077536942573,
0.172059548510213));
#43204=CARTESIAN_POINT('Ctrl Pts',(-0.491861190935719,-0.000202060802622812,
0.176615847409642));
#43205=CARTESIAN_POINT('Origin',(0.,0.,-0.277281266907388));
#43206=CARTESIAN_POINT('',(-0.406885497393593,-0.000301612126959839,0.247718733092612));
#43207=CARTESIAN_POINT('',(-0.407643323035318,5.2650356487962E-5,0.277281266907388));
#43208=CARTESIAN_POINT('',(-0.40705,-1.70476957675307E-16,-0.277281266907388));
#43209=CARTESIAN_POINT('',(-0.398956125446125,0.0807695020971151,0.39295));
#43210=CARTESIAN_POINT('Ctrl Pts',(-0.406885497393594,-0.00030161212695989,
0.247718733092612));
#43211=CARTESIAN_POINT('Ctrl Pts',(-0.407173762990612,-0.0375198404872463,
0.249899743630369));
#43212=CARTESIAN_POINT('Ctrl Pts',(-0.385791970676486,-0.205899073274862,
0.25978565612891));
#43213=CARTESIAN_POINT('Ctrl Pts',(-0.153651115557833,-0.451003868944285,
0.277376470588235));
#43214=CARTESIAN_POINT('Ctrl Pts',(0.284312994089833,-0.382152940416395,
0.300491176470589));
#43215=CARTESIAN_POINT('Ctrl Pts',(0.476331647790245,0.0175545413646465,
0.323605882352941));
#43216=CARTESIAN_POINT('Ctrl Pts',(0.254819026846725,0.402583723993036,
0.346720588235294));
#43217=CARTESIAN_POINT('Ctrl Pts',(-0.112351263190869,0.431821186557985,
0.365982843137255));
#43218=CARTESIAN_POINT('Ctrl Pts',(-0.327918115217093,0.266750651701983,
0.381392647058824));
#43219=CARTESIAN_POINT('Ctrl Pts',(-0.385922262909618,0.145149486647597,
0.389097549019608));
#43220=CARTESIAN_POINT('Ctrl Pts',(-0.398956125446125,0.0807695020971137,
0.39295));
#43221=CARTESIAN_POINT('',(-0.0538698874795526,0.403469624287802,0.39295));
#43222=CARTESIAN_POINT('Origin',(0.,0.,0.39295));
#43223=CARTESIAN_POINT('Ctrl Pts',(-0.407643323035318,5.26503564879819E-5,
0.277281266907388));
#43224=CARTESIAN_POINT('Ctrl Pts',(-0.407328549577932,-0.127609068365495,
0.284799996850381));
#43225=CARTESIAN_POINT('Ctrl Pts',(-0.275150626354469,-0.387484704349645,
0.300078105398677));
#43226=CARTESIAN_POINT('Ctrl Pts',(0.163268921903001,-0.448972926511222,
0.323115592552276));
#43227=CARTESIAN_POINT('Ctrl Pts',(0.463203848138002,-0.116047052095292,
0.346393728368184));
#43228=CARTESIAN_POINT('Ctrl Pts',(0.373893623429547,0.244589772389548,
0.365792174881441));
#43229=CARTESIAN_POINT('Ctrl Pts',(0.146530577079214,0.396735441137677,
0.381310932092046));
#43230=CARTESIAN_POINT('Ctrl Pts',(0.0116987864547665,0.412224129892184,
0.389070310697349));
#43231=CARTESIAN_POINT('Ctrl Pts',(-0.0538698874795526,0.403469624287802,
0.39295));
#43232=CARTESIAN_POINT('Origin',(0.,0.,-0.277281266907388));
#43233=CARTESIAN_POINT('',(-0.407034641531608,0.00029431847389476,0.0977187330926118));
#43234=CARTESIAN_POINT('',(-0.406522025929715,-0.00016700274052156,0.127281266907388));
#43235=CARTESIAN_POINT('',(-0.40705,-1.70476957675307E-16,-0.277281266907388));
#43236=CARTESIAN_POINT('Ctrl Pts',(-0.407034641531608,0.000294318473894748,
0.0977187330926118));
#43237=CARTESIAN_POINT('Ctrl Pts',(-0.406191425816484,-0.101142578001576,
0.103670331865663));
#43238=CARTESIAN_POINT('Ctrl Pts',(-0.317612179383904,-0.335174773810633,
0.117326832599498));
#43239=CARTESIAN_POINT('Ctrl Pts',(0.0690289416187412,-0.471438154334252,
0.138688235294118));
#43240=CARTESIAN_POINT('Ctrl Pts',(0.427480850757132,-0.210324685510313,
0.161802941176471));
#43241=CARTESIAN_POINT('Ctrl Pts',(0.41559351751567,0.232990213325393,0.184917647058823));
#43242=CARTESIAN_POINT('Ctrl Pts',(0.0435609502753498,0.474452162939076,
0.208032352941177));
#43243=CARTESIAN_POINT('Ctrl Pts',(-0.32751247561348,0.320793411196436,
0.228966048285772));
#43244=CARTESIAN_POINT('Ctrl Pts',(-0.406155401031675,0.09396178039709,
0.242194841669584));
#43245=CARTESIAN_POINT('Ctrl Pts',(-0.406885497393594,-0.00030161212695989,
0.247718733092612));
#43246=CARTESIAN_POINT('Ctrl Pts',(-0.406522025929715,-0.000167002740521567,
0.127281266907388));
#43247=CARTESIAN_POINT('Ctrl Pts',(-0.406733041365224,-0.0549460890728457,
0.130484346613262));
#43248=CARTESIAN_POINT('Ctrl Pts',(-0.371307907491832,-0.242165643317298,
0.141446804924439));
#43249=CARTESIAN_POINT('Ctrl Pts',(-0.0916847062669661,-0.468629856473293,
0.160168641840919));
#43250=CARTESIAN_POINT('Ctrl Pts',(0.336453410254844,-0.338849716643417,
0.183446777656827));
#43251=CARTESIAN_POINT('Ctrl Pts',(0.46926975494663,0.088378354603048,0.206724913472736));
#43252=CARTESIAN_POINT('Ctrl Pts',(0.190156376929569,0.437998801366229,
0.230003049288643));
#43253=CARTESIAN_POINT('Ctrl Pts',(-0.255854007963939,0.403215004461254,
0.253281185104552));
#43254=CARTESIAN_POINT('Ctrl Pts',(-0.405783805870032,0.139964592457054,
0.269040590977466));
#43255=CARTESIAN_POINT('Ctrl Pts',(-0.407653397850083,0.0041386624983676,
0.277040618245079));
#43256=CARTESIAN_POINT('Ctrl Pts',(-0.407643323035318,5.26503564879819E-5,
0.277281266907388));
#43257=CARTESIAN_POINT('Origin',(0.,0.,0.35));
#43258=CARTESIAN_POINT('',(-0.481004250423532,5.53027357347368E-5,0.319618961639866));
#43259=CARTESIAN_POINT('Ctrl Pts',(-0.0538698874795498,0.403469624287803,
0.39295));
#43260=CARTESIAN_POINT('Ctrl Pts',(-0.0316653326884239,0.407278826215671,
0.392112902831245));
#43261=CARTESIAN_POINT('Ctrl Pts',(-0.00924491338711062,0.409176650041635,
0.391280875609609));
#43262=CARTESIAN_POINT('Ctrl Pts',(0.0131866458412135,0.409236810812678,
0.390451027642853));
#43263=CARTESIAN_POINT('Ctrl Pts',(0.0268208116764566,0.409273377237724,
0.389946636277027));
#43264=CARTESIAN_POINT('Ctrl Pts',(0.040459458237955,0.408630029143461,
0.389443050004563));
#43265=CARTESIAN_POINT('Ctrl Pts',(0.0540577419912376,0.407314101233933,
0.388939619729085));
#43266=CARTESIAN_POINT('Ctrl Pts',(0.0622889918244366,0.406517549876253,
0.388634885657769));
#43267=CARTESIAN_POINT('Ctrl Pts',(0.0705093035012178,0.405473504159666,
0.388330064318474));
#43268=CARTESIAN_POINT('Ctrl Pts',(0.0786814053095045,0.404187608479032,
0.388026026559159));
#43269=CARTESIAN_POINT('Ctrl Pts',(0.100768052332083,0.40071223278349,0.38720430714975));
#43270=CARTESIAN_POINT('Ctrl Pts',(0.122540335589337,0.395471779259362,
0.386386924436749));
#43271=CARTESIAN_POINT('Ctrl Pts',(0.143803418736277,0.388506736509305,
0.38557112662273));
#43272=CARTESIAN_POINT('Ctrl Pts',(0.156170109258924,0.384455840993744,
0.3850966554924));
#43273=CARTESIAN_POINT('Ctrl Pts',(0.168364571979357,0.379820676364071,
0.384622720474772));
#43274=CARTESIAN_POINT('Ctrl Pts',(0.180342700215435,0.374619772055251,
0.38414878019481));
#43275=CARTESIAN_POINT('Ctrl Pts',(0.186280745973306,0.372041472077208,
0.383913828705442));
#43276=CARTESIAN_POINT('Ctrl Pts',(0.192158160674688,0.369327168271282,
0.38367916801279));
#43277=CARTESIAN_POINT('Ctrl Pts',(0.197963597616422,0.366483083438636,
0.38344498715594));
#43278=CARTESIAN_POINT('Ctrl Pts',(0.219836146361836,0.355767717004984,
0.382562687983959));
#43279=CARTESIAN_POINT('Ctrl Pts',(0.240716970738482,0.343202582426593,
0.381686072170868));
#43280=CARTESIAN_POINT('Ctrl Pts',(0.260332898611107,0.328932743376239,
0.380811747318508));
#43281=CARTESIAN_POINT('Ctrl Pts',(0.278594803461462,0.315647904409681,
0.379997774236746));
#43282=CARTESIAN_POINT('Ctrl Pts',(0.295761578458153,0.300884440199882,
0.379185786756448));
#43283=CARTESIAN_POINT('Ctrl Pts',(0.311586138874096,0.284716704150859,
0.378373047602317));
#43284=CARTESIAN_POINT('Ctrl Pts',(0.312759445782441,0.283517952596312,
0.378312787320883));
#43285=CARTESIAN_POINT('Ctrl Pts',(0.313925356487753,0.282311464687701,
0.378252522907174));
#43286=CARTESIAN_POINT('Ctrl Pts',(0.315083761312798,0.281097263038206,
0.378192253245459));
#43287=CARTESIAN_POINT('Ctrl Pts',(0.318831185432892,0.27716933693707,0.377997281695672));
#43288=CARTESIAN_POINT('Ctrl Pts',(0.322493195092308,0.273167891631071,
0.377802612506538));
#43289=CARTESIAN_POINT('Ctrl Pts',(0.326069508835965,0.269096914837346,
0.377608226014736));
#43290=CARTESIAN_POINT('Ctrl Pts',(0.341206374273448,0.251866371785855,
0.376785478800656));
#43291=CARTESIAN_POINT('Ctrl Pts',(0.354812779827501,0.233391506862419,
0.375967697324452));
#43292=CARTESIAN_POINT('Ctrl Pts',(0.366870039940409,0.213921252206375,
0.375152133928824));
#43293=CARTESIAN_POINT('Ctrl Pts',(0.376130504932898,0.198967306621001,
0.374525748149332));
#43294=CARTESIAN_POINT('Ctrl Pts',(0.384476533461525,0.183425031595393,
0.373900670785239));
#43295=CARTESIAN_POINT('Ctrl Pts',(0.391884013928886,0.167394361930957,
0.373275656992184));
#43296=CARTESIAN_POINT('Ctrl Pts',(0.395222611144067,0.160169240064625,
0.372993959413886));
#43297=CARTESIAN_POINT('Ctrl Pts',(0.398370359701117,0.152844794166232,
0.372712274749158));
#43298=CARTESIAN_POINT('Ctrl Pts',(0.401324042121161,0.145429744486488,
0.372430489026677));
#43299=CARTESIAN_POINT('Ctrl Pts',(0.403162482847082,0.140814444878291,
0.372255099030556));
#43300=CARTESIAN_POINT('Ctrl Pts',(0.404925063262203,0.136165420236397,
0.37207972382087));
#43301=CARTESIAN_POINT('Ctrl Pts',(0.406608059344916,0.131493954632065,
0.371904674370206));
#43302=CARTESIAN_POINT('Ctrl Pts',(0.414696192879373,0.10904385032253,0.371063422660446));
#43303=CARTESIAN_POINT('Ctrl Pts',(0.420972938099192,0.0860210152190577,
0.370227536000813));
#43304=CARTESIAN_POINT('Ctrl Pts',(0.425395909977663,0.0626759796342939,
0.369394086287783));
#43305=CARTESIAN_POINT('Ctrl Pts',(0.429018549770037,0.0435552035616685,
0.368711448419326));
#43306=CARTESIAN_POINT('Ctrl Pts',(0.431396924655892,0.0242172462070704,
0.368030445363422));
#43307=CARTESIAN_POINT('Ctrl Pts',(0.432482965195409,0.00479181875932576,
0.367349468256));
#43308=CARTESIAN_POINT('Ctrl Pts',(0.432895970962219,-0.00259539494657891,
0.367090502349851));
#43309=CARTESIAN_POINT('Ctrl Pts',(0.433121836997117,-0.00999528408518393,
0.3668315401963));
#43310=CARTESIAN_POINT('Ctrl Pts',(0.433156980509427,-0.0174007138892953,
0.366572493314436));
#43311=CARTESIAN_POINT('Ctrl Pts',(0.433183158031874,-0.0229168331438603,
0.366379535777779));
#43312=CARTESIAN_POINT('Ctrl Pts',(0.433103335387378,-0.0284349632594622,
0.366186568266144));
#43313=CARTESIAN_POINT('Ctrl Pts',(0.432916876988951,-0.0339394879965735,
0.36599399665361));
#43314=CARTESIAN_POINT('Ctrl Pts',(0.43208645521872,-0.0584547536806542,
0.365136348723961));
#43315=CARTESIAN_POINT('Ctrl Pts',(0.429146442859694,-0.0827663174634086,
0.36428421955312));
#43316=CARTESIAN_POINT('Ctrl Pts',(0.424019958835254,-0.106615431423388,
0.363434506490917));
#43317=CARTESIAN_POINT('Ctrl Pts',(0.420254969930063,-0.12413068145243,
0.362810460802579));
#43318=CARTESIAN_POINT('Ctrl Pts',(0.415309486405733,-0.141396959340888,
0.362187718294952));
#43319=CARTESIAN_POINT('Ctrl Pts',(0.409263192987451,-0.158338140935025,
0.361565049930666));
#43320=CARTESIAN_POINT('Ctrl Pts',(0.406160149386259,-0.167032595786217,
0.361245487688182));
#43321=CARTESIAN_POINT('Ctrl Pts',(0.402766875155836,-0.175641358171848,
0.360925944974225));
#43322=CARTESIAN_POINT('Ctrl Pts',(0.399092466924463,-0.184153510043428,
0.360606255653821));
#43323=CARTESIAN_POINT('Ctrl Pts',(0.396937681309731,-0.189145296815156,
0.360418780037228));
#43324=CARTESIAN_POINT('Ctrl Pts',(0.394687827641809,-0.194099817084966,
0.36023140397824));
#43325=CARTESIAN_POINT('Ctrl Pts',(0.392348729830297,-0.199007875093207,
0.360044367857094));
#43326=CARTESIAN_POINT('Ctrl Pts',(0.382074069665097,-0.220566882954087,
0.359222797859493));
#43327=CARTESIAN_POINT('Ctrl Pts',(0.370063481928657,-0.241272797950768,
0.358406199055954));
#43328=CARTESIAN_POINT('Ctrl Pts',(0.356513827665842,-0.260956061324833,
0.357591842535157));
#43329=CARTESIAN_POINT('Ctrl Pts',(0.344051171209901,-0.279060268606045,
0.356842816371501));
#43330=CARTESIAN_POINT('Ctrl Pts',(0.33028533438652,-0.29629992463707,0.35609568715483));
#43331=CARTESIAN_POINT('Ctrl Pts',(0.315336322124332,-0.312526310576975,
0.355348331461484));
#43332=CARTESIAN_POINT('Ctrl Pts',(0.310609992907685,-0.317656498485265,
0.355112045010799));
#43333=CARTESIAN_POINT('Ctrl Pts',(0.30576519313948,-0.322685232420505,
0.354875735921677));
#43334=CARTESIAN_POINT('Ctrl Pts',(0.300805202572924,-0.327607284714727,
0.354639337086618));
#43335=CARTESIAN_POINT('Ctrl Pts',(0.296833059963398,-0.331549044962422,
0.354450020217366));
#43336=CARTESIAN_POINT('Ctrl Pts',(0.292793666699487,-0.335415776601772,
0.354260962157573));
#43337=CARTESIAN_POINT('Ctrl Pts',(0.288690374812154,-0.339204472629103,
0.354072175529782));
#43338=CARTESIAN_POINT('Ctrl Pts',(0.270614704216604,-0.355894297105914,
0.353240539616353));
#43339=CARTESIAN_POINT('Ctrl Pts',(0.251296156517944,-0.371078438036047,
0.352413878354462));
#43340=CARTESIAN_POINT('Ctrl Pts',(0.230912254648246,-0.38456380919539,
0.351589358773348));
#43341=CARTESIAN_POINT('Ctrl Pts',(0.218893580948008,-0.392514999145518,
0.351103208875834));
#43342=CARTESIAN_POINT('Ctrl Pts',(0.206503719012034,-0.399875069206143,
0.350617803527155));
#43343=CARTESIAN_POINT('Ctrl Pts',(0.193773466861638,-0.406597848773312,
0.350132562030064));
#43344=CARTESIAN_POINT('Ctrl Pts',(0.185999255133483,-0.41070336931913,
0.349836230889636));
#43345=CARTESIAN_POINT('Ctrl Pts',(0.178098026299929,-0.414571112773857,
0.349539960855983));
#43346=CARTESIAN_POINT('Ctrl Pts',(0.170076244645801,-0.418189396436464,
0.349243619675404));
#43347=CARTESIAN_POINT('Ctrl Pts',(0.164962379018466,-0.420496043170314,
0.349054702918171));
#43348=CARTESIAN_POINT('Ctrl Pts',(0.159797829707925,-0.422701963634567,
0.348865696264321));
#43349=CARTESIAN_POINT('Ctrl Pts',(0.154589564749718,-0.424801769371719,
0.348676759736376));
#43350=CARTESIAN_POINT('Ctrl Pts',(0.132490547639595,-0.433711385776723,
0.347875089391783));
#43351=CARTESIAN_POINT('Ctrl Pts',(0.109712996458169,-0.440673017272614,
0.347078510447043));
#43352=CARTESIAN_POINT('Ctrl Pts',(0.0865025359672138,-0.445776648784633,
0.346284504867115));
#43353=CARTESIAN_POINT('Ctrl Pts',(0.0656695337547962,-0.450357512943821,
0.345571829648553));
#43354=CARTESIAN_POINT('Ctrl Pts',(0.044486654916784,-0.453440828959329,
0.344861227612633));
#43355=CARTESIAN_POINT('Ctrl Pts',(0.0231186212993554,-0.455059571778107,
0.344150877943281));
#43356=CARTESIAN_POINT('Ctrl Pts',(0.0130564925833783,-0.45582183183873,
0.343816376887435));
#43357=CARTESIAN_POINT('Ctrl Pts',(0.00295320522441201,-0.456258902299385,
0.343481931792199));
#43358=CARTESIAN_POINT('Ctrl Pts',(-0.00717423696244157,-0.456371949816793,
0.343147352531355));
#43359=CARTESIAN_POINT('Ctrl Pts',(-0.0143387859440224,-0.456451924055182,
0.342910658067115));
#43360=CARTESIAN_POINT('Ctrl Pts',(-0.0215180448808933,-0.456369369939335,
0.342673810145585));
#43361=CARTESIAN_POINT('Ctrl Pts',(-0.0286817505223104,-0.456125823134922,
0.342437538775626));
#43362=CARTESIAN_POINT('Ctrl Pts',(-0.0537451739868064,-0.455273733867443,
0.341610903833569));
#43363=CARTESIAN_POINT('Ctrl Pts',(-0.0786793252660694,-0.452457377108644,
0.340789283404409));
#43364=CARTESIAN_POINT('Ctrl Pts',(-0.10322605317072,-0.447736883397827,
0.339969902788797));
#43365=CARTESIAN_POINT('Ctrl Pts',(-0.123810173907499,-0.443778424540985,
0.339282795750064));
#43366=CARTESIAN_POINT('Ctrl Pts',(-0.144122638314188,-0.43848000679386,
0.338597263743002));
#43367=CARTESIAN_POINT('Ctrl Pts',(-0.164009324183141,-0.431848940441746,
0.337911670583885));
#43368=CARTESIAN_POINT('Ctrl Pts',(-0.173238698931143,-0.428771474606271,
0.337593488045484));
#43369=CARTESIAN_POINT('Ctrl Pts',(-0.182376275359539,-0.425406617445509,
0.337275292335719));
#43370=CARTESIAN_POINT('Ctrl Pts',(-0.191405887931006,-0.421753266829663,
0.3369569199004));
#43371=CARTESIAN_POINT('Ctrl Pts',(-0.196618434355552,-0.419644288228475,
0.336773132269838));
#43372=CARTESIAN_POINT('Ctrl Pts',(-0.201785860418484,-0.417442838008913,
0.336589607391786));
#43373=CARTESIAN_POINT('Ctrl Pts',(-0.206905131052897,-0.415149652617678,
0.336406322902213));
#43374=CARTESIAN_POINT('Ctrl Pts',(-0.230173294793032,-0.404726641806129,
0.335573256276322));
#43375=CARTESIAN_POINT('Ctrl Pts',(-0.252449394294505,-0.392412097418436,
0.334745101295834));
#43376=CARTESIAN_POINT('Ctrl Pts',(-0.273462988147765,-0.378233667265445,
0.333919012981835));
#43377=CARTESIAN_POINT('Ctrl Pts',(-0.288822939436902,-0.367869899980937,
0.333315181178852));
#43378=CARTESIAN_POINT('Ctrl Pts',(-0.303508291533758,-0.356509065180283,
0.332712453580099));
#43379=CARTESIAN_POINT('Ctrl Pts',(-0.317480036993706,-0.344248782374799,
0.332109719099858));
#43380=CARTESIAN_POINT('Ctrl Pts',(-0.32442200017635,-0.338157171839205,
0.331810246096808));
#43381=CARTESIAN_POINT('Ctrl Pts',(-0.331187642820478,-0.331843302499605,
0.331510771394944));
#43382=CARTESIAN_POINT('Ctrl Pts',(-0.337771160258578,-0.325318048159448,
0.331211158711015));
#43383=CARTESIAN_POINT('Ctrl Pts',(-0.34183643772567,-0.321288747761068,
0.331026149906181));
#43384=CARTESIAN_POINT('Ctrl Pts',(-0.345831067083111,-0.317179806234212,
0.330841137997783));
#43385=CARTESIAN_POINT('Ctrl Pts',(-0.349745720442196,-0.313002903467174,
0.330656479407013));
#43386=CARTESIAN_POINT('Ctrl Pts',(-0.366864224643312,-0.294737601023669,
0.329848980358718));
#43387=CARTESIAN_POINT('Ctrl Pts',(-0.382500655113849,-0.275132445206135,
0.329046214584533));
#43388=CARTESIAN_POINT('Ctrl Pts',(-0.396573125796599,-0.254434970524844,
0.328245596979643));
#43389=CARTESIAN_POINT('Ctrl Pts',(-0.40930334920357,-0.235711643072761,
0.327521343136549));
#43390=CARTESIAN_POINT('Ctrl Pts',(-0.420753757249109,-0.216093166297332,
0.326798847216462));
#43391=CARTESIAN_POINT('Ctrl Pts',(-0.430837734643622,-0.19573929488211,
0.326076195513572));
#43392=CARTESIAN_POINT('Ctrl Pts',(-0.434459892094156,-0.188428198862203,
0.325816619539989));
#43393=CARTESIAN_POINT('Ctrl Pts',(-0.437905483329181,-0.181022066702969,
0.325557023466667));
#43394=CARTESIAN_POINT('Ctrl Pts',(-0.441169547255124,-0.173527888906457,
0.325297318602195));
#43395=CARTESIAN_POINT('Ctrl Pts',(-0.443252573854766,-0.168745331932464,
0.325131582834445));
#43396=CARTESIAN_POINT('Ctrl Pts',(-0.445260942161103,-0.163928315057075,
0.324965852626416));
#43397=CARTESIAN_POINT('Ctrl Pts',(-0.447190162062795,-0.159087569551048,
0.324800404574383));
#43398=CARTESIAN_POINT('Ctrl Pts',(-0.456742756959829,-0.135118461219655,
0.323981183180187));
#43399=CARTESIAN_POINT('Ctrl Pts',(-0.464384303051498,-0.110511230558558,
0.323166844164823));
#43400=CARTESIAN_POINT('Ctrl Pts',(-0.470005652087834,-0.0855055059985193,
0.322354690199387));
#43401=CARTESIAN_POINT('Ctrl Pts',(-0.475490118350773,-0.0611086838401096,
0.321562312605512));
#43402=CARTESIAN_POINT('Ctrl Pts',(-0.479052081018164,-0.0363312413003476,
0.320772014942982));
#43403=CARTESIAN_POINT('Ctrl Pts',(-0.480543654488575,-0.0113809312581294,
0.319981292167799));
#43404=CARTESIAN_POINT('Ctrl Pts',(-0.480771456586696,-0.0075703693990342,
0.319860528215642));
#43405=CARTESIAN_POINT('Ctrl Pts',(-0.480950867488915,-0.0037557678692382,
0.31973975434763));
#43406=CARTESIAN_POINT('Ctrl Pts',(-0.481081249970215,6.21355392569225E-5,
0.319618961639866));
#43407=CARTESIAN_POINT('',(0.0697955034108395,0.486863953835044,0.3075));
#43408=CARTESIAN_POINT('Ctrl Pts',(0.0698314663893227,0.486747372427084,
0.3075));
#43409=CARTESIAN_POINT('Ctrl Pts',(0.0442470650552309,0.487370644859313,
0.310410073119928));
#43410=CARTESIAN_POINT('Ctrl Pts',(0.018704409302911,0.48608015899137,0.313334011041929));
#43411=CARTESIAN_POINT('Ctrl Pts',(-0.00656009088084865,0.482874809315394,
0.316282658377337));
#43412=CARTESIAN_POINT('Ctrl Pts',(-0.0255467494552765,0.480465939974351,
0.318498611980479));
#43413=CARTESIAN_POINT('Ctrl Pts',(-0.0443764046829174,0.476974515955641,
0.320728520848864));
#43414=CARTESIAN_POINT('Ctrl Pts',(-0.0629406504805546,0.472382319692998,
0.322976987839482));
#43415=CARTESIAN_POINT('Ctrl Pts',(-0.0730547215737834,0.469880424384095,
0.324201985355771));
#43416=CARTESIAN_POINT('Ctrl Pts',(-0.0830898537740494,0.467051537608078,
0.325432491347468));
#43417=CARTESIAN_POINT('Ctrl Pts',(-0.0930270499457564,0.463890934176298,
0.326669250158342));
#43418=CARTESIAN_POINT('Ctrl Pts',(-0.0990188180630417,0.461985205181247,
0.327414970770446));
#43419=CARTESIAN_POINT('Ctrl Pts',(-0.104975897972382,0.459958313281541,
0.328163094796111));
#43420=CARTESIAN_POINT('Ctrl Pts',(-0.110878233577805,0.457815290850395,
0.328911766032642));
#43421=CARTESIAN_POINT('Ctrl Pts',(-0.133573530023649,0.449575073313414,
0.331790510446621));
#43422=CARTESIAN_POINT('Ctrl Pts',(-0.155517947173888,0.439604362330888,
0.334684288072021));
#43423=CARTESIAN_POINT('Ctrl Pts',(-0.176494052666361,0.427876171853613,
0.337603770956938));
#43424=CARTESIAN_POINT('Ctrl Pts',(-0.178064691351246,0.426997994077767,
0.337822374584792));
#43425=CARTESIAN_POINT('Ctrl Pts',(-0.179629886094255,0.426109943451997,
0.338041122332846));
#43426=CARTESIAN_POINT('Ctrl Pts',(-0.181189537858252,0.425211999409135,
0.338260018681348));
#43427=CARTESIAN_POINT('Ctrl Pts',(-0.196947491648197,0.416139614752499,
0.340471639649637));
#43428=CARTESIAN_POINT('Ctrl Pts',(-0.212140744926486,0.406057980777516,
0.34269842988097));
#43429=CARTESIAN_POINT('Ctrl Pts',(-0.226690439368773,0.395046192060306,
0.34494501019069));
#43430=CARTESIAN_POINT('Ctrl Pts',(-0.233632026251567,0.389792522409806,
0.346016842487303));
#43431=CARTESIAN_POINT('Ctrl Pts',(-0.240426924417161,0.384327011933825,
0.347093179394951));
#43432=CARTESIAN_POINT('Ctrl Pts',(-0.247065363968451,0.378657760718284,
0.348174522716671));
#43433=CARTESIAN_POINT('Ctrl Pts',(-0.252478394053154,0.374035013587674,
0.349056257631501));
#43434=CARTESIAN_POINT('Ctrl Pts',(-0.257789430726446,0.369274532028075,
0.349941703414435));
#43435=CARTESIAN_POINT('Ctrl Pts',(-0.262975387221713,0.364397963208855,
0.350828068454723));
#43436=CARTESIAN_POINT('Ctrl Pts',(-0.280204713927883,0.348196516577331,
0.353772843034685));
#43437=CARTESIAN_POINT('Ctrl Pts',(-0.296100249356768,0.330680913403001,
0.356734624194827));
#43438=CARTESIAN_POINT('Ctrl Pts',(-0.310500746304381,0.312039737428418,
0.359725026866486));
#43439=CARTESIAN_POINT('Ctrl Pts',(-0.319875678890449,0.299904061227625,
0.361671822421804));
#43440=CARTESIAN_POINT('Ctrl Pts',(-0.328616148097658,0.287290689006832,
0.363630748343365));
#43441=CARTESIAN_POINT('Ctrl Pts',(-0.33666630465908,0.274247977633762,
0.365605009340675));
#43442=CARTESIAN_POINT('Ctrl Pts',(-0.342961754433943,0.264048209001847,
0.367148937195519));
#43443=CARTESIAN_POINT('Ctrl Pts',(-0.3488348232303,0.253585792876292,0.368702243494569));
#43444=CARTESIAN_POINT('Ctrl Pts',(-0.354267090617469,0.242885040692727,
0.370266460933668));
#43445=CARTESIAN_POINT('Ctrl Pts',(-0.356941497389496,0.237616860379455,
0.371036554416534));
#43446=CARTESIAN_POINT('Ctrl Pts',(-0.359509312395157,0.2322898014544,0.37180944552389));
#43447=CARTESIAN_POINT('Ctrl Pts',(-0.361961446378714,0.226922541435087,
0.372583073900236));
#43448=CARTESIAN_POINT('Ctrl Pts',(-0.37140492256759,0.20625254846906,0.375562414017882));
#43449=CARTESIAN_POINT('Ctrl Pts',(-0.379164540226144,0.184934471292981,
0.378560389293445));
#43450=CARTESIAN_POINT('Ctrl Pts',(-0.385152715128125,0.163143884177883,
0.381589261171817));
#43451=CARTESIAN_POINT('Ctrl Pts',(-0.390990790306795,0.141899500396909,
0.384542211281314));
#43452=CARTESIAN_POINT('Ctrl Pts',(-0.395145084054741,0.120204809722708,
0.387524528496279));
#43453=CARTESIAN_POINT('Ctrl Pts',(-0.397485650378386,0.098227288615696,
0.390547575143355));
#43454=CARTESIAN_POINT('Ctrl Pts',(-0.39810341816627,0.0924265537848513,
0.391345476412364));
#43455=CARTESIAN_POINT('Ctrl Pts',(-0.398594566690346,0.0866061945215394,
0.392146215057885));
#43456=CARTESIAN_POINT('Ctrl Pts',(-0.398956125446125,0.0807695020971151,
0.39295));
#43457=CARTESIAN_POINT('',(-0.342664481608845,0.353895656000097,0.3075));
#43458=CARTESIAN_POINT('Origin',(0.,0.,0.3075));
#43459=CARTESIAN_POINT('Ctrl Pts',(-0.481081249970215,6.21355392569225E-5,
0.319618961639866));
#43460=CARTESIAN_POINT('Ctrl Pts',(-0.481245905746716,0.00488364103652631,
0.319466416475099));
#43461=CARTESIAN_POINT('Ctrl Pts',(-0.481332358526736,0.00971269744067388,
0.319313769100939));
#43462=CARTESIAN_POINT('Ctrl Pts',(-0.481339290728969,0.0145394320803265,
0.319161266227293));
#43463=CARTESIAN_POINT('Ctrl Pts',(-0.481374927233973,0.0393523194386921,
0.318377291779119));
#43464=CARTESIAN_POINT('Ctrl Pts',(-0.479315765619102,0.0640754382249796,
0.317598006650885));
#43465=CARTESIAN_POINT('Ctrl Pts',(-0.475334185366473,0.0885133909011413,
0.316821056278798));
#43466=CARTESIAN_POINT('Ctrl Pts',(-0.471321611003206,0.113141577745898,
0.316038057834271));
#43467=CARTESIAN_POINT('Ctrl Pts',(-0.465356080254756,0.137481253645947,
0.315257430636602));
#43468=CARTESIAN_POINT('Ctrl Pts',(-0.457563909950549,0.161331853653742,
0.314476764706437));
#43469=CARTESIAN_POINT('Ctrl Pts',(-0.454530796981434,0.170615732391066,
0.314172889423314));
#43470=CARTESIAN_POINT('Ctrl Pts',(-0.45122042339318,0.179825411865552,
0.313869008271574));
#43471=CARTESIAN_POINT('Ctrl Pts',(-0.447638452480909,0.188948473220082,
0.313564979115321));
#43472=CARTESIAN_POINT('Ctrl Pts',(-0.445471137905168,0.194468491202731,
0.313381022618203));
#43473=CARTESIAN_POINT('Ctrl Pts',(-0.443204366528429,0.199956368985501,
0.313197024052677));
#43474=CARTESIAN_POINT('Ctrl Pts',(-0.440845177239491,0.20539685797324,
0.31301337682937));
#43475=CARTESIAN_POINT('Ctrl Pts',(-0.430431121133819,0.229412547526533,
0.312202711701251));
#43476=CARTESIAN_POINT('Ctrl Pts',(-0.418196042282852,0.252569544019692,
0.311396773420503));
#43477=CARTESIAN_POINT('Ctrl Pts',(-0.404292000940336,0.274648614567846,
0.310592949274326));
#43478=CARTESIAN_POINT('Ctrl Pts',(-0.390460558173166,0.296612401434999,
0.309793322216349));
#43479=CARTESIAN_POINT('Ctrl Pts',(-0.374976844053069,0.317510780436166,
0.308995787273091));
#43480=CARTESIAN_POINT('Ctrl Pts',(-0.357945478548728,0.337105770246179,
0.308197772444498));
#43481=CARTESIAN_POINT('Ctrl Pts',(-0.352982808855556,0.342815439388291,
0.307965243584522));
#43482=CARTESIAN_POINT('Ctrl Pts',(-0.347888479690135,0.34841423125597,
0.307732673980019));
#43483=CARTESIAN_POINT('Ctrl Pts',(-0.342664481608845,0.353895656000097,
0.3075));
#43484=CARTESIAN_POINT('',(-0.4,-4.89858719658941E-17,0.4));
#43485=CARTESIAN_POINT('',(-0.45,-5.51091059616309E-17,0.35));
#43486=CARTESIAN_POINT('Origin',(0.,0.,0.4));
#43487=CARTESIAN_POINT('Ctrl Pts',(0.285821514250018,-0.401076441581685,
-0.0493345805022535));
#43488=CARTESIAN_POINT('Ctrl Pts',(0.350543656524979,-0.354953112478679,
-0.0454821295218614));
#43489=CARTESIAN_POINT('Ctrl Pts',(0.456341900696097,-0.230941845013787,
-0.037777227561077));
#43490=CARTESIAN_POINT('Ctrl Pts',(0.532545219900247,0.0886035482833393,
-0.0223674236395085));
#43491=CARTESIAN_POINT('Ctrl Pts',(0.319330773560668,0.47994453109398,-0.00310516873754761));
#43492=CARTESIAN_POINT('Ctrl Pts',(-0.215290254258889,0.535025635481654,
0.0200095371448053));
#43493=CARTESIAN_POINT('Ctrl Pts',(-0.562384412092527,0.125896602679806,
0.0431242430271583));
#43494=CARTESIAN_POINT('Ctrl Pts',(-0.422683627229176,-0.392004271488446,
0.0662389489095112));
#43495=CARTESIAN_POINT('Ctrl Pts',(0.0835198470635792,-0.570404842180615,
0.0893536547918642));
#43496=CARTESIAN_POINT('Ctrl Pts',(0.517219798545357,-0.254477109971328,
0.112468360674217));
#43497=CARTESIAN_POINT('Ctrl Pts',(0.502837016033576,0.281900700313858,
0.13558306655657));
#43498=CARTESIAN_POINT('Ctrl Pts',(0.0527054858386194,0.574051566754687,
0.158697772438923));
#43499=CARTESIAN_POINT('Ctrl Pts',(-0.44304232133121,0.368766078993326,
0.181812478321276));
#43500=CARTESIAN_POINT('Ctrl Pts',(-0.554979510632384,-0.155996767962851,
0.204927184203629));
#43501=CARTESIAN_POINT('Ctrl Pts',(-0.185906336843711,-0.545680887986882,
0.228041890085982));
#43502=CARTESIAN_POINT('Ctrl Pts',(0.343997419455209,-0.462376423424824,
0.251156595968335));
#43503=CARTESIAN_POINT('Ctrl Pts',(0.576325602595985,0.0212396797004994,
0.274271301850687));
#43504=CARTESIAN_POINT('Ctrl Pts',(0.308311929055428,0.487096140686821,
0.297386007733041));
#43505=CARTESIAN_POINT('Ctrl Pts',(-0.135936610051597,0.522471279645762,
0.316648262635001));
#43506=CARTESIAN_POINT('Ctrl Pts',(-0.396756348714945,0.322748301101158,
0.33205806655657));
#43507=CARTESIAN_POINT('Ctrl Pts',(-0.466937021208664,0.175620002884023,
0.339762968517355));
#43508=CARTESIAN_POINT('Ctrl Pts',(-0.482707018258731,0.0977250455296118,
0.343615419497747));
#43509=CARTESIAN_POINT('Ctrl Pts',(0.269291261530787,-0.377880514723374,
-0.0328897203348357));
#43510=CARTESIAN_POINT('Ctrl Pts',(0.330270251821047,-0.334424690508254,
-0.0290372693544436));
#43511=CARTESIAN_POINT('Ctrl Pts',(0.429949741363115,-0.217585512928218,
-0.0213323673936592));
#43512=CARTESIAN_POINT('Ctrl Pts',(0.501745904136811,0.083479234780252,
-0.00592256347209064));
#43513=CARTESIAN_POINT('Ctrl Pts',(0.300862540328343,0.452187333001269,
0.0133396914298702));
#43514=CARTESIAN_POINT('Ctrl Pts',(-0.202839119080262,0.504082866918604,
0.0364543973122232));
#43515=CARTESIAN_POINT('Ctrl Pts',(-0.529859371135975,0.118615475979983,
0.0595691031945761));
#43516=CARTESIAN_POINT('Ctrl Pts',(-0.398238066520727,-0.369333026142464,
0.0826838090769291));
#43517=CARTESIAN_POINT('Ctrl Pts',(0.0786895452486333,-0.537415946231828,
0.105798514959282));
#43518=CARTESIAN_POINT('Ctrl Pts',(0.487306815949282,-0.23975963515099,
0.128913220841635));
#43519=CARTESIAN_POINT('Ctrl Pts',(0.473755849860941,0.265597204651036,
0.152027926723988));
#43520=CARTESIAN_POINT('Ctrl Pts',(0.0496573073175292,0.540851765482816,
0.175142632606341));
#43521=CARTESIAN_POINT('Ctrl Pts',(-0.417419332256589,0.347438795440041,
0.198257338488694));
#43522=CARTESIAN_POINT('Ctrl Pts',(-0.522882726074999,-0.146974822905372,
0.221372044371047));
#43523=CARTESIAN_POINT('Ctrl Pts',(-0.175154596415085,-0.51412188163935,
0.2444867502534));
#43524=CARTESIAN_POINT('Ctrl Pts',(0.324102611000083,-0.435635262422014,
0.267601456135753));
#43525=CARTESIAN_POINT('Ctrl Pts',(0.542994284327405,0.0200113002552149,
0.290716162018105));
#43526=CARTESIAN_POINT('Ctrl Pts',(0.290480961652527,0.458925335122226,
0.313830867900458));
#43527=CARTESIAN_POINT('Ctrl Pts',(-0.128074827764688,0.492254581949836,
0.333093122802419));
#43528=CARTESIAN_POINT('Ctrl Pts',(-0.373810270882328,0.3040824179681,0.348502926723988));
#43529=CARTESIAN_POINT('Ctrl Pts',(-0.439932101775649,0.165463164138548,
0.356207828684772));
#43530=CARTESIAN_POINT('Ctrl Pts',(-0.454790053987863,0.0920731977187791,
0.360060279665165));
#43531=CARTESIAN_POINT('Ctrl Pts',(0.252761008811555,-0.354684587865062,
-0.0164448601674179));
#43532=CARTESIAN_POINT('Ctrl Pts',(0.309996847117115,-0.313896268537829,
-0.0125924091870257));
#43533=CARTESIAN_POINT('Ctrl Pts',(0.403557582030132,-0.204229180842649,
-0.00488750722624137));
#43534=CARTESIAN_POINT('Ctrl Pts',(0.470946588373376,0.0783549212771649,
0.0105222966953272));
#43535=CARTESIAN_POINT('Ctrl Pts',(0.282394307096019,0.424430134908558,
0.029784551597288));
#43536=CARTESIAN_POINT('Ctrl Pts',(-0.190387983901635,0.473140098355552,
0.052899257479641));
#43537=CARTESIAN_POINT('Ctrl Pts',(-0.497334330179422,0.111334349280159,
0.076013963361994));
#43538=CARTESIAN_POINT('Ctrl Pts',(-0.373792505812278,-0.346661780796483,
0.0991286692443469));
#43539=CARTESIAN_POINT('Ctrl Pts',(0.0738592434336875,-0.50442705028304,
0.1222433751267));
#43540=CARTESIAN_POINT('Ctrl Pts',(0.457393833353206,-0.225042160330651,
0.145358081009053));
#43541=CARTESIAN_POINT('Ctrl Pts',(0.444674683688306,0.249293708988214,
0.168472786891406));
#43542=CARTESIAN_POINT('Ctrl Pts',(0.0466091287964395,0.507651964210947,
0.191587492773759));
#43543=CARTESIAN_POINT('Ctrl Pts',(-0.391796343181968,0.326111511886755,
0.214702198656111));
#43544=CARTESIAN_POINT('Ctrl Pts',(-0.490785941517614,-0.137952877847892,
0.237816904538465));
#43545=CARTESIAN_POINT('Ctrl Pts',(-0.164402855986459,-0.482562875291818,
0.260931610420817));
#43546=CARTESIAN_POINT('Ctrl Pts',(0.304207802544958,-0.408894101419205,
0.28404631630317));
#43547=CARTESIAN_POINT('Ctrl Pts',(0.509662966058825,0.0187829208099306,
0.307161022185524));
#43548=CARTESIAN_POINT('Ctrl Pts',(0.272649994249626,0.430754529557631,
0.330275728067876));
#43549=CARTESIAN_POINT('Ctrl Pts',(-0.120213045477778,0.46203788425391,
0.349537982969837));
#43550=CARTESIAN_POINT('Ctrl Pts',(-0.350864193049711,0.285416534835041,
0.364947786891406));
#43551=CARTESIAN_POINT('Ctrl Pts',(-0.412927182342633,0.155306325393072,
0.37265268885219));
#43552=CARTESIAN_POINT('Ctrl Pts',(-0.426873089716994,0.0864213499079464,
0.376505139832582));
#43553=CARTESIAN_POINT('Ctrl Pts',(0.236230756092324,-0.331488661006751,
-5.55111512312578E-17));
#43554=CARTESIAN_POINT('Ctrl Pts',(0.289723442413183,-0.293367846567404,
0.00385245098039209));
#43555=CARTESIAN_POINT('Ctrl Pts',(0.37716542269715,-0.19087284875708,0.0115573529411765));
#43556=CARTESIAN_POINT('Ctrl Pts',(0.44014727260994,0.0732306077740779,
0.026967156862745));
#43557=CARTESIAN_POINT('Ctrl Pts',(0.263926073863695,0.396672936815846,
0.0462294117647059));
#43558=CARTESIAN_POINT('Ctrl Pts',(-0.177936848723007,0.442197329792502,
0.0693441176470588));
#43559=CARTESIAN_POINT('Ctrl Pts',(-0.46480928922287,0.104053222580335,
0.0924588235294117));
#43560=CARTESIAN_POINT('Ctrl Pts',(-0.349346945103829,-0.323990535450501,
0.115573529411765));
#43561=CARTESIAN_POINT('Ctrl Pts',(0.0690289416187412,-0.471438154334252,
0.138688235294118));
#43562=CARTESIAN_POINT('Ctrl Pts',(0.427480850757132,-0.210324685510313,
0.161802941176471));
#43563=CARTESIAN_POINT('Ctrl Pts',(0.41559351751567,0.232990213325393,0.184917647058823));
#43564=CARTESIAN_POINT('Ctrl Pts',(0.0435609502753498,0.474452162939076,
0.208032352941177));
#43565=CARTESIAN_POINT('Ctrl Pts',(-0.366173354107348,0.304784228333469,
0.231147058823529));
#43566=CARTESIAN_POINT('Ctrl Pts',(-0.458689156960228,-0.128930932790413,
0.254261764705883));
#43567=CARTESIAN_POINT('Ctrl Pts',(-0.153651115557833,-0.451003868944285,
0.277376470588235));
#43568=CARTESIAN_POINT('Ctrl Pts',(0.284312994089833,-0.382152940416395,
0.300491176470589));
#43569=CARTESIAN_POINT('Ctrl Pts',(0.476331647790245,0.0175545413646465,
0.323605882352941));
#43570=CARTESIAN_POINT('Ctrl Pts',(0.254819026846725,0.402583723993036,
0.346720588235294));
#43571=CARTESIAN_POINT('Ctrl Pts',(-0.112351263190869,0.431821186557985,
0.365982843137255));
#43572=CARTESIAN_POINT('Ctrl Pts',(-0.327918115217093,0.266750651701983,
0.381392647058824));
#43573=CARTESIAN_POINT('Ctrl Pts',(-0.385922262909618,0.145149486647597,
0.389097549019608));
#43574=CARTESIAN_POINT('Ctrl Pts',(-0.398956125446125,0.0807695020971137,
0.39295));
#43575=CARTESIAN_POINT('',(0.236230756092325,-0.331488661006751,0.));
#43576=CARTESIAN_POINT('Ctrl Pts',(0.236230756092324,-0.331488661006751,
-5.55111512312578E-17));
#43577=CARTESIAN_POINT('Ctrl Pts',(0.289723442413183,-0.293367846567404,
0.00385245098039209));
#43578=CARTESIAN_POINT('Ctrl Pts',(0.37716542269715,-0.19087284875708,0.0115573529411765));
#43579=CARTESIAN_POINT('Ctrl Pts',(0.44014727260994,0.0732306077740779,
0.026967156862745));
#43580=CARTESIAN_POINT('Ctrl Pts',(0.263926073863695,0.396672936815846,
0.0462294117647059));
#43581=CARTESIAN_POINT('Ctrl Pts',(-0.177936848723007,0.442197329792502,
0.0693441176470588));
#43582=CARTESIAN_POINT('Ctrl Pts',(-0.390945071629489,0.191118922825079,
0.0865072247563608));
#43583=CARTESIAN_POINT('Ctrl Pts',(-0.407283047524291,0.0301769837418441,
0.0959654299048784));
#43584=CARTESIAN_POINT('Ctrl Pts',(-0.407034641531608,0.000294318473894748,
0.0977187330926118));
#43585=CARTESIAN_POINT('Ctrl Pts',(0.217447815076512,0.442338803773993,
-3.8597597340484E-17));
#43586=CARTESIAN_POINT('Ctrl Pts',(0.235771185649973,0.431537188392035,
-4.42054783740276E-17));
#43587=CARTESIAN_POINT('Ctrl Pts',(0.253300690580711,0.419546382573851,
-1.43244558183068E-17));
#43588=CARTESIAN_POINT('Ctrl Pts',(0.269890299702997,0.406369790209568,
2.16840434497101E-17));
#43589=CARTESIAN_POINT('Ctrl Pts',(0.281071263833339,0.397489110411798,
4.87538430948304E-17));
#43590=CARTESIAN_POINT('Ctrl Pts',(0.291824924692404,0.388069292305422,
-6.77184820252973E-17));
#43591=CARTESIAN_POINT('Ctrl Pts',(0.30213264706158,0.37815074175771,-7.80625564189563E-17));
#43592=CARTESIAN_POINT('Ctrl Pts',(0.30776728830288,0.372728838453719,-8.37170692292625E-17));
#43593=CARTESIAN_POINT('Ctrl Pts',(0.313270261594427,0.367156075512075,
1.65417925227048E-18));
#43594=CARTESIAN_POINT('Ctrl Pts',(0.318632624766842,0.361444505503272,
-7.80625564189563E-18));
#43595=CARTESIAN_POINT('Ctrl Pts',(0.336033064429788,0.342910917582537,
-3.85046103165619E-17));
#43596=CARTESIAN_POINT('Ctrl Pts',(0.351905028805777,0.322974626561441,
-8.88307993243271E-18));
#43597=CARTESIAN_POINT('Ctrl Pts',(0.366150538251326,0.301871858897891,
3.46944695195361E-17));
#43598=CARTESIAN_POINT('Ctrl Pts',(0.372568420276111,0.292364647254896,
5.4327012138036E-17));
#43599=CARTESIAN_POINT('Ctrl Pts',(0.37865556572648,0.282620326083274,3.4499532893746E-17));
#43600=CARTESIAN_POINT('Ctrl Pts',(0.384399785951081,0.272659327527138,
5.89805981832114E-17));
#43601=CARTESIAN_POINT('Ctrl Pts',(0.388480791465398,0.265582494041263,
7.6373274392731E-17));
#43602=CARTESIAN_POINT('Ctrl Pts',(0.392390160301114,0.25839280128157,2.53748915853478E-17));
#43603=CARTESIAN_POINT('Ctrl Pts',(0.396111438865062,0.251121487239994,
2.25514051876985E-17));
#43604=CARTESIAN_POINT('Ctrl Pts',(0.40745358116902,0.228959137074835,1.39456574681695E-17));
#43605=CARTESIAN_POINT('Ctrl Pts',(0.417077210155165,0.205999660918854,
-8.66004344781302E-17));
#43606=CARTESIAN_POINT('Ctrl Pts',(0.424881751749804,0.182459781868829,
-6.93889390390723E-17));
#43607=CARTESIAN_POINT('Ctrl Pts',(0.430607845296002,0.165188870070598,
-5.6761082327833E-17));
#43608=CARTESIAN_POINT('Ctrl Pts',(0.435353796515255,0.147604950608036,
7.4600576781502E-17));
#43609=CARTESIAN_POINT('Ctrl Pts',(0.439061990731694,0.129792158612379,
1.00613961606655E-16));
#43610=CARTESIAN_POINT('Ctrl Pts',(0.441052023831415,0.120232776443923,
1.14574259750785E-16));
#43611=CARTESIAN_POINT('Ctrl Pts',(0.442742911254792,0.11060749250059,6.5499624826844E-17));
#43612=CARTESIAN_POINT('Ctrl Pts',(0.444123791797554,0.100929672122365,
6.24500451351651E-17));
#43613=CARTESIAN_POINT('Ctrl Pts',(0.445088133438485,0.094171140232625,
6.03203629556022E-17));
#43614=CARTESIAN_POINT('Ctrl Pts',(0.445901192054133,0.087385117597804,
9.07916038813422E-17));
#43615=CARTESIAN_POINT('Ctrl Pts',(0.446557500931817,0.0805979169647933,
8.32667268468867E-17));
#43616=CARTESIAN_POINT('Ctrl Pts',(0.448915348394345,0.056214300752433,
5.62329431745785E-17));
#43617=CARTESIAN_POINT('Ctrl Pts',(0.449264882015899,0.0317529871848161,
2.53752424620923E-17));
#43618=CARTESIAN_POINT('Ctrl Pts',(0.447476027996775,0.00742372749985042,
2.77555756156289E-17));
#43619=CARTESIAN_POINT('Ctrl Pts',(0.446180524189214,-0.0101957362574197,
2.94794338123863E-17));
#43620=CARTESIAN_POINT('Ctrl Pts',(0.443762029056545,-0.0277461199319404,
4.3074745668937E-17));
#43621=CARTESIAN_POINT('Ctrl Pts',(0.440260086235777,-0.045127533989719,
5.55111512312578E-17));
#43622=CARTESIAN_POINT('Ctrl Pts',(0.438497782445595,-0.0538744877352476,
6.17695985504835E-17));
#43623=CARTESIAN_POINT('Ctrl Pts',(0.436460883233537,-0.0625785391661663,
4.81993018880041E-17));
#43624=CARTESIAN_POINT('Ctrl Pts',(0.434153233316401,-0.0712260787334543,
5.55111512312578E-17));
#43625=CARTESIAN_POINT('Ctrl Pts',(0.432455960374384,-0.0775863306995747,
6.08890051051305E-17));
#43626=CARTESIAN_POINT('Ctrl Pts',(0.43061151612711,-0.0839173798140132,
-1.92100666488577E-17));
#43627=CARTESIAN_POINT('Ctrl Pts',(0.42862810433969,-0.0901940790812472,
-1.38777878078145E-17));
#43628=CARTESIAN_POINT('Ctrl Pts',(0.421563946478226,-0.112549292836608,
5.11375985434415E-18));
#43629=CARTESIAN_POINT('Ctrl Pts',(0.412726164773691,-0.134275543420596,
-3.59125272893349E-17));
#43630=CARTESIAN_POINT('Ctrl Pts',(0.402223235339076,-0.155144150016548,
-2.08166817117217E-17));
#43631=CARTESIAN_POINT('Ctrl Pts',(0.395782695443094,-0.16794106483841,
-1.15597028553478E-17));
#43632=CARTESIAN_POINT('Ctrl Pts',(0.388715069443995,-0.18041506830769,
9.54523787347189E-17));
#43633=CARTESIAN_POINT('Ctrl Pts',(0.381038025471632,-0.192507033808116,
9.71445146547012E-17));
#43634=CARTESIAN_POINT('Ctrl Pts',(0.374554680793545,-0.202718826323181,
9.88257224754246E-17));
#43635=CARTESIAN_POINT('Ctrl Pts',(0.367636567228464,-0.212658063476375,
4.58363829752519E-17));
#43636=CARTESIAN_POINT('Ctrl Pts',(0.360298753602303,-0.222297236750623,
4.16333634234434E-17));
#43637=CARTESIAN_POINT('Ctrl Pts',(0.356885786025934,-0.226780613887746,
3.96784528487154E-17));
#43638=CARTESIAN_POINT('Ctrl Pts',(0.353381726209429,-0.231199059390674,
-6.35056968455181E-17));
#43639=CARTESIAN_POINT('Ctrl Pts',(0.349797863823796,-0.235538458422797,
-6.24500451351651E-17));
#43640=CARTESIAN_POINT('Ctrl Pts',(0.335312213365481,-0.253077920270008,
-5.81831955643792E-17));
#43641=CARTESIAN_POINT('Ctrl Pts',(0.319489163245678,-0.269378119582282,
-1.177990700976E-17));
#43642=CARTESIAN_POINT('Ctrl Pts',(0.302455374280317,-0.284284251770872,
-3.46944695195361E-17));
#43643=CARTESIAN_POINT('Ctrl Pts',(0.285837815097629,-0.298826144612952,
-5.70491023863626E-17));
#43644=CARTESIAN_POINT('Ctrl Pts',(0.268066931012482,-0.312041854936447,
1.51086484203379E-17));
#43645=CARTESIAN_POINT('Ctrl Pts',(0.249239140885698,-0.323743396449302,
0.));
#43646=CARTESIAN_POINT('Ctrl Pts',(0.244957374879624,-0.326404529929706,
-3.43596868077925E-18));
#43647=CARTESIAN_POINT('Ctrl Pts',(0.240620893760326,-0.32898714764827,
-1.20546207527071E-17));
#43648=CARTESIAN_POINT('Ctrl Pts',(0.236230756092325,-0.331488661006751,
-1.38777878078145E-17));
#43649=CARTESIAN_POINT('Ctrl Pts',(0.0698314663893245,0.486747372427084,
0.3075));
#43650=CARTESIAN_POINT('Ctrl Pts',(0.13882856656482,0.47715546868819,0.304128669244347));
#43651=CARTESIAN_POINT('Ctrl Pts',(0.20570919792813,0.453597245499616,0.300757338488694));
#43652=CARTESIAN_POINT('Ctrl Pts',(0.264131166824116,0.416528424980888,
0.297386007733041));
#43653=CARTESIAN_POINT('Ctrl Pts',(0.397649820235614,0.33181065369138,0.289681105772257));
#43654=CARTESIAN_POINT('Ctrl Pts',(0.486987711415799,0.17652516669594,0.281976203811472));
#43655=CARTESIAN_POINT('Ctrl Pts',(0.492935293149096,0.0182797393439991,
0.274271301850688));
#43656=CARTESIAN_POINT('Ctrl Pts',(0.498882874882393,-0.139965688007942,
0.266566399889903));
#43657=CARTESIAN_POINT('Ctrl Pts',(0.421440147168801,-0.301171055716382,
0.258861497929119));
#43658=CARTESIAN_POINT('Ctrl Pts',(0.294401490595519,-0.395657816997613,
0.251156595968335));
#43659=CARTESIAN_POINT('Ctrl Pts',(0.167362834022236,-0.490144578278843,
0.243451694007551));
#43660=CARTESIAN_POINT('Ctrl Pts',(-0.00927175141073788,-0.517912733132863,
0.235746792046766));
#43661=CARTESIAN_POINT('Ctrl Pts',(-0.15910123975867,-0.466849457222534,
0.228041890085982));
#43662=CARTESIAN_POINT('Ctrl Pts',(-0.308930728106602,-0.415786181312205,
0.220336988125198));
#43663=CARTESIAN_POINT('Ctrl Pts',(-0.431955119369493,-0.285891474637528,
0.212632086164413));
#43664=CARTESIAN_POINT('Ctrl Pts',(-0.474811116784076,-0.133483646807493,
0.204927184203629));
#43665=CARTESIAN_POINT('Ctrl Pts',(-0.486942274642154,-0.0903418806661754,
0.202746173665872));
#43666=CARTESIAN_POINT('Ctrl Pts',(-0.492649743945157,-0.0453961956515631,
0.200565163128115));
#43667=CARTESIAN_POINT('Ctrl Pts',(-0.492300964172325,-0.000364928074014725,
0.198384152590358));
#43668=CARTESIAN_POINT('Origin',(0.,0.,-0.277281266907388));
#43669=CARTESIAN_POINT('',(-0.236771598461275,-0.331576719094244,-5.03775273800896E-17));
#43670=CARTESIAN_POINT('Ctrl Pts',(-0.236771598461276,-0.331576719094244,
-2.30935062739412E-17));
#43671=CARTESIAN_POINT('Ctrl Pts',(-0.141722621809602,-0.398300946144845,
0.00683327564849024));
#43672=CARTESIAN_POINT('Ctrl Pts',(0.126781614045834,-0.452218967011808,
0.0214259299022832));
#43673=CARTESIAN_POINT('Ctrl Pts',(0.447438415353507,-0.166418058771462,
0.0437779627613788));
#43674=CARTESIAN_POINT('Ctrl Pts',(0.389000999211174,0.276972659072313,
0.067056098577287));
#43675=CARTESIAN_POINT('Ctrl Pts',(-0.0110871576621449,0.477410398031793,
0.0903342343931949));
#43676=CARTESIAN_POINT('Ctrl Pts',(-0.347644687561783,0.288793871360888,
0.110409290503229));
#43677=CARTESIAN_POINT('Ctrl Pts',(-0.406221861873601,0.0777548455075631,
0.12272496800796));
#43678=CARTESIAN_POINT('Ctrl Pts',(-0.406522025929715,-0.000167002740521567,
0.127281266907388));
#43679=CARTESIAN_POINT('Origin',(0.,0.,0.));
#43680=CARTESIAN_POINT('Ctrl Pts',(-0.179217368492184,0.36547344271607,
-0.0493345805022535));
#43681=CARTESIAN_POINT('Ctrl Pts',(-0.238611205238638,0.336348461575858,
-0.0454548911996022));
#43682=CARTESIAN_POINT('Ctrl Pts',(-0.342150032955443,0.248603248616071,
-0.0376955125942995));
#43683=CARTESIAN_POINT('Ctrl Pts',(-0.44676970066958,-0.00417527992601634,
-0.0221767553836941));
#43684=CARTESIAN_POINT('Ctrl Pts',(-0.320810106679502,-0.353702698155029,
-0.00277830887043734));
#43685=CARTESIAN_POINT('Ctrl Pts',(0.113495967335977,-0.464060443259162,
0.0204998269454708));
#43686=CARTESIAN_POINT('Ctrl Pts',(0.447438415353507,-0.166418058771462,
0.0437779627613788));
#43687=CARTESIAN_POINT('Ctrl Pts',(0.389000999211174,0.276972659072313,
0.067056098577287));
#43688=CARTESIAN_POINT('Ctrl Pts',(-0.0110871576621449,0.477410398031793,
0.0903342343931949));
#43689=CARTESIAN_POINT('Ctrl Pts',(-0.401344193454667,0.258699122660778,
0.113612370209103));
#43690=CARTESIAN_POINT('Ctrl Pts',(-0.439359289932517,-0.187051465698632,
0.136890506025011));
#43691=CARTESIAN_POINT('Ctrl Pts',(-0.0916847062669661,-0.468629856473293,
0.160168641840919));
#43692=CARTESIAN_POINT('Ctrl Pts',(0.336453410254844,-0.338849716643417,
0.183446777656827));
#43693=CARTESIAN_POINT('Ctrl Pts',(0.46926975494663,0.088378354603048,0.206724913472736));
#43694=CARTESIAN_POINT('Ctrl Pts',(0.190156376929569,0.437998801366229,
0.230003049288643));
#43695=CARTESIAN_POINT('Ctrl Pts',(-0.255854007963939,0.403215004461254,
0.253281185104552));
#43696=CARTESIAN_POINT('Ctrl Pts',(-0.477314526631585,0.0143692006508807,
0.27655932092046));
#43697=CARTESIAN_POINT('Ctrl Pts',(-0.279730339285618,-0.386842400859151,
0.299837456736368));
#43698=CARTESIAN_POINT('Ctrl Pts',(0.163268921903001,-0.448972926511222,
0.323115592552276));
#43699=CARTESIAN_POINT('Ctrl Pts',(0.463203848138002,-0.116047052095292,
0.346393728368184));
#43700=CARTESIAN_POINT('Ctrl Pts',(0.373893623429547,0.244589772389548,
0.365792174881441));
#43701=CARTESIAN_POINT('Ctrl Pts',(0.146530577079214,0.396735441137677,
0.381310932092046));
#43702=CARTESIAN_POINT('Ctrl Pts',(0.0116987864547665,0.412224129892184,
0.389070310697349));
#43703=CARTESIAN_POINT('Ctrl Pts',(-0.0538698874795526,0.403469624287802,
0.39295));
#43704=CARTESIAN_POINT('Ctrl Pts',(-0.191758108071807,0.391047455474608,
-0.0328897203348357));
#43705=CARTESIAN_POINT('Ctrl Pts',(-0.255308029942927,0.359884453093409,
-0.0290100310321843));
#43706=CARTESIAN_POINT('Ctrl Pts',(-0.366091989566869,0.265999266790941,
-0.0212506524268816));
#43707=CARTESIAN_POINT('Ctrl Pts',(-0.478032420992403,-0.00446744523713975,
-0.00573189521627628));
#43708=CARTESIAN_POINT('Ctrl Pts',(-0.343258801447355,-0.378453052785785,
0.0136665512969805));
#43709=CARTESIAN_POINT('Ctrl Pts',(0.121437850322391,-0.496533083701774,
0.0369446871128886));
#43710=CARTESIAN_POINT('Ctrl Pts',(0.478747929002081,-0.178063166352039,
0.0602228229287966));
#43711=CARTESIAN_POINT('Ctrl Pts',(0.416221353289375,0.296353827411771,
0.0835009587447048));
#43712=CARTESIAN_POINT('Ctrl Pts',(-0.0118629817805825,0.510817201873923,
0.106779094560613));
#43713=CARTESIAN_POINT('Ctrl Pts',(-0.429428262840657,0.276801599859618,
0.130057230376521));
#43714=CARTESIAN_POINT('Ctrl Pts',(-0.470103466589548,-0.200140396414718,
0.153335366192429));
#43715=CARTESIAN_POINT('Ctrl Pts',(-0.098100345746565,-0.501422241713142,
0.176613502008337));
#43716=CARTESIAN_POINT('Ctrl Pts',(0.359996745558678,-0.362560733543208,
0.199891637824245));
#43717=CARTESIAN_POINT('Ctrl Pts',(0.502106917097217,0.0945626320471215,
0.223169773640153));
#43718=CARTESIAN_POINT('Ctrl Pts',(0.203462573882139,0.468647777803804,
0.246447909456061));
#43719=CARTESIAN_POINT('Ctrl Pts',(-0.273757398194884,0.431429983891475,
0.269726045271969));
#43720=CARTESIAN_POINT('Ctrl Pts',(-0.510714621870228,0.0153746858047257,
0.293004181087878));
#43721=CARTESIAN_POINT('Ctrl Pts',(-0.299304476362928,-0.413911706966848,
0.316282316903785));
#43722=CARTESIAN_POINT('Ctrl Pts',(0.174693668557066,-0.480389817614186,
0.339560452719694));
#43723=CARTESIAN_POINT('Ctrl Pts',(0.495616548316844,-0.1241674472978,0.362838588535602));
#43724=CARTESIAN_POINT('Ctrl Pts',(0.400056838531749,0.261704947470977,
0.382237035048858));
#43725=CARTESIAN_POINT('Ctrl Pts',(0.156784057660157,0.42449701297178,0.397755792259464));
#43726=CARTESIAN_POINT('Ctrl Pts',(0.0125174093123678,0.441069523086539,
0.405515170864767));
#43727=CARTESIAN_POINT('Ctrl Pts',(-0.0576394341242136,0.43170242074638,
0.409394860167418));
#43728=CARTESIAN_POINT('Ctrl Pts',(-0.20429884765143,0.416621468233146,
-0.0164448601674178));
#43729=CARTESIAN_POINT('Ctrl Pts',(-0.272004854647215,0.38342044461096,
-0.0125651708647665));
#43730=CARTESIAN_POINT('Ctrl Pts',(-0.390033946178295,0.283395284965812,
-0.00480579225946384));
#43731=CARTESIAN_POINT('Ctrl Pts',(-0.509295141315226,-0.00475961054826249,
0.0107129649511416));
#43732=CARTESIAN_POINT('Ctrl Pts',(-0.365707496215208,-0.403203407416541,
0.0301114114643983));
#43733=CARTESIAN_POINT('Ctrl Pts',(0.129379733308805,-0.529005724144386,
0.0533895472803064));
#43734=CARTESIAN_POINT('Ctrl Pts',(0.510057442650656,-0.189708273932616,
0.0766676830962145));
#43735=CARTESIAN_POINT('Ctrl Pts',(0.443441707367576,0.315734995751229,
0.0999458189121226));
#43736=CARTESIAN_POINT('Ctrl Pts',(-0.0126388058990205,0.544224005716052,
0.123223954728031));
#43737=CARTESIAN_POINT('Ctrl Pts',(-0.457512332226647,0.294904077058458,
0.146502090543939));
#43738=CARTESIAN_POINT('Ctrl Pts',(-0.500847643246579,-0.213229327130804,
0.169780226359847));
#43739=CARTESIAN_POINT('Ctrl Pts',(-0.104515985226164,-0.534214626952992,
0.193058362175755));
#43740=CARTESIAN_POINT('Ctrl Pts',(0.383540080862511,-0.386271750443,0.216336497991663));
#43741=CARTESIAN_POINT('Ctrl Pts',(0.534944079247805,0.100746909491195,
0.239614633807571));
#43742=CARTESIAN_POINT('Ctrl Pts',(0.21676877083471,0.499296754241378,0.262892769623479));
#43743=CARTESIAN_POINT('Ctrl Pts',(-0.291660788425829,0.459644963321696,
0.286170905439387));
#43744=CARTESIAN_POINT('Ctrl Pts',(-0.544114717108871,0.0163801709585708,
0.309449041255295));
#43745=CARTESIAN_POINT('Ctrl Pts',(-0.318878613440237,-0.440981013074545,
0.332727177071203));
#43746=CARTESIAN_POINT('Ctrl Pts',(0.186118415211131,-0.511806708717149,
0.356005312887112));
#43747=CARTESIAN_POINT('Ctrl Pts',(0.528029248495686,-0.132287842500309,
0.37928344870302));
#43748=CARTESIAN_POINT('Ctrl Pts',(0.426220053633952,0.278820122552406,
0.398681895216276));
#43749=CARTESIAN_POINT('Ctrl Pts',(0.167037538241101,0.452258584805883,
0.414200652426882));
#43750=CARTESIAN_POINT('Ctrl Pts',(0.0133360321699692,0.469914916280895,
0.421960031032184));
#43751=CARTESIAN_POINT('Ctrl Pts',(-0.0614089807688746,0.459935217204959,
0.425839720334836));
#43752=CARTESIAN_POINT('Ctrl Pts',(-0.216839587231054,0.442195480991683,
0.));
#43753=CARTESIAN_POINT('Ctrl Pts',(-0.288701679351503,0.406956436128511,
0.00387968930265134));
#43754=CARTESIAN_POINT('Ctrl Pts',(-0.413975902789721,0.300791303140682,
0.011639067907954));
#43755=CARTESIAN_POINT('Ctrl Pts',(-0.54055786163805,-0.00505177585938594,
0.0271578251185594));
#43756=CARTESIAN_POINT('Ctrl Pts',(-0.38815619098306,-0.427953762047296,
0.0465562716318161));
#43757=CARTESIAN_POINT('Ctrl Pts',(0.137321616295219,-0.561478364586998,
0.0698344074477243));
#43758=CARTESIAN_POINT('Ctrl Pts',(0.541366956299231,-0.201353381513192,
0.0931125432636322));
#43759=CARTESIAN_POINT('Ctrl Pts',(0.470662061445776,0.335116164090687,
0.11639067907954));
#43760=CARTESIAN_POINT('Ctrl Pts',(-0.0134146300174581,0.577630809558183,
0.139668814895449));
#43761=CARTESIAN_POINT('Ctrl Pts',(-0.485596401612636,0.313006554257298,
0.162946950711356));
#43762=CARTESIAN_POINT('Ctrl Pts',(-0.53159181990361,-0.226318257846889,
0.186225086527265));
#43763=CARTESIAN_POINT('Ctrl Pts',(-0.110931624705763,-0.567007012192843,
0.209503222343173));
#43764=CARTESIAN_POINT('Ctrl Pts',(0.407083416166345,-0.409982767342791,
0.232781358159081));
#43765=CARTESIAN_POINT('Ctrl Pts',(0.567781241398392,0.106931186935269,
0.256059493974989));
#43766=CARTESIAN_POINT('Ctrl Pts',(0.230074967787281,0.529945730678953,
0.279337629790897));
#43767=CARTESIAN_POINT('Ctrl Pts',(-0.309564178656774,0.487859942751916,
0.302615765606805));
#43768=CARTESIAN_POINT('Ctrl Pts',(-0.577514812347514,0.0173856561124158,
0.325893901422713));
#43769=CARTESIAN_POINT('Ctrl Pts',(-0.338452750517546,-0.468050319182243,
0.349172037238622));
#43770=CARTESIAN_POINT('Ctrl Pts',(0.197543161865195,-0.543223599820112,
0.372450173054529));
#43771=CARTESIAN_POINT('Ctrl Pts',(0.560441948674527,-0.140408237702817,
0.395728308870437));
#43772=CARTESIAN_POINT('Ctrl Pts',(0.452383268736155,0.295935297633835,
0.415126755383694));
#43773=CARTESIAN_POINT('Ctrl Pts',(0.177291018822044,0.480020156639985,
0.4306455125943));
#43774=CARTESIAN_POINT('Ctrl Pts',(0.0141546550275704,0.49876030947525,
0.438404891199602));
#43775=CARTESIAN_POINT('Ctrl Pts',(-0.0651785274135356,0.488168013663537,
0.442284580502254));
#43776=CARTESIAN_POINT('Ctrl Pts',(-0.491861190935719,-0.000202060802622812,
0.176615847409642));
#43777=CARTESIAN_POINT('Ctrl Pts',(-0.492116503801431,-0.0664806507023142,
0.179818927115516));
#43778=CARTESIAN_POINT('Ctrl Pts',(-0.479592887105073,-0.13266715951835,
0.18302200682139));
#43779=CARTESIAN_POINT('Ctrl Pts',(-0.45381588432214,-0.193212248220517,
0.186225086527265));
#43780=CARTESIAN_POINT('Ctrl Pts',(-0.391371754837661,-0.339881175962207,
0.193984465132567));
#43781=CARTESIAN_POINT('Ctrl Pts',(-0.251151689771712,-0.453444094077525,
0.20174384373787));
#43782=CARTESIAN_POINT('Ctrl Pts',(-0.0947058170933862,-0.484054845660175,
0.209503222343173));
#43783=CARTESIAN_POINT('Ctrl Pts',(0.0617400555849396,-0.514665597242825,
0.217262600948475));
#43784=CARTESIAN_POINT('Ctrl Pts',(0.234411735875642,-0.462324182292808,
0.225021979553778));
#43785=CARTESIAN_POINT('Ctrl Pts',(0.347530546893001,-0.35000114910479,
0.232781358159081));
#43786=CARTESIAN_POINT('Ctrl Pts',(0.46064935791036,-0.237678115916771,
0.240540736764384));
#43787=CARTESIAN_POINT('Ctrl Pts',(0.514215299654376,-0.0653734644907513,
0.248300115369686));
#43788=CARTESIAN_POINT('Ctrl Pts',(0.484713891591199,0.0912812851795395,
0.256059493974989));
#43789=CARTESIAN_POINT('Ctrl Pts',(0.455212483528021,0.24793603484983,0.263818872580292));
#43790=CARTESIAN_POINT('Ctrl Pts',(0.342643725657651,0.388940882764392,
0.271578251185594));
#43791=CARTESIAN_POINT('Ctrl Pts',(0.19641948898179,0.452429008733833,0.279337629790897));
#43792=CARTESIAN_POINT('Ctrl Pts',(0.0501952523059287,0.515917134703274,
0.2870970083962));
#43793=CARTESIAN_POINT('Ctrl Pts',(-0.129684463175423,0.501888538727595,
0.294856387001502));
#43794=CARTESIAN_POINT('Ctrl Pts',(-0.264282759864555,0.416461859633172,
0.302615765606805));
#43795=CARTESIAN_POINT('Ctrl Pts',(-0.292524266622378,0.398537575342149,
0.30424384373787));
#43796=CARTESIAN_POINT('Ctrl Pts',(-0.318772271610817,0.377470010455589,
0.305871921868935));
#43797=CARTESIAN_POINT('Ctrl Pts',(-0.342664481608841,0.353895656000101,
0.3075));
#43798=CARTESIAN_POINT('Ctrl Pts',(-0.236771598461275,-0.331576719094244,
1.77809156287623E-17));
#43799=CARTESIAN_POINT('Ctrl Pts',(-0.250685093761403,-0.323785106371382,
1.80035313947998E-17));
#43800=CARTESIAN_POINT('Ctrl Pts',(-0.264074236959953,-0.315173418978676,
2.94409432717802E-17));
#43801=CARTESIAN_POINT('Ctrl Pts',(-0.276852406183546,-0.305762684301697,
2.29850860566927E-17));
#43802=CARTESIAN_POINT('Ctrl Pts',(-0.287822209380187,-0.297683756441541,
1.72958474292146E-17));
#43803=CARTESIAN_POINT('Ctrl Pts',(-0.298341885321039,-0.289015772946681,
3.86197526290172E-17));
#43804=CARTESIAN_POINT('Ctrl Pts',(-0.308399583438957,-0.27981147161853,
4.68375338513738E-17));
#43805=CARTESIAN_POINT('Ctrl Pts',(-0.313176580152552,-0.275439803600658,
5.07406450237306E-17));
#43806=CARTESIAN_POINT('Ctrl Pts',(-0.317849715293028,-0.270946637032549,
2.78009939264429E-17));
#43807=CARTESIAN_POINT('Ctrl Pts',(-0.322416173250408,-0.266338360354402,
3.55618312575245E-17));
#43808=CARTESIAN_POINT('Ctrl Pts',(-0.338339031391128,-0.250269683821266,
6.26232239232097E-17));
#43809=CARTESIAN_POINT('Ctrl Pts',(-0.352891345987932,-0.232881717338864,
-2.29443486208257E-18));
#43810=CARTESIAN_POINT('Ctrl Pts',(-0.366023507015969,-0.214414045295771,
2.25514051876985E-17));
#43811=CARTESIAN_POINT('Ctrl Pts',(-0.372915048500564,-0.204722515642947,
3.55900921987028E-17));
#43812=CARTESIAN_POINT('Ctrl Pts',(-0.379415068568767,-0.194732824866228,
9.50689841530354E-17));
#43813=CARTESIAN_POINT('Ctrl Pts',(-0.385513091657106,-0.184475102093045,
8.15320033709099E-17));
#43814=CARTESIAN_POINT('Ctrl Pts',(-0.38870776678985,-0.179101214295747,
7.4440154873356E-17));
#43815=CARTESIAN_POINT('Ctrl Pts',(-0.391791940744699,-0.17365352637825,
7.3696258065194E-17));
#43816=CARTESIAN_POINT('Ctrl Pts',(-0.394757285743178,-0.168149505204942,
6.93889390390723E-17));
#43817=CARTESIAN_POINT('Ctrl Pts',(-0.406042481613924,-0.147202884474678,
5.29966005717066E-17));
#43818=CARTESIAN_POINT('Ctrl Pts',(-0.415636815927215,-0.12539890172167,
1.40125039712718E-17));
#43819=CARTESIAN_POINT('Ctrl Pts',(-0.423478528957865,-0.102985404860791,
2.77555756156289E-17));
#43820=CARTESIAN_POINT('Ctrl Pts',(-0.429376839283599,-0.0861266191014051,
3.80927176495664E-17));
#43821=CARTESIAN_POINT('Ctrl Pts',(-0.434283049989256,-0.0689218306178823,
5.65608473286771E-17));
#43822=CARTESIAN_POINT('Ctrl Pts',(-0.43815575437846,-0.0514644871269222,
4.5102810375397E-17));
#43823=CARTESIAN_POINT('Ctrl Pts',(-0.439906400633787,-0.0435729390150655,
3.99232336585234E-17));
#43824=CARTESIAN_POINT('Ctrl Pts',(-0.44144565613257,-0.0356296777440409,
6.15140867947257E-17));
#43825=CARTESIAN_POINT('Ctrl Pts',(-0.442768644909789,-0.0276429456528638,
5.89805981832114E-17));
#43826=CARTESIAN_POINT('Ctrl Pts',(-0.443871289745052,-0.0209864047640719,
5.68690624084653E-17));
#43827=CARTESIAN_POINT('Ctrl Pts',(-0.44482365403208,-0.0142978621335312,
3.1313155957869E-17));
#43828=CARTESIAN_POINT('Ctrl Pts',(-0.445620686304564,-0.00760396509680276,
3.81639164714898E-17));
#43829=CARTESIAN_POINT('Ctrl Pts',(-0.448419947719333,0.015905707392318,
6.22245100379753E-17));
#43830=CARTESIAN_POINT('Ctrl Pts',(-0.449317353814376,0.039538445055359,
1.16772899686138E-16));
#43831=CARTESIAN_POINT('Ctrl Pts',(-0.44823656490343,0.0630780692117099,
1.04083408558608E-16));
#43832=CARTESIAN_POINT('Ctrl Pts',(-0.447374340120413,0.081857358233785,
9.47489001442916E-17));
#43833=CARTESIAN_POINT('Ctrl Pts',(-0.445252620327562,0.100578184059543,
7.52302054080897E-18));
#43834=CARTESIAN_POINT('Ctrl Pts',(-0.441939735912287,0.119138777262726,
-6.93889390390723E-18));
#43835=CARTESIAN_POINT('Ctrl Pts',(-0.440350972534721,0.128039899985618,
-1.38744090499585E-17));
#43836=CARTESIAN_POINT('Ctrl Pts',(-0.438487949296401,0.136904200117995,
7.29844862664086E-17));
#43837=CARTESIAN_POINT('Ctrl Pts',(-0.436356577222032,0.145720408589059,
7.28583859910259E-17));
#43838=CARTESIAN_POINT('Ctrl Pts',(-0.434687913405322,0.152622670401133,
7.27596613387989E-17));
#43839=CARTESIAN_POINT('Ctrl Pts',(-0.43285383314019,0.159497658516508,
1.23405815283735E-18));
#43840=CARTESIAN_POINT('Ctrl Pts',(-0.430864188011168,0.166317151368737,
0.));
#43841=CARTESIAN_POINT('Ctrl Pts',(-0.423921464110642,0.190113282308881,
-4.30615736814992E-18));
#43842=CARTESIAN_POINT('Ctrl Pts',(-0.415075878758636,0.213293450260572,
-2.85677649743916E-17));
#43843=CARTESIAN_POINT('Ctrl Pts',(-0.404491724583964,0.235635990622313,
-2.08166817117217E-17));
#43844=CARTESIAN_POINT('Ctrl Pts',(-0.397747393951119,0.249872884462906,
-1.5877612663459E-17));
#43845=CARTESIAN_POINT('Ctrl Pts',(-0.390295993937811,0.263769868300252,
5.84132300429329E-17));
#43846=CARTESIAN_POINT('Ctrl Pts',(-0.382169143027842,0.277268407825058,
6.93889390390723E-17));
#43847=CARTESIAN_POINT('Ctrl Pts',(-0.375587981126775,0.288199588306262,
7.8277119551156E-17));
#43848=CARTESIAN_POINT('Ctrl Pts',(-0.368563698892631,0.298869479267404,
6.83778588982247E-18));
#43849=CARTESIAN_POINT('Ctrl Pts',(-0.36111404718269,0.309257673710277,
-6.93889390390723E-18));
#43850=CARTESIAN_POINT('Ctrl Pts',(-0.356830943331032,0.315230263753738,
-1.4859660214209E-17));
#43851=CARTESIAN_POINT('Ctrl Pts',(-0.352405080449604,0.32111196869177,
8.37777440281965E-17));
#43852=CARTESIAN_POINT('Ctrl Pts',(-0.347855489317613,0.326879369584256,
8.32667268468867E-17));
#43853=CARTESIAN_POINT('Ctrl Pts',(-0.332050949477965,0.346914382518844,
8.14915362492162E-17));
#43854=CARTESIAN_POINT('Ctrl Pts',(-0.314723541600508,0.365621295399423,
6.08259975105604E-18));
#43855=CARTESIAN_POINT('Ctrl Pts',(-0.296050162210069,0.382860211578897,
2.08166817117217E-17));
#43856=CARTESIAN_POINT('Ctrl Pts',(-0.277394780843452,0.400082512317878,
3.55365624743834E-17));
#43857=CARTESIAN_POINT('Ctrl Pts',(-0.257395271430084,0.415840722974244,
5.73069542662832E-17));
#43858=CARTESIAN_POINT('Ctrl Pts',(-0.236184952673479,0.429968144128177,
6.24500451351651E-17));
#43859=CARTESIAN_POINT('Ctrl Pts',(-0.229843975137141,0.434191638419397,
6.39876091878868E-17));
#43860=CARTESIAN_POINT('Ctrl Pts',(-0.223394530553168,0.43826913492392,
3.92474881692199E-17));
#43861=CARTESIAN_POINT('Ctrl Pts',(-0.216839587231054,0.442195480991683,
4.16333634234434E-17));
#43862=CARTESIAN_POINT('Origin',(0.,0.,0.));
#43863=CARTESIAN_POINT('Origin',(-0.144337567297407,-0.25,-0.2));
#43864=CARTESIAN_POINT('',(-0.144337567297407,-0.25,-0.2));
#43865=CARTESIAN_POINT('',(0.144337567297406,-0.25,-0.2));
#43866=CARTESIAN_POINT('',(-0.0721687836487033,-0.25,-0.2));
#43867=CARTESIAN_POINT('',(-0.144337567297407,-0.25,-0.1));
#43868=CARTESIAN_POINT('',(-0.144337567297407,-0.25,-0.2));
#43869=CARTESIAN_POINT('',(0.144337567297406,-0.25,-0.1));
#43870=CARTESIAN_POINT('',(-0.144337567297407,-0.25,-0.1));
#43871=CARTESIAN_POINT('',(0.144337567297406,-0.25,-0.2));
#43872=CARTESIAN_POINT('Origin',(-0.288675134594813,3.53525079574969E-17,
-0.2));
#43873=CARTESIAN_POINT('',(-0.288675134594813,3.53525079574969E-17,-0.2));
#43874=CARTESIAN_POINT('',(-0.252590742770461,-0.0625,-0.2));
#43875=CARTESIAN_POINT('',(-0.288675134594813,5.55111512312578E-17,-0.1));
#43876=CARTESIAN_POINT('',(-0.288675134594813,3.53525079574969E-17,-0.2));
#43877=CARTESIAN_POINT('',(-0.288675134594813,3.53525079574969E-17,-0.1));
#43878=CARTESIAN_POINT('Origin',(-0.144337567297406,0.25,-0.2));
#43879=CARTESIAN_POINT('',(-0.144337567297406,0.25,-0.2));
#43880=CARTESIAN_POINT('',(-0.180421959121758,0.1875,-0.2));
#43881=CARTESIAN_POINT('',(-0.144337567297406,0.25,-0.1));
#43882=CARTESIAN_POINT('',(-0.144337567297406,0.25,-0.2));
#43883=CARTESIAN_POINT('',(-0.144337567297406,0.25,-0.1));
#43884=CARTESIAN_POINT('Origin',(0.144337567297406,0.25,-0.2));
#43885=CARTESIAN_POINT('',(0.144337567297406,0.25,-0.2));
#43886=CARTESIAN_POINT('',(0.0721687836487033,0.25,-0.2));
#43887=CARTESIAN_POINT('',(0.144337567297406,0.25,-0.1));
#43888=CARTESIAN_POINT('',(0.144337567297406,0.25,-0.2));
#43889=CARTESIAN_POINT('',(0.144337567297406,0.25,-0.1));
#43890=CARTESIAN_POINT('Origin',(0.288675134594813,0.,-0.2));
#43891=CARTESIAN_POINT('',(0.288675134594813,0.,-0.2));
#43892=CARTESIAN_POINT('',(0.252590742770461,0.0625,-0.2));
#43893=CARTESIAN_POINT('',(0.288675134594813,0.,-0.1));
#43894=CARTESIAN_POINT('',(0.288675134594813,0.,-0.2));
#43895=CARTESIAN_POINT('',(0.288675134594813,0.,-0.1));
#43896=CARTESIAN_POINT('Origin',(0.144337567297406,-0.25,-0.2));
#43897=CARTESIAN_POINT('',(0.180421959121758,-0.1875,-0.2));
#43898=CARTESIAN_POINT('',(0.144337567297406,-0.25,-0.1));
#43899=CARTESIAN_POINT('Origin',(0.,0.,-0.1));
#43900=CARTESIAN_POINT('Origin',(0.,0.,0.));
#43901=CARTESIAN_POINT('',(-0.6,-7.34788079488412E-17,0.));
#43902=CARTESIAN_POINT('Origin',(0.,0.,0.));
#43903=CARTESIAN_POINT('Origin',(0.,0.,-0.2));
#43904=CARTESIAN_POINT('',(-0.6,-7.34788079488412E-17,-0.2));
#43905=CARTESIAN_POINT('',(-0.6,-7.34788079488412E-17,-0.2));
#43906=CARTESIAN_POINT('Origin',(0.,0.,-0.2));
#43907=CARTESIAN_POINT('Origin',(0.,0.,-0.2));
#43908=CARTESIAN_POINT('Origin',(0.,0.,0.4));
#43909=CARTESIAN_POINT('',(0.,0.,0.));
#43910=CARTESIAN_POINT('',(0.,0.,0.));
#43911=CARTESIAN_POINT('',(0.,-2.8,2.2));
#43912=CARTESIAN_POINT('',(-1.83697019872103E-16,2.24028564144024E-16,0.));
#43913=CARTESIAN_POINT('',(-1.83697019872103E-16,2.24028564144024E-16,0.));
#43914=CARTESIAN_POINT('',(-1.83697019872103E-16,2.24028564144024E-16,0.));
#43915=CARTESIAN_POINT('',(2.4,1.,0.));
#43916=CARTESIAN_POINT('',(1.4,1.,0.));
#43917=CARTESIAN_POINT('',(1.4,1.,0.));
#43918=CARTESIAN_POINT('',(0.726794919243112,0.,6.4));
#43919=CARTESIAN_POINT('',(0.926794919243112,0.,6.4));
#43920=CARTESIAN_POINT('',(0.,0.,0.85));
#43921=CARTESIAN_POINT('',(-2.4,1.,0.));
#43922=CARTESIAN_POINT('',(-1.4,1.,0.));
#43923=CARTESIAN_POINT('',(-1.4,1.,0.));
#43924=CARTESIAN_POINT('',(-0.726794919243112,0.,6.4));
#43925=CARTESIAN_POINT('',(-0.926794919243112,0.,6.4));
#43926=CARTESIAN_POINT('',(2.15,0.,6.4));
#43927=CARTESIAN_POINT('',(-3.6,-2.4,5.8));
#43928=CARTESIAN_POINT('',(-0.6,1.,2.6));
#43929=CARTESIAN_POINT('',(2.4,1.,4.));
#43930=CARTESIAN_POINT('',(2.6,0.,6.4));
#43931=CARTESIAN_POINT('',(-2.15,0.,6.4));
#43932=CARTESIAN_POINT('',(-3.6,2.4,5.8));
#43933=CARTESIAN_POINT('',(3.6,-2.4,5.8));
#43934=CARTESIAN_POINT('',(3.6,2.4,5.8));
#43935=CARTESIAN_POINT('',(-2.4,1.,0.4));
#43936=CARTESIAN_POINT('',(2.4,1.,0.4));
#43937=CARTESIAN_POINT('',(9.26526004753054E-16,4.50093621765325E-16,9.));
#43938=CARTESIAN_POINT('',(0.6,1.,2.6));
#43939=CARTESIAN_POINT('',(-1.4,1.,4.2));
#43940=CARTESIAN_POINT('',(1.4,1.,4.2));
#43941=CARTESIAN_POINT('',(-2.4,1.,4.));
#43942=CARTESIAN_POINT('',(-2.6,0.,6.4));
#43943=UNCERTAINTY_MEASURE_WITH_UNIT(LENGTH_MEASURE(0.001),#43981,
'DISTANCE_ACCURACY_VALUE',
'Maximum model space distance between geometric entities at asserted c
onnectivities');
#43944=UNCERTAINTY_MEASURE_WITH_UNIT(LENGTH_MEASURE(0.001),#43981,
'DISTANCE_ACCURACY_VALUE',
'Maximum model space distance between geometric entities at asserted c
onnectivities');
#43945=UNCERTAINTY_MEASURE_WITH_UNIT(LENGTH_MEASURE(0.001),#43981,
'DISTANCE_ACCURACY_VALUE',
'Maximum model space distance between geometric entities at asserted c
onnectivities');
#43946=UNCERTAINTY_MEASURE_WITH_UNIT(LENGTH_MEASURE(0.001),#43981,
'DISTANCE_ACCURACY_VALUE',
'Maximum model space distance between geometric entities at asserted c
onnectivities');
#43947=UNCERTAINTY_MEASURE_WITH_UNIT(LENGTH_MEASURE(0.001),#43981,
'DISTANCE_ACCURACY_VALUE',
'Maximum model space distance between geometric entities at asserted c
onnectivities');
#43948=UNCERTAINTY_MEASURE_WITH_UNIT(LENGTH_MEASURE(0.001),#43981,
'DISTANCE_ACCURACY_VALUE',
'Maximum model space distance between geometric entities at asserted c
onnectivities');
#43949=UNCERTAINTY_MEASURE_WITH_UNIT(LENGTH_MEASURE(0.001),#43981,
'DISTANCE_ACCURACY_VALUE',
'Maximum model space distance between geometric entities at asserted c
onnectivities');
#43950=UNCERTAINTY_MEASURE_WITH_UNIT(LENGTH_MEASURE(0.001),#43981,
'DISTANCE_ACCURACY_VALUE',
'Maximum model space distance between geometric entities at asserted c
onnectivities');
#43951=UNCERTAINTY_MEASURE_WITH_UNIT(LENGTH_MEASURE(0.001),#43981,
'DISTANCE_ACCURACY_VALUE',
'Maximum model space distance between geometric entities at asserted c
onnectivities');
#43952=UNCERTAINTY_MEASURE_WITH_UNIT(LENGTH_MEASURE(0.001),#43981,
'DISTANCE_ACCURACY_VALUE',
'Maximum model space distance between geometric entities at asserted c
onnectivities');
#43953=UNCERTAINTY_MEASURE_WITH_UNIT(LENGTH_MEASURE(0.001),#43981,
'DISTANCE_ACCURACY_VALUE',
'Maximum model space distance between geometric entities at asserted c
onnectivities');
#43954=UNCERTAINTY_MEASURE_WITH_UNIT(LENGTH_MEASURE(0.001),#43981,
'DISTANCE_ACCURACY_VALUE',
'Maximum model space distance between geometric entities at asserted c
onnectivities');
#43955=UNCERTAINTY_MEASURE_WITH_UNIT(LENGTH_MEASURE(0.001),#43981,
'DISTANCE_ACCURACY_VALUE',
'Maximum model space distance between geometric entities at asserted c
onnectivities');
#43956=UNCERTAINTY_MEASURE_WITH_UNIT(LENGTH_MEASURE(0.001),#43981,
'DISTANCE_ACCURACY_VALUE',
'Maximum model space distance between geometric entities at asserted c
onnectivities');
#43957=UNCERTAINTY_MEASURE_WITH_UNIT(LENGTH_MEASURE(0.001),#43981,
'DISTANCE_ACCURACY_VALUE',
'Maximum model space distance between geometric entities at asserted c
onnectivities');
#43958=UNCERTAINTY_MEASURE_WITH_UNIT(LENGTH_MEASURE(0.001),#43981,
'DISTANCE_ACCURACY_VALUE',
'Maximum model space distance between geometric entities at asserted c
onnectivities');
#43959=UNCERTAINTY_MEASURE_WITH_UNIT(LENGTH_MEASURE(0.001),#43981,
'DISTANCE_ACCURACY_VALUE',
'Maximum model space distance between geometric entities at asserted c
onnectivities');
#43960=UNCERTAINTY_MEASURE_WITH_UNIT(LENGTH_MEASURE(0.001),#43981,
'DISTANCE_ACCURACY_VALUE',
'Maximum model space distance between geometric entities at asserted c
onnectivities');
#43961=UNCERTAINTY_MEASURE_WITH_UNIT(LENGTH_MEASURE(0.001),#43981,
'DISTANCE_ACCURACY_VALUE',
'Maximum model space distance between geometric entities at asserted c
onnectivities');
#43962=(
GEOMETRIC_REPRESENTATION_CONTEXT(3)
GLOBAL_UNCERTAINTY_ASSIGNED_CONTEXT((#43943))
GLOBAL_UNIT_ASSIGNED_CONTEXT((#43981,#43983,#43984))
REPRESENTATION_CONTEXT('','3D')
);
#43963=(
GEOMETRIC_REPRESENTATION_CONTEXT(3)
GLOBAL_UNCERTAINTY_ASSIGNED_CONTEXT((#43944))
GLOBAL_UNIT_ASSIGNED_CONTEXT((#43981,#43983,#43984))
REPRESENTATION_CONTEXT('','3D')
);
#43964=(
GEOMETRIC_REPRESENTATION_CONTEXT(3)
GLOBAL_UNCERTAINTY_ASSIGNED_CONTEXT((#43945))
GLOBAL_UNIT_ASSIGNED_CONTEXT((#43981,#43983,#43984))
REPRESENTATION_CONTEXT('','3D')
);
#43965=(
GEOMETRIC_REPRESENTATION_CONTEXT(3)
GLOBAL_UNCERTAINTY_ASSIGNED_CONTEXT((#43946))
GLOBAL_UNIT_ASSIGNED_CONTEXT((#43981,#43983,#43984))
REPRESENTATION_CONTEXT('','3D')
);
#43966=(
GEOMETRIC_REPRESENTATION_CONTEXT(3)
GLOBAL_UNCERTAINTY_ASSIGNED_CONTEXT((#43947))
GLOBAL_UNIT_ASSIGNED_CONTEXT((#43981,#43983,#43984))
REPRESENTATION_CONTEXT('','3D')
);
#43967=(
GEOMETRIC_REPRESENTATION_CONTEXT(3)
GLOBAL_UNCERTAINTY_ASSIGNED_CONTEXT((#43948))
GLOBAL_UNIT_ASSIGNED_CONTEXT((#43981,#43983,#43984))
REPRESENTATION_CONTEXT('','3D')
);
#43968=(
GEOMETRIC_REPRESENTATION_CONTEXT(3)
GLOBAL_UNCERTAINTY_ASSIGNED_CONTEXT((#43949))
GLOBAL_UNIT_ASSIGNED_CONTEXT((#43981,#43983,#43984))
REPRESENTATION_CONTEXT('','3D')
);
#43969=(
GEOMETRIC_REPRESENTATION_CONTEXT(3)
GLOBAL_UNCERTAINTY_ASSIGNED_CONTEXT((#43950))
GLOBAL_UNIT_ASSIGNED_CONTEXT((#43981,#43983,#43984))
REPRESENTATION_CONTEXT('','3D')
);
#43970=(
GEOMETRIC_REPRESENTATION_CONTEXT(3)
GLOBAL_UNCERTAINTY_ASSIGNED_CONTEXT((#43951))
GLOBAL_UNIT_ASSIGNED_CONTEXT((#43981,#43983,#43984))
REPRESENTATION_CONTEXT('','3D')
);
#43971=(
GEOMETRIC_REPRESENTATION_CONTEXT(3)
GLOBAL_UNCERTAINTY_ASSIGNED_CONTEXT((#43952))
GLOBAL_UNIT_ASSIGNED_CONTEXT((#43981,#43983,#43984))
REPRESENTATION_CONTEXT('','3D')
);
#43972=(
GEOMETRIC_REPRESENTATION_CONTEXT(3)
GLOBAL_UNCERTAINTY_ASSIGNED_CONTEXT((#43953))
GLOBAL_UNIT_ASSIGNED_CONTEXT((#43981,#43983,#43984))
REPRESENTATION_CONTEXT('','3D')
);
#43973=(
GEOMETRIC_REPRESENTATION_CONTEXT(3)
GLOBAL_UNCERTAINTY_ASSIGNED_CONTEXT((#43954))
GLOBAL_UNIT_ASSIGNED_CONTEXT((#43981,#43983,#43984))
REPRESENTATION_CONTEXT('','3D')
);
#43974=(
GEOMETRIC_REPRESENTATION_CONTEXT(3)
GLOBAL_UNCERTAINTY_ASSIGNED_CONTEXT((#43955))
GLOBAL_UNIT_ASSIGNED_CONTEXT((#43981,#43983,#43984))
REPRESENTATION_CONTEXT('','3D')
);
#43975=(
GEOMETRIC_REPRESENTATION_CONTEXT(3)
GLOBAL_UNCERTAINTY_ASSIGNED_CONTEXT((#43956))
GLOBAL_UNIT_ASSIGNED_CONTEXT((#43981,#43983,#43984))
REPRESENTATION_CONTEXT('','3D')
);
#43976=(
GEOMETRIC_REPRESENTATION_CONTEXT(3)
GLOBAL_UNCERTAINTY_ASSIGNED_CONTEXT((#43957))
GLOBAL_UNIT_ASSIGNED_CONTEXT((#43981,#43983,#43984))
REPRESENTATION_CONTEXT('','3D')
);
#43977=(
GEOMETRIC_REPRESENTATION_CONTEXT(3)
GLOBAL_UNCERTAINTY_ASSIGNED_CONTEXT((#43958))
GLOBAL_UNIT_ASSIGNED_CONTEXT((#43981,#43983,#43984))
REPRESENTATION_CONTEXT('','3D')
);
#43978=(
GEOMETRIC_REPRESENTATION_CONTEXT(3)
GLOBAL_UNCERTAINTY_ASSIGNED_CONTEXT((#43959))
GLOBAL_UNIT_ASSIGNED_CONTEXT((#43981,#43983,#43984))
REPRESENTATION_CONTEXT('','3D')
);
#43979=(
GEOMETRIC_REPRESENTATION_CONTEXT(3)
GLOBAL_UNCERTAINTY_ASSIGNED_CONTEXT((#43960))
GLOBAL_UNIT_ASSIGNED_CONTEXT((#43981,#43983,#43984))
REPRESENTATION_CONTEXT('','3D')
);
#43980=(
GEOMETRIC_REPRESENTATION_CONTEXT(3)
GLOBAL_UNCERTAINTY_ASSIGNED_CONTEXT((#43961))
GLOBAL_UNIT_ASSIGNED_CONTEXT((#43981,#43983,#43984))
REPRESENTATION_CONTEXT('','3D')
);
#43981=(
LENGTH_UNIT()
NAMED_UNIT(*)
SI_UNIT(.CENTI.,.METRE.)
);
#43982=(
LENGTH_UNIT()
NAMED_UNIT(*)
SI_UNIT($,.METRE.)
);
#43983=(
NAMED_UNIT(*)
PLANE_ANGLE_UNIT()
SI_UNIT($,.RADIAN.)
);
#43984=(
NAMED_UNIT(*)
SI_UNIT($,.STERADIAN.)
SOLID_ANGLE_UNIT()
);
#43985=SHAPE_DEFINITION_REPRESENTATION(#44003,#44055);
#43986=SHAPE_DEFINITION_REPRESENTATION(#44004,#44056);
#43987=SHAPE_DEFINITION_REPRESENTATION(#44005,#44057);
#43988=SHAPE_DEFINITION_REPRESENTATION(#44006,#44058);
#43989=SHAPE_DEFINITION_REPRESENTATION(#44007,#44059);
#43990=SHAPE_DEFINITION_REPRESENTATION(#44008,#44060);
#43991=SHAPE_DEFINITION_REPRESENTATION(#44009,#44061);
#43992=SHAPE_DEFINITION_REPRESENTATION(#44010,#44062);
#43993=SHAPE_DEFINITION_REPRESENTATION(#44011,#44063);
#43994=SHAPE_DEFINITION_REPRESENTATION(#44012,#44064);
#43995=SHAPE_DEFINITION_REPRESENTATION(#44013,#44065);
#43996=SHAPE_DEFINITION_REPRESENTATION(#44014,#44066);
#43997=SHAPE_DEFINITION_REPRESENTATION(#44015,#44067);
#43998=SHAPE_DEFINITION_REPRESENTATION(#44016,#44068);
#43999=SHAPE_DEFINITION_REPRESENTATION(#44017,#44069);
#44000=SHAPE_DEFINITION_REPRESENTATION(#44018,#44070);
#44001=SHAPE_DEFINITION_REPRESENTATION(#44019,#44071);
#44002=SHAPE_DEFINITION_REPRESENTATION(#44020,#44072);
#44003=PRODUCT_DEFINITION_SHAPE('',$,#44074);
#44004=PRODUCT_DEFINITION_SHAPE('',$,#44075);
#44005=PRODUCT_DEFINITION_SHAPE('',$,#44076);
#44006=PRODUCT_DEFINITION_SHAPE('',$,#44077);
#44007=PRODUCT_DEFINITION_SHAPE('',$,#44078);
#44008=PRODUCT_DEFINITION_SHAPE('',$,#44079);
#44009=PRODUCT_DEFINITION_SHAPE('',$,#44080);
#44010=PRODUCT_DEFINITION_SHAPE('',$,#44081);
#44011=PRODUCT_DEFINITION_SHAPE('',$,#44082);
#44012=PRODUCT_DEFINITION_SHAPE('',$,#44083);
#44013=PRODUCT_DEFINITION_SHAPE('',$,#44084);
#44014=PRODUCT_DEFINITION_SHAPE('',$,#44085);
#44015=PRODUCT_DEFINITION_SHAPE('',$,#44086);
#44016=PRODUCT_DEFINITION_SHAPE('',$,#44087);
#44017=PRODUCT_DEFINITION_SHAPE('',$,#44088);
#44018=PRODUCT_DEFINITION_SHAPE('',$,#44089);
#44019=PRODUCT_DEFINITION_SHAPE('',$,#44090);
#44020=PRODUCT_DEFINITION_SHAPE('',$,#44091);
#44021=PRODUCT_DEFINITION_SHAPE($,$,#113);
#44022=PRODUCT_DEFINITION_SHAPE($,$,#114);
#44023=PRODUCT_DEFINITION_SHAPE($,$,#115);
#44024=PRODUCT_DEFINITION_SHAPE($,$,#116);
#44025=PRODUCT_DEFINITION_SHAPE($,$,#117);
#44026=PRODUCT_DEFINITION_SHAPE($,$,#118);
#44027=PRODUCT_DEFINITION_SHAPE($,$,#119);
#44028=PRODUCT_DEFINITION_SHAPE($,$,#120);
#44029=PRODUCT_DEFINITION_SHAPE($,$,#121);
#44030=PRODUCT_DEFINITION_SHAPE($,$,#122);
#44031=PRODUCT_DEFINITION_SHAPE($,$,#123);
#44032=PRODUCT_DEFINITION_SHAPE($,$,#124);
#44033=PRODUCT_DEFINITION_SHAPE($,$,#125);
#44034=PRODUCT_DEFINITION_SHAPE($,$,#126);
#44035=PRODUCT_DEFINITION_SHAPE($,$,#127);
#44036=PRODUCT_DEFINITION_SHAPE($,$,#128);
#44037=PRODUCT_DEFINITION_SHAPE($,$,#129);
#44038=PRODUCT_DEFINITION_SHAPE($,$,#130);
#44039=PRODUCT_DEFINITION_SHAPE($,$,#131);
#44040=PRODUCT_DEFINITION_SHAPE($,$,#132);
#44041=PRODUCT_DEFINITION_SHAPE($,$,#133);
#44042=PRODUCT_DEFINITION_SHAPE($,$,#134);
#44043=PRODUCT_DEFINITION_SHAPE($,$,#135);
#44044=PRODUCT_DEFINITION_SHAPE($,$,#136);
#44045=PRODUCT_DEFINITION_SHAPE($,$,#137);
#44046=PRODUCT_DEFINITION_SHAPE($,$,#138);
#44047=PRODUCT_DEFINITION_SHAPE($,$,#139);
#44048=PRODUCT_DEFINITION_SHAPE($,$,#140);
#44049=PRODUCT_DEFINITION_SHAPE($,$,#141);
#44050=PRODUCT_DEFINITION_SHAPE($,$,#142);
#44051=PRODUCT_DEFINITION_SHAPE($,$,#143);
#44052=PRODUCT_DEFINITION_SHAPE($,$,#144);
#44053=PRODUCT_DEFINITION_SHAPE($,$,#145);
#44054=PRODUCT_DEFINITION_SHAPE($,$,#146);
#44055=SHAPE_REPRESENTATION('',(#11436,#12233,#12234,#12235,#12236,#12237,
#12238,#12239,#12240,#12241,#12242,#12243,#12244,#12245,#12246,#12247,#12248,
#12249,#12250,#12251,#12252,#12253,#12254,#12255,#12256,#12257,#12258,#12259,
#12260,#12261,#12262,#12263,#12264,#12265,#12266),#43962);
#44056=SHAPE_REPRESENTATION('',(#11437),#43963);
#44057=SHAPE_REPRESENTATION('',(#11636),#43964);
#44058=SHAPE_REPRESENTATION('',(#11727),#43965);
#44059=SHAPE_REPRESENTATION('',(#11740),#43966);
#44060=SHAPE_REPRESENTATION('',(#11851),#43967);
#44061=SHAPE_REPRESENTATION('',(#11878),#43968);
#44062=SHAPE_REPRESENTATION('',(#11891),#43969);
#44063=SHAPE_REPRESENTATION('',(#11896),#43970);
#44064=SHAPE_REPRESENTATION('',(#11983),#43971);
#44065=SHAPE_REPRESENTATION('',(#12025),#43972);
#44066=SHAPE_REPRESENTATION('',(#12035),#43973);
#44067=SHAPE_REPRESENTATION('',(#12038),#43974);
#44068=SHAPE_REPRESENTATION('',(#12048),#43975);
#44069=SHAPE_REPRESENTATION('',(#12053),#43976);
#44070=SHAPE_REPRESENTATION('',(#12107),#43977);
#44071=SHAPE_REPRESENTATION('',(#12149),#43978);
#44072=SHAPE_REPRESENTATION('',(#12207),#43979);
#44073=PRODUCT_DEFINITION_CONTEXT('part definition',#44129,'design');
#44074=PRODUCT_DEFINITION('MAS-639','MAS-639',#44092,#44073);
#44075=PRODUCT_DEFINITION('Switch housing','Switch housing',#44093,#44073);
#44076=PRODUCT_DEFINITION('Housing cover','Housing cover',#44094,#44073);
#44077=PRODUCT_DEFINITION('Cable entry seal','Cable entry seal',#44095,
#44073);
#44078=PRODUCT_DEFINITION('Button actuator','Button actuator',#44096,#44073);
#44079=PRODUCT_DEFINITION('Mushroom head','Mushroom head',#44097,#44073);
#44080=PRODUCT_DEFINITION('Moving contact bridge',
'Moving contact bridge',#44098,#44073);
#44081=PRODUCT_DEFINITION('Return Spring','Return spring',#44099,#44073);
#44082=PRODUCT_DEFINITION('Terminal insulator','Terminal insulator',#44100,
#44073);
#44083=PRODUCT_DEFINITION('Fixed contact terminal',
'Fixed contact terminal',#44101,#44073);
#44084=PRODUCT_DEFINITION('Terminal clamp plate','Terminal clamp plate',
#44102,#44073);
#44085=PRODUCT_DEFINITION('Detent ball','Detent ball',#44103,#44073);
#44086=PRODUCT_DEFINITION('Detent plunger','Detent plunger',#44104,#44073);
#44087=PRODUCT_DEFINITION('Detent spring','Detent spring',#44105,#44073);
#44088=PRODUCT_DEFINITION('Socket head cap screw M4x12',
'Socket head cap screw M4x12',#44106,#44073);
#44089=PRODUCT_DEFINITION('Socket head cap screw M3x6',
'Socket head cap screw M3x6',#44107,#44073);
#44090=PRODUCT_DEFINITION('Socket head cap screw M3x10',
'Socket head cap screw M3x10',#44108,#44073);
#44091=PRODUCT_DEFINITION('Socket head cap screw M10x4',
'Socket head cap screw M10x4',#44109,#44073);
#44092=PRODUCT_DEFINITION_FORMATION('',$,#44131);
#44093=PRODUCT_DEFINITION_FORMATION('',$,#44132);
#44094=PRODUCT_DEFINITION_FORMATION('',$,#44133);
#44095=PRODUCT_DEFINITION_FORMATION('',$,#44134);
#44096=PRODUCT_DEFINITION_FORMATION('',$,#44135);
#44097=PRODUCT_DEFINITION_FORMATION('',$,#44136);
#44098=PRODUCT_DEFINITION_FORMATION('',$,#44137);
#44099=PRODUCT_DEFINITION_FORMATION('',$,#44138);
#44100=PRODUCT_DEFINITION_FORMATION('',$,#44139);
#44101=PRODUCT_DEFINITION_FORMATION('',$,#44140);
#44102=PRODUCT_DEFINITION_FORMATION('',$,#44141);
#44103=PRODUCT_DEFINITION_FORMATION('',$,#44142);
#44104=PRODUCT_DEFINITION_FORMATION('',$,#44143);
#44105=PRODUCT_DEFINITION_FORMATION('',$,#44144);
#44106=PRODUCT_DEFINITION_FORMATION('',$,#44145);
#44107=PRODUCT_DEFINITION_FORMATION('',$,#44146);
#44108=PRODUCT_DEFINITION_FORMATION('',$,#44147);
#44109=PRODUCT_DEFINITION_FORMATION('',$,#44148);
#44110=PRODUCT_RELATED_PRODUCT_CATEGORY('MAS-639','MAS-639',(#44131));
#44111=PRODUCT_RELATED_PRODUCT_CATEGORY('Switch housing',
'Switch housing',(#44132));
#44112=PRODUCT_RELATED_PRODUCT_CATEGORY('Housing cover','Housing cover',
(#44133));
#44113=PRODUCT_RELATED_PRODUCT_CATEGORY('Cable entry seal',
'Cable entry seal',(#44134));
#44114=PRODUCT_RELATED_PRODUCT_CATEGORY('Button actuator',
'Button actuator',(#44135));
#44115=PRODUCT_RELATED_PRODUCT_CATEGORY('Mushroom head','Mushroom head',
(#44136));
#44116=PRODUCT_RELATED_PRODUCT_CATEGORY('Moving contact bridge',
'Moving contact bridge',(#44137));
#44117=PRODUCT_RELATED_PRODUCT_CATEGORY('Return spring','Return spring',
(#44138));
#44118=PRODUCT_RELATED_PRODUCT_CATEGORY('Terminal insulator',
'Terminal insulator',(#44139));
#44119=PRODUCT_RELATED_PRODUCT_CATEGORY('Fixed contact terminal',
'Fixed contact terminal',(#44140));
#44120=PRODUCT_RELATED_PRODUCT_CATEGORY('Terminal clamp plate',
'Terminal clamp plate',(#44141));
#44121=PRODUCT_RELATED_PRODUCT_CATEGORY('Detent ball','Detent ball',(#44142));
#44122=PRODUCT_RELATED_PRODUCT_CATEGORY('Detent plunger',
'Detent plunger',(#44143));
#44123=PRODUCT_RELATED_PRODUCT_CATEGORY('Detent spring','Detent spring',
(#44144));
#44124=PRODUCT_RELATED_PRODUCT_CATEGORY('Socket head cap screw M4x12',
'Socket head cap screw M4x12',(#44145));
#44125=PRODUCT_RELATED_PRODUCT_CATEGORY('Socket head cap screw M3x6',
'Socket head cap screw M3x6',(#44146));
#44126=PRODUCT_RELATED_PRODUCT_CATEGORY('Socket head cap screw M3x10',
'Socket head cap screw M3x10',(#44147));
#44127=PRODUCT_RELATED_PRODUCT_CATEGORY('Socket head cap screw M10x4',
'Socket head cap screw M10x4',(#44148));
#44128=APPLICATION_PROTOCOL_DEFINITION('international standard',
'automotive_design',2009,#44129);
#44129=APPLICATION_CONTEXT(
'Core Data for Automotive Mechanical Design Process');
#44130=PRODUCT_CONTEXT('part definition',#44129,'mechanical');
#44131=PRODUCT('MAS-639','MAS-639',
'Independent maintained push-to-latch/pull-to-reset mushroom-operator 
CAD. Two opposed spring-loaded ball detents in turned circular seats b
ias both travel stops; direct normally-closed bridge opens6mm when pre
ssed. Rounded palm/pull rim, captured head screw, removable detent clo
sures, native Coil spring families, insulated shared terminals and ord
inary machining features. Manual geometric states and ideal same-mater
ial spring-energy direction only; no electrical/safety certification, 
force/contact dynamics, wear, load or life rating. Requested blue/gray
 visual palette, not safety identification. External wiring/anchors an
d application engineering omitted.',(#44130));
#44132=PRODUCT('Switch housing','Switch housing',$,(#44130));
#44133=PRODUCT('Housing cover','Housing cover',$,(#44130));
#44134=PRODUCT('Cable entry seal','Cable entry seal',$,(#44130));
#44135=PRODUCT('Button actuator','Button actuator',$,(#44130));
#44136=PRODUCT('Mushroom head','Mushroom head',$,(#44130));
#44137=PRODUCT('Moving contact bridge','Moving contact bridge',$,(#44130));
#44138=PRODUCT('Return Spring','Return spring',$,(#44130));
#44139=PRODUCT('Terminal insulator','Terminal insulator',$,(#44130));
#44140=PRODUCT('Fixed contact terminal','Fixed contact terminal',$,(#44130));
#44141=PRODUCT('Terminal clamp plate','Terminal clamp plate',$,(#44130));
#44142=PRODUCT('Detent ball','Detent ball','Detent ball',(#44130));
#44143=PRODUCT('Detent plunger','Detent plunger',$,(#44130));
#44144=PRODUCT('Detent spring','Detent spring','Detent spring',(#44130));
#44145=PRODUCT('Socket head cap screw M4x12',
'Socket head cap screw M4x12',$,(#44130));
#44146=PRODUCT('Socket head cap screw M3x6',
'Socket head cap screw M3x6',$,(#44130));
#44147=PRODUCT('Socket head cap screw M3x10',
'Socket head cap screw M3x10',$,(#44130));
#44148=PRODUCT('Socket head cap screw M10x4',
'Socket head cap screw M10x4',$,(#44130));
#44149=PRESENTATION_STYLE_ASSIGNMENT((#44161));
#44150=PRESENTATION_STYLE_ASSIGNMENT((#44162));
#44151=PRESENTATION_STYLE_ASSIGNMENT((#44163));
#44152=PRESENTATION_STYLE_ASSIGNMENT((#44164));
#44153=PRESENTATION_STYLE_ASSIGNMENT((#44165));
#44154=PRESENTATION_STYLE_ASSIGNMENT((#44166));
#44155=PRESENTATION_STYLE_ASSIGNMENT((#44167));
#44156=PRESENTATION_STYLE_ASSIGNMENT((#44168));
#44157=PRESENTATION_STYLE_ASSIGNMENT((#44169));
#44158=PRESENTATION_STYLE_ASSIGNMENT((#44170));
#44159=PRESENTATION_STYLE_ASSIGNMENT((#44171));
#44160=PRESENTATION_STYLE_ASSIGNMENT((#44172));
#44161=SURFACE_STYLE_USAGE(.BOTH.,#44173);
#44162=SURFACE_STYLE_USAGE(.BOTH.,#44174);
#44163=SURFACE_STYLE_USAGE(.BOTH.,#44175);
#44164=SURFACE_STYLE_USAGE(.BOTH.,#44176);
#44165=SURFACE_STYLE_USAGE(.BOTH.,#44177);
#44166=SURFACE_STYLE_USAGE(.BOTH.,#44178);
#44167=SURFACE_STYLE_USAGE(.BOTH.,#44179);
#44168=SURFACE_STYLE_USAGE(.BOTH.,#44180);
#44169=SURFACE_STYLE_USAGE(.BOTH.,#44181);
#44170=SURFACE_STYLE_USAGE(.BOTH.,#44182);
#44171=SURFACE_STYLE_USAGE(.BOTH.,#44183);
#44172=SURFACE_STYLE_USAGE(.BOTH.,#44184);
#44173=SURFACE_SIDE_STYLE('',(#44185));
#44174=SURFACE_SIDE_STYLE('',(#44186));
#44175=SURFACE_SIDE_STYLE('',(#44187));
#44176=SURFACE_SIDE_STYLE('',(#44188));
#44177=SURFACE_SIDE_STYLE('',(#44189));
#44178=SURFACE_SIDE_STYLE('',(#44190));
#44179=SURFACE_SIDE_STYLE('',(#44191));
#44180=SURFACE_SIDE_STYLE('',(#44192));
#44181=SURFACE_SIDE_STYLE('',(#44193));
#44182=SURFACE_SIDE_STYLE('',(#44194));
#44183=SURFACE_SIDE_STYLE('',(#44195));
#44184=SURFACE_SIDE_STYLE('',(#44196));
#44185=SURFACE_STYLE_FILL_AREA(#44197);
#44186=SURFACE_STYLE_FILL_AREA(#44198);
#44187=SURFACE_STYLE_FILL_AREA(#44199);
#44188=SURFACE_STYLE_FILL_AREA(#44200);
#44189=SURFACE_STYLE_FILL_AREA(#44201);
#44190=SURFACE_STYLE_FILL_AREA(#44202);
#44191=SURFACE_STYLE_FILL_AREA(#44203);
#44192=SURFACE_STYLE_FILL_AREA(#44204);
#44193=SURFACE_STYLE_FILL_AREA(#44205);
#44194=SURFACE_STYLE_FILL_AREA(#44206);
#44195=SURFACE_STYLE_FILL_AREA(#44207);
#44196=SURFACE_STYLE_FILL_AREA(#44208);
#44197=FILL_AREA_STYLE('Steel - Satin',(#44209));
#44198=FILL_AREA_STYLE('Dark blue',(#44210));
#44199=FILL_AREA_STYLE('Sky blue',(#44211));
#44200=FILL_AREA_STYLE('Charcoal',(#44212));
#44201=FILL_AREA_STYLE('Light blue',(#44213));
#44202=FILL_AREA_STYLE('Contact gray',(#44214));
#44203=FILL_AREA_STYLE('Spring gray',(#44215));
#44204=FILL_AREA_STYLE('Insulator gray',(#44216));
#44205=FILL_AREA_STYLE('Clamp gray',(#44217));
#44206=FILL_AREA_STYLE('Ball gray',(#44218));
#44207=FILL_AREA_STYLE('Plunger gray',(#44219));
#44208=FILL_AREA_STYLE('Dark gray',(#44220));
#44209=FILL_AREA_STYLE_COLOUR('Steel - Satin',#44221);
#44210=FILL_AREA_STYLE_COLOUR('Dark blue',#44222);
#44211=FILL_AREA_STYLE_COLOUR('Sky blue',#44223);
#44212=FILL_AREA_STYLE_COLOUR('Charcoal',#44224);
#44213=FILL_AREA_STYLE_COLOUR('Light blue',#44225);
#44214=FILL_AREA_STYLE_COLOUR('Contact gray',#44226);
#44215=FILL_AREA_STYLE_COLOUR('Spring gray',#44227);
#44216=FILL_AREA_STYLE_COLOUR('Insulator gray',#44228);
#44217=FILL_AREA_STYLE_COLOUR('Clamp gray',#44229);
#44218=FILL_AREA_STYLE_COLOUR('Ball gray',#44230);
#44219=FILL_AREA_STYLE_COLOUR('Plunger gray',#44231);
#44220=FILL_AREA_STYLE_COLOUR('Dark gray',#44232);
#44221=COLOUR_RGB('Steel - Satin',0.627450980392157,0.627450980392157,0.627450980392157);
#44222=COLOUR_RGB('Dark blue',0.0901960784313725,0.270588235294118,0.513725490196078);
#44223=COLOUR_RGB('Sky blue',0.317647058823529,0.686274509803922,0.890196078431372);
#44224=COLOUR_RGB('Charcoal',0.164705882352941,0.184313725490196,0.211764705882353);
#44225=COLOUR_RGB('Light blue',0.662745098039216,0.831372549019608,0.949019607843137);
#44226=COLOUR_RGB('Contact gray',0.725490196078431,0.752941176470588,0.792156862745098);
#44227=COLOUR_RGB('Spring gray',0.407843137254902,0.447058823529412,0.498039215686275);
#44228=COLOUR_RGB('Insulator gray',0.576470588235294,0.615686274509804,
0.666666666666667);
#44229=COLOUR_RGB('Clamp gray',0.407843137254902,0.447058823529412,0.498039215686275);
#44230=COLOUR_RGB('Ball gray',0.725490196078431,0.752941176470588,0.792156862745098);
#44231=COLOUR_RGB('Plunger gray',0.576470588235294,0.615686274509804,0.666666666666667);
#44232=COLOUR_RGB('Dark gray',0.250980392156863,0.282352941176471,0.32156862745098);
ENDSEC;
END-ISO-10303-21;
